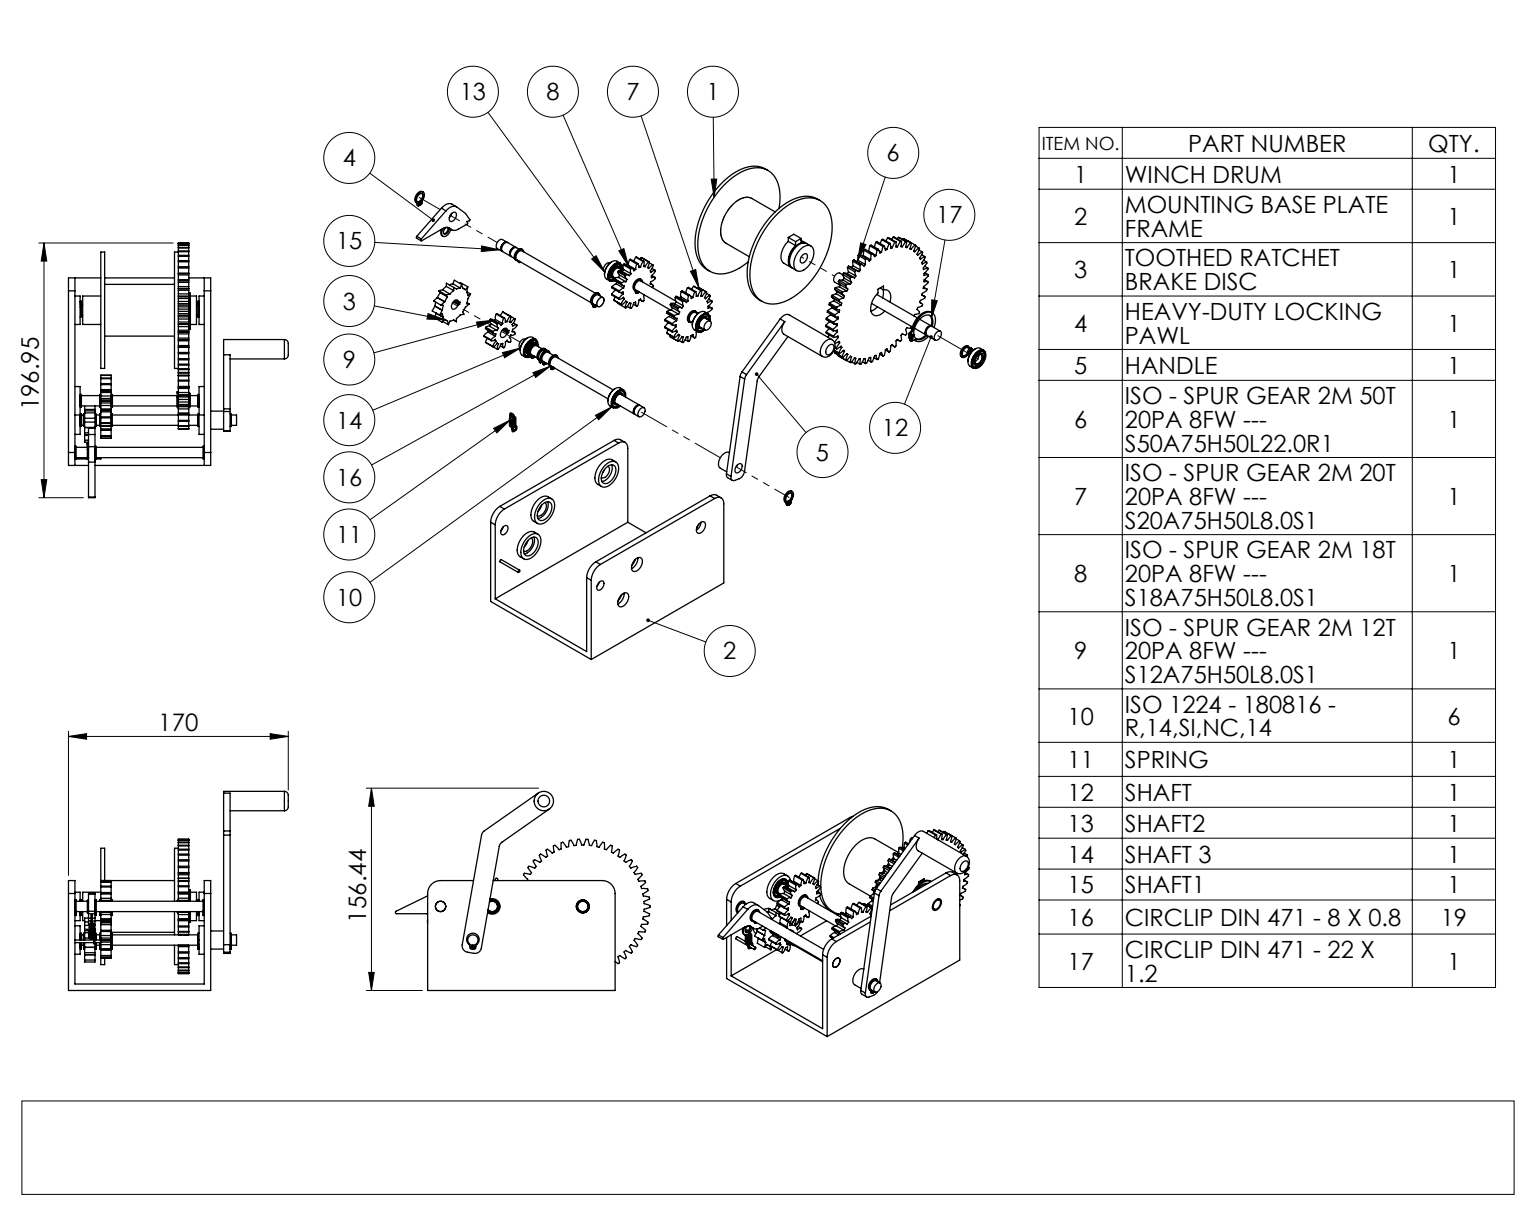
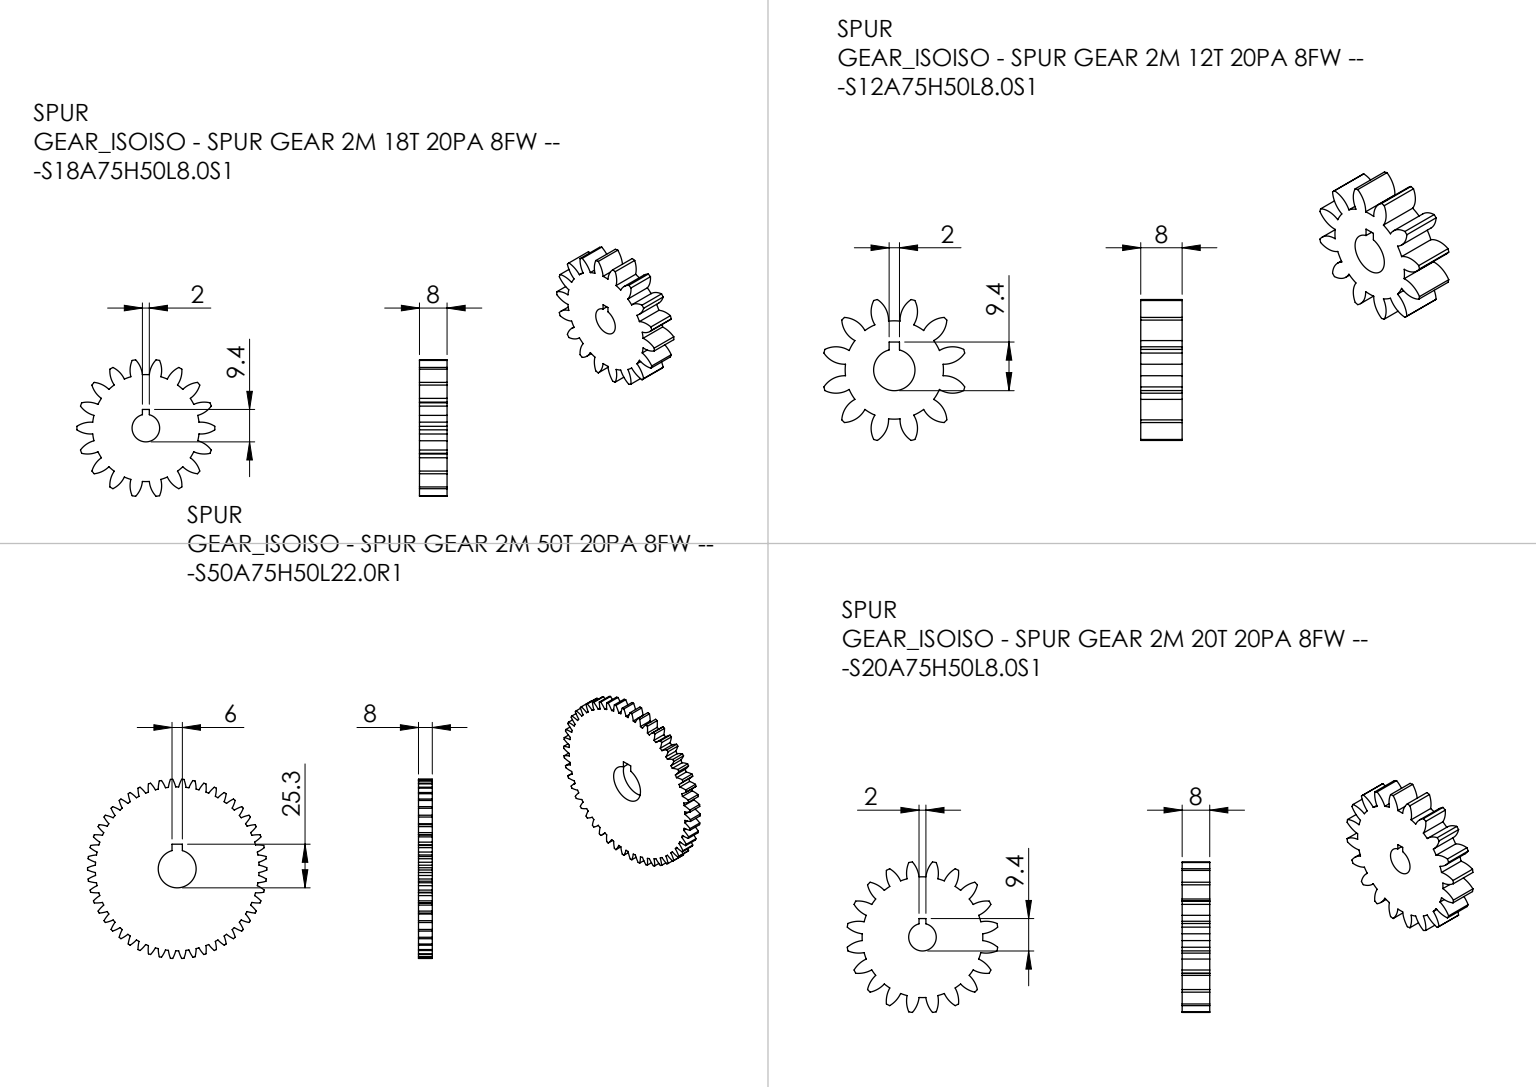
ISO-10303-21;
HEADER;
FILE_DESCRIPTION (('STEP AP214'),
    '1' );
FILE_NAME ('BR-594',
    '2026-09-28T15:49:00',
    ( '' ),
    ( '' ),
    'SwSTEP 2.0',
    'SolidWorks 2026',
    '' );
FILE_SCHEMA (( 'AUTOMOTIVE_DESIGN' ));
ENDSEC;

DATA;
#1 = CARTESIAN_POINT ( 'NONE',  ( 8.000000000000000000, -16.59870953437682672, 3.253005020243791456 ) ) ;
#2 = CARTESIAN_POINT ( 'NONE',  ( 8.000000000000000000, 0.000000000000000000, 0.000000000000000000 ) ) ;
#3 = EDGE_CURVE ( 'NONE', #21603, #30554, #20379, .T. ) ;
#4 = EDGE_LOOP ( 'NONE', ( #3245, #31755, #34673, #24973 ) ) ;
#5 = CARTESIAN_POINT ( 'NONE',  ( -34.00000000000000000, -114.0592624029313242, 6.003524454178450043 ) ) ;
#6 = EDGE_CURVE ( 'NONE', #33603, #20080, #10924, .T. ) ;
#7 = DIRECTION ( 'NONE',  ( -1.000000000000000000, 0.000000000000000000, 0.000000000000000000 ) ) ;
#8 = CYLINDRICAL_SURFACE ( 'NONE', #33227, 47.49900000000001654 ) ;
#9 = VERTEX_POINT ( 'NONE', #21941 ) ;
#10 = ORIENTED_EDGE ( 'NONE', *, *, #14256, .F. ) ;
#11 = DIRECTION ( 'NONE',  ( 1.000000000000000000, -0.000000000000000000, -0.000000000000000000 ) ) ;
#12 =( NAMED_UNIT ( * ) SI_UNIT ( $, .STERADIAN. ) SOLID_ANGLE_UNIT ( ) );
#13 = CARTESIAN_POINT ( 'NONE',  ( -12.55910585664919132, 0.7408941433508802188, -1.200000000000006617 ) ) ;
#14 = ORIENTED_EDGE ( 'NONE', *, *, #31358, .T. ) ;
#15 = ORIENTED_EDGE ( 'NONE', *, *, #2696, .T. ) ;
#16 = CARTESIAN_POINT ( 'NONE',  ( -35.50000000000000000, -112.5389594332240222, 2.818899826424027477 ) ) ;
#17 = DIRECTION ( 'NONE',  ( -1.000000000000000000, -0.000000000000000000, -0.000000000000000000 ) ) ;
#18 = VECTOR ( 'NONE', #20974, 1000.000000000000000 ) ;
#19 = ORIENTED_EDGE ( 'NONE', *, *, #4802, .F. ) ;
#20 = CARTESIAN_POINT ( 'NONE',  ( -35.50000000000000711, -114.9929510916434339, 11.38636890470581164 ) ) ;
#21 = EDGE_CURVE ( 'NONE', #11865, #28075, #4908, .T. ) ;
#22 = CARTESIAN_POINT ( 'NONE',  ( -34.50000000000000000, -113.9929510916434339, 12.17846912687782712 ) ) ;
#23 = CARTESIAN_POINT ( 'NONE',  ( 7.999999999999992895, 0.000000000000000000, 0.000000000000000000 ) ) ;
#24 = CARTESIAN_POINT ( 'NONE',  ( 7.999999999999992895, 13.56094713063570723, 50.20060470671747055 ) ) ;
#25 = CARTESIAN_POINT ( 'NONE',  ( -34.50000000000000000, -113.9929510916434339, 10.68227981832981044 ) ) ;
#26 = CARTESIAN_POINT ( 'NONE',  ( -38.99999693208653895, -114.9929510916434339, 12.62875129555797749 ) ) ;
#27 = CARTESIAN_POINT ( 'NONE',  ( -35.50000000000000711, -114.9860996047076895, 10.38555023491505835 ) ) ;
#28 = DIRECTION ( 'NONE',  ( 0.000000000000000000, 0.000000000000000000, 1.000000000000000000 ) ) ;
#29 = EDGE_CURVE ( 'NONE', #15669, #7819, #25865, .T. ) ;
#30 = VERTEX_POINT ( 'NONE', #8607 ) ;
#31 = ADVANCED_FACE ( 'NONE', ( #16880 ), #5577, .T. ) ;
#32 = ORIENTED_EDGE ( 'NONE', *, *, #23830, .T. ) ;
#33 = AXIS2_PLACEMENT_3D ( 'NONE', #19655, #6177, #11053 ) ;
#34 = EDGE_CURVE ( 'NONE', #41, #24879, #23867, .T. ) ;
#35 = DIRECTION ( 'NONE',  ( 0.000000000000000000, 0.000000000000000000, 1.000000000000000000 ) ) ;
#36 = DIRECTION ( 'NONE',  ( -1.174092375852890260E-15, 4.222049128630259891E-16, 1.000000000000000000 ) ) ;
#37 = ORIENTED_EDGE ( 'NONE', *, *, #7435, .F. ) ;
#38 = AXIS2_PLACEMENT_3D ( 'NONE', #16663, #5703, #35251 ) ;
#39 = ADVANCED_BREP_SHAPE_REPRESENTATION ( '', ( #22133, #21307 ), #32890 ) ;
#40 = FACE_OUTER_BOUND ( 'NONE', #7039, .T. ) ;
#41 = VERTEX_POINT ( 'NONE', #30237 ) ;
#42 = CARTESIAN_POINT ( 'NONE',  ( -35.50000000000000000, -113.2441867727860227, 0.9026824934337903672 ) ) ;
#43 = DIRECTION ( 'NONE',  ( -1.000000000000000000, 0.000000000000000000, 0.000000000000000000 ) ) ;
#44 = CARTESIAN_POINT ( 'NONE',  ( -37.97545270896701908, -113.5265240346955977, 3.847274454178448710 ) ) ;
#45 = CIRCLE ( 'NONE', #32841, 4.000000000000000000 ) ;
#46 = AXIS2_PLACEMENT_3D ( 'NONE', #19606, #14217, #25394 ) ;
#47 = DIRECTION ( 'NONE',  ( 0.000000000000000000, 0.000000000000000000, -1.000000000000000000 ) ) ;
#48 = ADVANCED_FACE ( 'NONE', ( #22956 ), #19423, .T. ) ;
#49 = ORIENTED_EDGE ( 'NONE', *, *, #14010, .T. ) ;
#50 = LINE ( 'NONE', #33346, #23380 ) ;
#51 = CARTESIAN_POINT ( 'NONE',  ( -35.50000000000000000, -116.2431927316855109, -2.224114562372550008 ) ) ;
#52 = VERTEX_POINT ( 'NONE', #30421 ) ;
#53 = ORIENTED_EDGE ( 'NONE', *, *, #22089, .T. ) ;
#54 = CARTESIAN_POINT ( 'NONE',  ( -39.02454729103295961, -114.7691647218148745, 8.159774454178448266 ) ) ;
#55 =( NAMED_UNIT ( * ) SI_UNIT ( $, .STERADIAN. ) SOLID_ANGLE_UNIT ( ) );
#56 = CARTESIAN_POINT ( 'NONE',  ( 55.00000000000000711, -25.98076211353320986, 88.99999999999994316 ) ) ;
#57 = ORIENTED_EDGE ( 'NONE', *, *, #32180, .F. ) ;
#58 = ORIENTED_EDGE ( 'NONE', *, *, #8163, .F. ) ;
#59 = CARTESIAN_POINT ( 'NONE',  ( -34.50000000000000000, -113.0140978167136581, -0.6247823525984268489 ) ) ;
#60 = DIRECTION ( 'NONE',  ( 0.000000000000000000, -0.3681245526846852467, 0.9297764858882484607 ) ) ;
#61 = PRODUCT_DEFINITION_CONTEXT ( 'detailed design', #10343, 'design' ) ;
#62 = CARTESIAN_POINT ( 'NONE',  ( 7.999999999999992895, 46.21320724403649649, 10.97699764141971102 ) ) ;
#63 = EDGE_CURVE ( 'NONE', #29341, #31925, #15789, .T. ) ;
#64 = FACE_BOUND ( 'NONE', #18708, .T. ) ;
#65 = CARTESIAN_POINT ( 'NONE',  ( -35.50000000000000000, -113.9929510916434339, 10.61627146648203990 ) ) ;
#66 = EDGE_CURVE ( 'NONE', #4339, #26513, #34817, .T. ) ;
#67 = DIRECTION ( 'NONE',  ( 1.226634733346697831E-16, 0.9659258262890664248, 0.2588190451025275673 ) ) ;
#68 = CARTESIAN_POINT ( 'NONE',  ( -55.00000000000000000, -25.98076211353320275, 84.99999999999994316 ) ) ;
#69 = CIRCLE ( 'NONE', #24242, 52.00000000000000711 ) ;
#70 = CARTESIAN_POINT ( 'NONE',  ( -34.50000000000000000, -113.0071371610607684, 2.888584676720006961 ) ) ;
#71 = CARTESIAN_POINT ( 'NONE',  ( -39.00000000000000000, -115.9929510916434481, 12.17846912687782179 ) ) ;
#72 = FACE_OUTER_BOUND ( 'NONE', #19048, .T. ) ;
#73 = CYLINDRICAL_SURFACE ( 'NONE', #12884, 22.00000000000000000 ) ;
#74 = EDGE_CURVE ( 'NONE', #4180, #540, #6597, .T. ) ;
#75 = DIRECTION ( 'NONE',  ( -1.000000000000000000, 0.000000000000000000, -0.000000000000000000 ) ) ;
#76 = ORIENTED_EDGE ( 'NONE', *, *, #2779, .T. ) ;
#77 = CARTESIAN_POINT ( 'NONE',  ( -35.50000000000000711, -114.1414532730574507, 9.517316564499758158 ) ) ;
#78 = CARTESIAN_POINT ( 'NONE',  ( 0.000000000000000000, 0.000000000000000000, -52.50000000000000000 ) ) ;
#79 = SURFACE_STYLE_USAGE ( .BOTH. , #8342 ) ;
#80 = ADVANCED_FACE ( 'NONE', ( #27547, #5915 ), #12161, .T. ) ;
#81 = CARTESIAN_POINT ( 'NONE',  ( 0.000000000000000000, 0.000000000000000000, -33.50000000000000711 ) ) ;
#82 = CARTESIAN_POINT ( 'NONE',  ( -3.799999999999999822, 4.382607293638566128E-16, -21.89999999999999858 ) ) ;
#83 = ORIENTED_EDGE ( 'NONE', *, *, #30527, .F. ) ;
#84 = LINE ( 'NONE', #13940, #22802 ) ;
#85 = CARTESIAN_POINT ( 'NONE',  ( -46.00000000000000000, 0.000000000000000000, 70.00000000000000000 ) ) ;
#86 = CARTESIAN_POINT ( 'NONE',  ( 0.000000000000000000, 43.83938735307269496, 18.28286404005814703 ) ) ;
#87 = DIRECTION ( 'NONE',  ( 0.000000000000000000, 0.000000000000000000, -1.000000000000000000 ) ) ;
#88 = CYLINDRICAL_SURFACE ( 'NONE', #8916, 47.49900000000001654 ) ;
#89 = CYLINDRICAL_SURFACE ( 'NONE', #22796, 4.000000000000000000 ) ;
#90 = ORIENTED_EDGE ( 'NONE', *, *, #30599, .T. ) ;
#91 = SURFACE_STYLE_FILL_AREA ( #262 ) ;
#92 = DIRECTION ( 'NONE',  ( 0.000000000000000000, 0.000000000000000000, 1.000000000000000000 ) ) ;
#93 = DIRECTION ( 'NONE',  ( -1.000000000000000000, 0.000000000000000000, -0.000000000000000000 ) ) ;
#94 = EDGE_LOOP ( 'NONE', ( #19216, #26930 ) ) ;
#95 = CARTESIAN_POINT ( 'NONE',  ( -36.64504884055821776, -112.9754527089670688, 6.715225545821551734 ) ) ;
#96 = ORIENTED_EDGE ( 'NONE', *, *, #21612, .T. ) ;
#97 = AXIS2_PLACEMENT_3D ( 'NONE', #12823, #1667, #2025 ) ;
#98 =( GEOMETRIC_REPRESENTATION_CONTEXT ( 3 ) GLOBAL_UNCERTAINTY_ASSIGNED_CONTEXT ( ( #24807 ) ) GLOBAL_UNIT_ASSIGNED_CONTEXT ( ( #15841, #16194, #16020 ) ) REPRESENTATION_CONTEXT ( 'NONE', 'WORKASPACE' ) );
#99 = AXIS2_PLACEMENT_3D ( 'NONE', #28579, #20265, #1214 ) ;
#100 = SURFACE_STYLE_FILL_AREA ( #24773 ) ;
#101 = ORIENTED_EDGE ( 'NONE', *, *, #74, .T. ) ;
#102 = EDGE_LOOP ( 'NONE', ( #28338, #13792, #13740, #22838 ) ) ;
#103 = DIRECTION ( 'NONE',  ( 0.000000000000000000, 0.000000000000000000, 1.000000000000000000 ) ) ;
#104 = ADVANCED_FACE ( 'NONE', ( #25008 ), #22116, .T. ) ;
#105 = CARTESIAN_POINT ( 'NONE',  ( 0.1085714285714300953, -3.798448662927791819, -0.7999999999999951594 ) ) ;
#106 = AXIS2_PLACEMENT_3D ( 'NONE', #28368, #3711, #14664 ) ;
#107 = EDGE_CURVE ( 'NONE', #5795, #7932, #19266, .T. ) ;
#108 = CARTESIAN_POINT ( 'NONE',  ( -35.50000000000000711, -114.0882517521923489, 9.510534276948430232 ) ) ;
#109 = FACE_OUTER_BOUND ( 'NONE', #11807, .T. ) ;
#110 = CARTESIAN_POINT ( 'NONE',  ( 0.000000000000000000, 0.000000000000000000, -0.7999999999999951594 ) ) ;
#111 = DIRECTION ( 'NONE',  ( -1.174092375852890260E-15, 4.222049128630259891E-16, 1.000000000000000000 ) ) ;
#112 = DIRECTION ( 'NONE',  ( -1.000000000000000000, 0.000000000000000000, 0.000000000000000000 ) ) ;
#113 = CARTESIAN_POINT ( 'NONE',  ( 3.983177536951269193, -13.66651769228263724, -1.200000000000006617 ) ) ;
#114 = CIRCLE ( 'NONE', #34046, 4.000000000000000000 ) ;
#115 = CARTESIAN_POINT ( 'NONE',  ( -35.87745010033553683, -115.9929510916434481, 14.11371147303761475 ) ) ;
#117 = DIRECTION ( 'NONE',  ( -1.000000000000000000, 0.000000000000000000, 0.000000000000000000 ) ) ;
#116 = AXIS2_PLACEMENT_3D ( 'NONE', #21705, #19183, #32879 ) ;
#118 = CARTESIAN_POINT ( 'NONE',  ( 7.999999999999992895, -46.90537658765327933, -2.727856614654800005 ) ) ;
#119 = DIRECTION ( 'NONE',  ( 1.000000000000000000, 0.000000000000000000, 0.000000000000000000 ) ) ;
#120 = CARTESIAN_POINT ( 'NONE',  ( 0.000000000000000000, 0.000000000000000000, -50.00000000000000000 ) ) ;
#121 = CARTESIAN_POINT ( 'NONE',  ( 8.000000000000000000, -6.085920226790910270, -15.78165944574524637 ) ) ;
#122 = FILL_AREA_STYLE_COLOUR ( '', #22409 ) ;
#123 = ORIENTED_EDGE ( 'NONE', *, *, #11203, .T. ) ;
#124 = CARTESIAN_POINT ( 'NONE',  ( -35.62769128460905677, -112.5438815906447729, 6.808975545821550845 ) ) ;
#125 = FACE_OUTER_BOUND ( 'NONE', #23551, .T. ) ;
#126 = LINE ( 'NONE', #14327, #30319 ) ;
#127 = DIRECTION ( 'NONE',  ( 0.000000000000000000, 0.000000000000000000, 1.000000000000000000 ) ) ;
#128 = VERTEX_POINT ( 'NONE', #22295 ) ;
#129 = COLOUR_RGB ( '', 0.40784314, 0.44705882, 0.49803922) ;
#130 = ORIENTED_EDGE ( 'NONE', *, *, #26286, .T. ) ;
#131 = DIRECTION ( 'NONE',  ( 3.154042683594195121E-16, -1.000000000000000000, 0.000000000000000000 ) ) ;
#132 = DIRECTION ( 'NONE',  ( -1.000000000000000000, 0.000000000000000000, 0.000000000000000000 ) ) ;
#133 = ORIENTED_EDGE ( 'NONE', *, *, #25065, .T. ) ;
#134 = ORIENTED_EDGE ( 'NONE', *, *, #4280, .T. ) ;
#135 = LINE ( 'NONE', #21918, #20318 ) ;
#136 = AXIS2_PLACEMENT_3D ( 'NONE', #5268, #29577, #7420 ) ;
#137 = FACE_BOUND ( 'NONE', #21992, .T. ) ;
#138 = VECTOR ( 'NONE', #11051, 999.9999999999998863 ) ;
#139 = DIRECTION ( 'NONE',  ( 0.000000000000000000, 0.000000000000000000, 1.000000000000000000 ) ) ;
#140 = DIRECTION ( 'NONE',  ( -1.000000000000000000, 0.000000000000000000, 0.000000000000000000 ) ) ;
#141 = ORIENTED_EDGE ( 'NONE', *, *, #2856, .F. ) ;
#142 = EDGE_LOOP ( 'NONE', ( #28421, #17559, #31221, #701 ) ) ;
#143 = EDGE_CURVE ( 'NONE', #14032, #9695, #27885, .T. ) ;
#144 = DIRECTION ( 'NONE',  ( -1.000000000000000000, 0.000000000000000000, -0.000000000000000000 ) ) ;
#145 = DIRECTION ( 'NONE',  ( -1.000000000000000000, 0.000000000000000000, 0.000000000000000000 ) ) ;
#146 = EDGE_LOOP ( 'NONE', ( #18691, #20967, #34067, #15002, #19215, #15839 ) ) ;
#147 = CARTESIAN_POINT ( 'NONE',  ( 0.000000000000000000, -3.968388925834656966, -21.63912866391144618 ) ) ;
#148 = AXIS2_PLACEMENT_3D ( 'NONE', #26646, #23213, #28979 ) ;
#149 = CARTESIAN_POINT ( 'NONE',  ( -34.50000000000000000, -113.4307644833805000, -1.624782352598427959 ) ) ;
#150 = CIRCLE ( 'NONE', #20253, 10.49999999999999645 ) ;
#151 = CARTESIAN_POINT ( 'NONE',  ( -39.00000000000000711, -114.9929510916434339, 12.60752341388803721 ) ) ;
#152 = CARTESIAN_POINT ( 'NONE',  ( -35.50000000000000000, -113.9929510916434339, 10.50625754673586876 ) ) ;
#153 = CARTESIAN_POINT ( 'NONE',  ( 8.000000000000000000, 8.605879768205236147, 12.89022243466711615 ) ) ;
#154 = EDGE_CURVE ( 'NONE', #9833, #15465, #27896, .T. ) ;
#155 = CARTESIAN_POINT ( 'NONE',  ( -36.03125000000004263, -114.9929510916434339, 14.11852480586264846 ) ) ;
#156 = CARTESIAN_POINT ( 'NONE',  ( 65.00000000000001421, 81.48267994499606459, 30.15054357219658954 ) ) ;
#157 = DIRECTION ( 'NONE',  ( 0.000000000000000000, 0.000000000000000000, 1.000000000000000000 ) ) ;
#158 = DIRECTION ( 'NONE',  ( 1.000000000000000000, 0.000000000000000000, 0.000000000000000000 ) ) ;
#159 = DIRECTION ( 'NONE',  ( 0.000000000000000000, -0.9510565162951564178, 0.3090169943749385140 ) ) ;
#160 = CARTESIAN_POINT ( 'NONE',  ( -39.49999999999999289, -4.676198662292047281, 104.0227405789415798 ) ) ;
#161 = AXIS2_PLACEMENT_3D ( 'NONE', #25822, #31910, #29039 ) ;
#162 = EDGE_LOOP ( 'NONE', ( #12105, #9700 ) ) ;
#163 = AXIS2_PLACEMENT_3D ( 'NONE', #32400, #32750, #18355 ) ;
#164 = CARTESIAN_POINT ( 'NONE',  ( 0.000000000000000000, 37.91532898920963390, -28.61088654061597225 ) ) ;
#165 = EDGE_LOOP ( 'NONE', ( #34019, #14736, #9837, #7104, #34372 ) ) ;
#166 = VECTOR ( 'NONE', #13952, 1000.000000000000000 ) ;
#167 = CARTESIAN_POINT ( 'NONE',  ( -39.16322519054179452, -116.0794154965774823, 6.566024454178448266 ) ) ;
#168 = DIRECTION ( 'NONE',  ( 0.000000000000000000, -2.423959199780483078E-15, 1.000000000000000000 ) ) ;
#169 = VERTEX_POINT ( 'NONE', #28551 ) ;
#170 = EDGE_LOOP ( 'NONE', ( #28975, #27946, #5714, #16850, #18978 ) ) ;
#171 = DIRECTION ( 'NONE',  ( 1.000000000000000000, 0.000000000000000000, 0.000000000000000000 ) ) ;
#172 = CARTESIAN_POINT ( 'NONE',  ( 7.999999999999992895, 0.000000000000000000, 0.000000000000000000 ) ) ;
#173 = ORIENTED_EDGE ( 'NONE', *, *, #35130, .T. ) ;
#174 = CARTESIAN_POINT ( 'NONE',  ( -39.07941549657748936, -111.8367748094582055, 6.941024454178450043 ) ) ;
#175 = CIRCLE ( 'NONE', #10540, 6.000000000000002665 ) ;
#176 = CARTESIAN_POINT ( 'NONE',  ( 8.000000000000000000, 5.482169781019050170, -16.00140663693117560 ) ) ;
#177 = DIRECTION ( 'NONE',  ( -1.000000000000000000, 0.000000000000000000, 0.000000000000000000 ) ) ;
#179 = ORIENTED_EDGE ( 'NONE', *, *, #27489, .F. ) ;
#178 = CIRCLE ( 'NONE', #22577, 4.000000000000000000 ) ;
#180 = VERTEX_POINT ( 'NONE', #14854 ) ;
#181 = CARTESIAN_POINT ( 'NONE',  ( 7.999999999999992895, -37.91532898920942074, 28.61088654061626357 ) ) ;
#182 = PRESENTATION_STYLE_ASSIGNMENT (( #24683 ) ) ;
#183 = CARTESIAN_POINT ( 'NONE',  ( -90.00000000000002842, 0.000000000000000000, 6.938893903907228378E-15 ) ) ;
#184 = ORIENTED_EDGE ( 'NONE', *, *, #5407, .T. ) ;
#185 = VERTEX_POINT ( 'NONE', #4789 ) ;
#186 = CARTESIAN_POINT ( 'NONE',  ( -35.50000000000000000, -111.8727710936879589, 2.535339294948415922 ) ) ;
#187 = VECTOR ( 'NONE', #26891, 1000.000000000000000 ) ;
#188 = EDGE_CURVE ( 'NONE', #23209, #29518, #12364, .T. ) ;
#189 = VECTOR ( 'NONE', #29534, 1000.000000000000000 ) ;
#190 = ADVANCED_FACE ( 'NONE', ( #12334 ), #23311, .F. ) ;
#191 = DIRECTION ( 'NONE',  ( 0.000000000000000000, 0.000000000000000000, 1.000000000000000000 ) ) ;
#192 = VERTEX_POINT ( 'NONE', #6754 ) ;
#193 = CARTESIAN_POINT ( 'NONE',  ( -35.50160444427493189, -114.9929510916434339, 12.65937477241749853 ) ) ;
#194 = CARTESIAN_POINT ( 'NONE',  ( -36.03125000000003553, -113.9929510916434339, 14.11852480586265024 ) ) ;
#195 = DIRECTION ( 'NONE',  ( 1.000000000000000000, -0.000000000000000000, -0.000000000000000000 ) ) ;
#196 = LINE ( 'NONE', #5955, #10522 ) ;
#197 = EDGE_CURVE ( 'NONE', #14850, #9043, #11214, .T. ) ;
#198 = CARTESIAN_POINT ( 'NONE',  ( -34.50000000000000000, -113.9929510916434339, 10.50625754673588474 ) ) ;
#199 = CARTESIAN_POINT ( 'NONE',  ( -39.00000000000000711, -114.9929510916434339, 11.21034663311206181 ) ) ;
#200 = CARTESIAN_POINT ( 'NONE',  ( -35.50000000000000711, -114.9492820284331742, 10.20776876943783940 ) ) ;
#201 = DIRECTION ( 'NONE',  ( 0.000000000000000000, 0.000000000000000000, -1.000000000000000000 ) ) ;
#202 = CIRCLE ( 'NONE', #8824, 0.5000000000000004441 ) ;
#203 = AXIS2_PLACEMENT_3D ( 'NONE', #2270, #7808, #27270 ) ;
#204 = DIRECTION ( 'NONE',  ( -1.000000000000000000, -0.000000000000000000, 0.000000000000000000 ) ) ;
#205 = ORIENTED_EDGE ( 'NONE', *, *, #23774, .F. ) ;
#206 = EDGE_LOOP ( 'NONE', ( #28394, #8003, #20134, #21793 ) ) ;
#207 = DIRECTION ( 'NONE',  ( 0.000000000000000000, 0.000000000000000000, 1.000000000000000000 ) ) ;
#208 = CARTESIAN_POINT ( 'NONE',  ( 8.000000000000000000, 0.000000000000000000, 20.00000000000000000 ) ) ;
#209 = VERTEX_POINT ( 'NONE', #26030 ) ;
#210 = CARTESIAN_POINT ( 'NONE',  ( 5.400000000000015454, -1.000000000000002220, -22.00000000000000000 ) ) ;
#211 = VERTEX_POINT ( 'NONE', #18081 ) ;
#212 = AXIS2_PLACEMENT_3D ( 'NONE', #10093, #32066, #18373 ) ;
#213 = CARTESIAN_POINT ( 'NONE',  ( -35.50000000000000000, -113.0140978167138712, 0.8127176474015720409 ) ) ;
#214 = CARTESIAN_POINT ( 'NONE',  ( -34.49999999999998579, -13.17619866229204284, 90.66066734786082293 ) ) ;
#215 = CARTESIAN_POINT ( 'NONE',  ( -36.11231047232249125, -112.0245472910329880, 5.722274454178448266 ) ) ;
#216 = DIRECTION ( 'NONE',  ( 0.000000000000000000, -0.4387576694191721027, 0.8986054237126862576 ) ) ;
#217 = ADVANCED_FACE ( 'NONE', ( #9811 ), #28733, .T. ) ;
#218 = ORIENTED_EDGE ( 'NONE', *, *, #1180, .F. ) ;
#219 = VECTOR ( 'NONE', #13826, 1000.000000000000000 ) ;
#220 = DIRECTION ( 'NONE',  ( -0.000000000000000000, 1.000000000000000000, 0.000000000000000000 ) ) ;
#221 = CARTESIAN_POINT ( 'NONE',  ( -35.50000000000000711, -112.8356783780338759, 1.859636627348750348 ) ) ;
#222 = ORIENTED_EDGE ( 'NONE', *, *, #22015, .T. ) ;
#223 = VERTEX_POINT ( 'NONE', #1907 ) ;
#224 = CARTESIAN_POINT ( 'NONE',  ( -38.97545270896704039, -113.1123104723225197, 8.347274454178448266 ) ) ;
#225 = LINE ( 'NONE', #30656, #27926 ) ;
#226 = EDGE_LOOP ( 'NONE', ( #27642, #13433, #11030, #13764 ) ) ;
#227 = ORIENTED_EDGE ( 'NONE', *, *, #23757, .T. ) ;
#228 = CARTESIAN_POINT ( 'NONE',  ( -34.50000000000000000, -113.6318576702834804, 1.956056246348823580 ) ) ;
#229 = CARTESIAN_POINT ( 'NONE',  ( 0.000000000000000000, 9.919332006307222116, 5.363026430117163734 ) ) ;
#230 = EDGE_CURVE ( 'NONE', #16800, #15848, #17909, .T. ) ;
#231 = EDGE_CURVE ( 'NONE', #22807, #14329, #9992, .T. ) ;
#232 = EDGE_CURVE ( 'NONE', #25838, #30814, #21546, .T. ) ;
#233 = DIRECTION ( 'NONE',  ( 0.000000000000000000, 0.000000000000000000, -1.000000000000000000 ) ) ;
#234 = AXIS2_PLACEMENT_3D ( 'NONE', #3071, #14027, #25022 ) ;
#235 = CARTESIAN_POINT ( 'NONE',  ( -35.50000000000000000, -113.9929510916434339, 11.38636890470581164 ) ) ;
#236 = AXIS2_PLACEMENT_3D ( 'NONE', #6665, #9551, #20518 ) ;
#237 = FACE_OUTER_BOUND ( 'NONE', #27820, .T. ) ;
#238 = DIRECTION ( 'NONE',  ( 1.000000000000000000, -0.000000000000000000, -0.000000000000000000 ) ) ;
#239 = ADVANCED_FACE ( 'NONE', ( #26385 ), #21143, .F. ) ;
#240 = CARTESIAN_POINT ( 'NONE',  ( -34.50000000000000000, -111.1014359431343905, 1.472195201997948510 ) ) ;
#241 = EDGE_CURVE ( 'NONE', #27557, #21748, #15191, .T. ) ;
#242 = CARTESIAN_POINT ( 'NONE',  ( -37.51022648969539119, -115.9929510916434481, 14.11852173794918563 ) ) ;
#243 = UNCERTAINTY_MEASURE_WITH_UNIT (LENGTH_MEASURE( 1.000000000000000082E-05 ), #22968, 'distance_accuracy_value', 'NONE');
#244 = FACE_BOUND ( 'NONE', #10635, .T. ) ;
#245 = DIRECTION ( 'NONE',  ( 0.000000000000000000, 0.000000000000000000, 1.000000000000000000 ) ) ;
#246 = EDGE_LOOP ( 'NONE', ( #18364, #3419, #5510, #32868 ) ) ;
#247 = CARTESIAN_POINT ( 'NONE',  ( -37.99999897736217491, -115.9929510916434481, 12.62466071271733092 ) ) ;
#248 = LINE ( 'NONE', #32677, #17648 ) ;
#249 = LINE ( 'NONE', #5836, #8196 ) ;
#250 = DIRECTION ( 'NONE',  ( 1.000000000000000000, -0.000000000000000000, -0.000000000000000000 ) ) ;
#251 = VERTEX_POINT ( 'NONE', #7468 ) ;
#252 = DIRECTION ( 'NONE',  ( 0.000000000000000000, 0.000000000000000000, 1.000000000000000000 ) ) ;
#253 = CARTESIAN_POINT ( 'NONE',  ( 46.00000000000000000, 0.000000000000000000, 0.000000000000000000 ) ) ;
#254 = CARTESIAN_POINT ( 'NONE',  ( 0.000000000000000000, -9.604183132802424083, 5.908880290975512928 ) ) ;
#255 = CARTESIAN_POINT ( 'NONE',  ( 0.000000000000000000, -2.710505431213761085E-17, -45.89999999999999858 ) ) ;
#256 = ITEM_DEFINED_TRANSFORMATION ( 'NONE', 'NONE', #2309,  #21307 ) ;
#257 = FACE_OUTER_BOUND ( 'NONE', #21375, .T. ) ;
#258 = DIRECTION ( 'NONE',  ( -1.000000000000000000, 0.000000000000000000, 0.000000000000000000 ) ) ;
#259 = ADVANCED_FACE ( 'NONE', ( #12521 ), #20953, .T. ) ;
#260 = ORIENTED_EDGE ( 'NONE', *, *, #3308, .F. ) ;
#261 = AXIS2_PLACEMENT_3D ( 'NONE', #4805, #2292, #35227 ) ;
#262 = FILL_AREA_STYLE ('',( #8710 ) ) ;
#263 = CARTESIAN_POINT ( 'NONE',  ( 0.000000000000000000, -2.710505431213761085E-17, 54.99999999999999289 ) ) ;
#264 = EDGE_CURVE ( 'NONE', #30567, #34766, #2139, .T. ) ;
#265 = CARTESIAN_POINT ( 'NONE',  ( -2.600000000000004530, -12.74999999999999822, -1.386669559958809814E-29 ) ) ;
#266 = ORIENTED_EDGE ( 'NONE', *, *, #9713, .F. ) ;
#267 = CARTESIAN_POINT ( 'NONE',  ( -37.74901162816868805, -113.3347980657955958, 4.933975545821551734 ) ) ;
#268 = ORIENTED_EDGE ( 'NONE', *, *, #6401, .F. ) ;
#269 = EDGE_CURVE ( 'NONE', #16003, #16053, #12703, .T. ) ;
#270 = AXIS2_PLACEMENT_3D ( 'NONE', #1715, #16715, #22475 ) ;
#271 = ORIENTED_EDGE ( 'NONE', *, *, #33716, .F. ) ;
#272 = VERTEX_POINT ( 'NONE', #18447 ) ;
#273 = CARTESIAN_POINT ( 'NONE',  ( -21.15833593587365513, -18.77980021920990694, 100.4724318643354053 ) ) ;
#274 = EDGE_CURVE ( 'NONE', #16735, #21654, #4432, .T. ) ;
#275 = EDGE_CURVE ( 'NONE', #2191, #19467, #3280, .T. ) ;
#276 = CARTESIAN_POINT ( 'NONE',  ( -35.50000000000000000, -117.0140978167138854, 0.6252176474015650465 ) ) ;
#277 = DIRECTION ( 'NONE',  ( -1.000000000000000000, 0.000000000000000000, 0.000000000000000000 ) ) ;
#278 = VECTOR ( 'NONE', #10313, 1000.000000000000000 ) ;
#279 = FACE_OUTER_BOUND ( 'NONE', #7139, .T. ) ;
#280 = CARTESIAN_POINT ( 'NONE',  ( 0.000000000000000000, 0.000000000000000000, 0.000000000000000000 ) ) ;
#281 = DIRECTION ( 'NONE',  ( 1.000000000000000000, -4.524158825347490025E-15, -1.177133787269970298E-15 ) ) ;
#282 = EDGE_CURVE ( 'NONE', #12434, #12602, #7107, .T. ) ;
#283 = CARTESIAN_POINT ( 'NONE',  ( -42.49999999999999289, -34.23950567274748380, 96.30456345124107997 ) ) ;
#284 = CARTESIAN_POINT ( 'NONE',  ( 29.99999999999999289, 1.244980450007031636E-14, -3.000000000000002665 ) ) ;
#285 = VECTOR ( 'NONE', #5532, 1000.000000000000000 ) ;
#286 = DIRECTION ( 'NONE',  ( -1.000000000000000000, 0.000000000000000000, 0.000000000000000000 ) ) ;
#287 = CARTESIAN_POINT ( 'NONE',  ( -38.81062062679291813, -115.9929510916434481, 13.37409560816442244 ) ) ;
#288 = DIRECTION ( 'NONE',  ( -1.000000000000000000, 0.000000000000000000, 0.000000000000000000 ) ) ;
#289 = VECTOR ( 'NONE', #25912, 1000.000000000000000 ) ;
#290 = CYLINDRICAL_SURFACE ( 'NONE', #33735, 20.00000000000000355 ) ;
#291 = DIRECTION ( 'NONE',  ( 1.000000000000000000, 0.000000000000000000, 0.000000000000000000 ) ) ;
#292 = DIRECTION ( 'NONE',  ( -1.000000000000000000, 0.000000000000000000, 0.000000000000000000 ) ) ;
#293 = CIRCLE ( 'NONE', #26762, 20.00000000000001066 ) ;
#294 = CARTESIAN_POINT ( 'NONE',  ( -42.49999999999999289, -25.98076211353322051, 84.99999999999992895 ) ) ;
#295 = ORIENTED_EDGE ( 'NONE', *, *, #4026, .T. ) ;
#296 = CARTESIAN_POINT ( 'NONE',  ( -37.88768952767750875, -112.0245472910329880, 9.527725545821557063 ) ) ;
#297 = FACE_OUTER_BOUND ( 'NONE', #4749, .T. ) ;
#298 = CARTESIAN_POINT ( 'NONE',  ( -34.49999999999998579, -28.81745899286249823, 74.41330312067046293 ) ) ;
#299 = DIRECTION ( 'NONE',  ( -1.000000000000000000, -0.000000000000000000, -0.000000000000000000 ) ) ;
#300 = ADVANCED_FACE ( 'NONE', ( #12882 ), #23862, .F. ) ;
#301 = ORIENTED_EDGE ( 'NONE', *, *, #5401, .F. ) ;
#302 = AXIS2_PLACEMENT_3D ( 'NONE', #13367, #4574, #23816 ) ;
#303 = EDGE_LOOP ( 'NONE', ( #1691, #1216, #1468, #3078 ) ) ;
#304 = EDGE_CURVE ( 'NONE', #15866, #20180, #29503, .T. ) ;
#305 = CARTESIAN_POINT ( 'NONE',  ( -21.15833593587365513, -33.18172400785640264, 69.52756813566438154 ) ) ;
#306 = DIRECTION ( 'NONE',  ( -1.000000000000000000, 0.000000000000000000, 0.000000000000000000 ) ) ;
#307 = ORIENTED_EDGE ( 'NONE', *, *, #12809, .F. ) ;
#308 = ORIENTED_EDGE ( 'NONE', *, *, #26431, .T. ) ;
#309 = PLANE ( 'NONE',  #1960 ) ;
#310 = VECTOR ( 'NONE', #1724, 1000.000000000000000 ) ;
#311 = PLANE ( 'NONE',  #8495 ) ;
#312 = EDGE_CURVE ( 'NONE', #5963, #29170, #3617, .T. ) ;
#313 = EDGE_CURVE ( 'NONE', #20125, #14882, #23736, .T. ) ;
#314 = DIRECTION ( 'NONE',  ( 1.000000000000000000, 0.000000000000000000, 0.000000000000000000 ) ) ;
#315 = AXIS2_PLACEMENT_3D ( 'NONE', #2102, #4970, #28914 ) ;
#316 = CARTESIAN_POINT ( 'NONE',  ( -4.000000000000000000, 0.000000000000000000, 55.00000000000000000 ) ) ;
#317 = ORIENTED_EDGE ( 'NONE', *, *, #1121, .T. ) ;
#318 = ORIENTED_EDGE ( 'NONE', *, *, #12144, .F. ) ;
#319 = CARTESIAN_POINT ( 'NONE',  ( 8.000000000000000000, 0.000000000000000000, 0.000000000000000000 ) ) ;
#320 = CARTESIAN_POINT ( 'NONE',  ( 7.999999999999992895, 0.000000000000000000, 0.000000000000000000 ) ) ;
#321 = ORIENTED_EDGE ( 'NONE', *, *, #9480, .F. ) ;
#322 = DIRECTION ( 'NONE',  ( 0.000000000000000000, 0.6427876096865349220, 0.7660444431189816772 ) ) ;
#323 = AXIS2_PLACEMENT_3D ( 'NONE', #35472, #10977, #16174 ) ;
#324 = CARTESIAN_POINT ( 'NONE',  ( -34.50000000000000000, -115.0795240838853886, -1.623175561345890472 ) ) ;
#325 = CARTESIAN_POINT ( 'NONE',  ( -38.99999693208653895, -114.9929510916434339, 12.62875129555797749 ) ) ;
#326 = CARTESIAN_POINT ( 'NONE',  ( -35.50000000000000000, -113.9929510916433060, 10.50625754673589540 ) ) ;
#327 = CARTESIAN_POINT ( 'NONE',  ( 50.00005079999998969, 5.400000000000098943, 1.000000000000000888 ) ) ;
#328 = CARTESIAN_POINT ( 'NONE',  ( -34.50481333282507279, -114.9929510916434339, 12.74107470552716492 ) ) ;
#329 = CARTESIAN_POINT ( 'NONE',  ( 0.000000000000000000, -45.78515115856053797, 12.64416602183649019 ) ) ;
#330 = CARTESIAN_POINT ( 'NONE',  ( 50.00000000000000000, 0.000000000000000000, 59.00000000000000000 ) ) ;
#331 = CARTESIAN_POINT ( 'NONE',  ( 50.00005079999998969, 5.400000000000029665, -1.000000000000000888 ) ) ;
#332 = DIRECTION ( 'NONE',  ( 1.000000000000000000, -5.339440136655842133E-16, -1.047965281155519420E-16 ) ) ;
#333 = DIRECTION ( 'NONE',  ( -1.000000000000000000, 0.000000000000000000, 0.000000000000000000 ) ) ;
#334 = VERTEX_POINT ( 'NONE', #10530 ) ;
#335 = DIRECTION ( 'NONE',  ( -1.000000000000000000, 0.000000000000000000, 0.000000000000000000 ) ) ;
#336 = ORIENTED_EDGE ( 'NONE', *, *, #17121, .F. ) ;
#337 = CARTESIAN_POINT ( 'NONE',  ( -33.97545270896702618, -112.8166217158120475, 5.909774454178450931 ) ) ;
#338 = AXIS2_PLACEMENT_3D ( 'NONE', #9593, #20561, #17688 ) ;
#339 = DIRECTION ( 'NONE',  ( -1.000000000000000000, -1.734723475976807094E-16, 0.000000000000000000 ) ) ;
#340 = VECTOR ( 'NONE', #10135, 1000.000000000000000 ) ;
#341 = CARTESIAN_POINT ( 'NONE',  ( -35.50000000000000711, -115.6286452741999113, -1.424448457485488095 ) ) ;
#342 = VERTEX_POINT ( 'NONE', #32678 ) ;
#343 = ORIENTED_EDGE ( 'NONE', *, *, #6840, .F. ) ;
#344 = CIRCLE ( 'NONE', #20442, 11.00000000000000000 ) ;
#345 = ADVANCED_FACE ( 'NONE', ( #24395 ), #13584, .T. ) ;
#346 = FILL_AREA_STYLE ('',( #33832 ) ) ;
#347 = CARTESIAN_POINT ( 'NONE',  ( 0.000000000000000000, 0.000000000000000000, 49.10000000000000142 ) ) ;
#348 = EDGE_LOOP ( 'NONE', ( #11431, #30900, #20303, #6750 ) ) ;
#349 = AXIS2_PLACEMENT_3D ( 'NONE', #33743, #25292, #25111 ) ;
#350 = CIRCLE ( 'NONE', #918, 6.984000000000015085 ) ;
#351 = DIRECTION ( 'NONE',  ( -1.000000000000000000, 0.000000000000000000, 0.000000000000000000 ) ) ;
#352 = VERTEX_POINT ( 'NONE', #8172 ) ;
#353 = ORIENTED_EDGE ( 'NONE', *, *, #11463, .F. ) ;
#354 = CARTESIAN_POINT ( 'NONE',  ( 2.000000000000001776, 0.000000000000000000, 0.000000000000000000 ) ) ;
#355 = CARTESIAN_POINT ( 'NONE',  ( 7.999999999999992895, 0.000000000000000000, 0.000000000000000000 ) ) ;
#356 = ORIENTED_EDGE ( 'NONE', *, *, #3793, .T. ) ;
#357 = ORIENTED_EDGE ( 'NONE', *, *, #10887, .T. ) ;
#358 = CARTESIAN_POINT ( 'NONE',  ( -35.50000000000000000, -112.3070160848889429, 2.749963775944984867 ) ) ;
#359 = AXIS2_PLACEMENT_3D ( 'NONE', #30031, #5369, #29856 ) ;
#360 = ORIENTED_EDGE ( 'NONE', *, *, #19402, .F. ) ;
#361 = CARTESIAN_POINT ( 'NONE',  ( -35.83891589277640577, -114.9929510916434339, 13.09299768411358222 ) ) ;
#362 = AXIS2_PLACEMENT_3D ( 'NONE', #20190, #31196, #14810 ) ;
#363 = VECTOR ( 'NONE', #32529, 1000.000000000000000 ) ;
#364 = VECTOR ( 'NONE', #24765, 1000.000000000000000 ) ;
#365 = CARTESIAN_POINT ( 'NONE',  ( -34.50000000000000000, -113.9929510916434339, 12.56351784598954424 ) ) ;
#366 = DIRECTION ( 'NONE',  ( -1.000000000000000000, 0.000000000000000000, 0.000000000000000000 ) ) ;
#367 = CARTESIAN_POINT ( 'NONE',  ( 8.000000000000000000, 21.80633394113452539, 2.912696353505896951 ) ) ;
#368 = CARTESIAN_POINT ( 'NONE',  ( -34.50000000000000000, -113.9929510916434339, 11.21034663311132107 ) ) ;
#369 = DIRECTION ( 'NONE',  ( 1.000000000000000000, 0.000000000000000000, 0.000000000000000000 ) ) ;
#370 = AXIS2_PLACEMENT_3D ( 'NONE', #13032, #24546, #7606 ) ;
#371 = CARTESIAN_POINT ( 'NONE',  ( -35.50000000000000711, -114.8211182053456838, 9.932864235516914775 ) ) ;
#372 = AXIS2_PLACEMENT_3D ( 'NONE', #3017, #13976, #33249 ) ;
#373 = DIRECTION ( 'NONE',  ( 0.000000000000000000, 0.000000000000000000, 1.000000000000000000 ) ) ;
#374 = DIRECTION ( 'NONE',  ( -1.226634733346697831E-16, -0.2588190451025116356, -0.9659258262890706437 ) ) ;
#375 = VERTEX_POINT ( 'NONE', #7637 ) ;
#376 = EDGE_LOOP ( 'NONE', ( #21433, #15135, #23914, #10868 ) ) ;
#377 = CARTESIAN_POINT ( 'NONE',  ( 0.000000000000000000, 44.75336757549799671, -14.30704879393557327 ) ) ;
#378 = CYLINDRICAL_SURFACE ( 'NONE', #30091, 15.49899999999998457 ) ;
#379 = CIRCLE ( 'NONE', #19345, 3.799999999999999822 ) ;
#380 = ORIENTED_EDGE ( 'NONE', *, *, #21612, .F. ) ;
#381 = DIRECTION ( 'NONE',  ( 1.000000000000000000, 0.000000000000000000, 0.000000000000000000 ) ) ;
#382 = ORIENTED_EDGE ( 'NONE', *, *, #11261, .F. ) ;
#383 = EDGE_CURVE ( 'NONE', #18596, #21774, #10521, .T. ) ;
#384 = VECTOR ( 'NONE', #23234, 1000.000000000000000 ) ;
#385 = CARTESIAN_POINT ( 'NONE',  ( -35.50000000000000000, -114.5974311500472567, -0.6247823525984269599 ) ) ;
#386 = CARTESIAN_POINT ( 'NONE',  ( 7.999999999999992895, 46.90537658765329354, 2.727856614654466938 ) ) ;
#387 = CARTESIAN_POINT ( 'NONE',  ( -39.02454729103295961, -114.7691647218148745, 5.159774454178448266 ) ) ;
#388 = CARTESIAN_POINT ( 'NONE',  ( 0.000000000000000000, 51.19683565102445755, 9.104066087303644750 ) ) ;
#389 = AXIS2_PLACEMENT_3D ( 'NONE', #7723, #24133, #18535 ) ;
#390 = VECTOR ( 'NONE', #25326, 1000.000000000000000 ) ;
#391 = ORIENTED_EDGE ( 'NONE', *, *, #34173, .T. ) ;
#392 = CIRCLE ( 'NONE', #1591, 47.49900000000000944 ) ;
#393 = CYLINDRICAL_SURFACE ( 'NONE', #30281, 7.199999999999993072 ) ;
#394 = CARTESIAN_POINT ( 'NONE',  ( -35.50000000000000711, -112.0140900043112282, 0.8439677466545482121 ) ) ;
#395 = ORIENTED_EDGE ( 'NONE', *, *, #3137, .T. ) ;
#396 = ORIENTED_EDGE ( 'NONE', *, *, #22449, .F. ) ;
#397 = VECTOR ( 'NONE', #13640, 1000.000000000000000 ) ;
#398 = AXIS2_PLACEMENT_3D ( 'NONE', #35095, #21378, #5020 ) ;
#399 = CARTESIAN_POINT ( 'NONE',  ( -35.00000000000000000, -114.0592624029313242, 9.003524454178448266 ) ) ;
#400 = EDGE_CURVE ( 'NONE', #22707, #21695, #5318, .T. ) ;
#401 =( NAMED_UNIT ( * ) PLANE_ANGLE_UNIT ( ) SI_UNIT ( $, .RADIAN. ) );
#402 = DIRECTION ( 'NONE',  ( 0.000000000000000000, -0.3090169943749350723, -0.9510565162951575280 ) ) ;
#403 = VERTEX_POINT ( 'NONE', #30151 ) ;
#404 = EDGE_LOOP ( 'NONE', ( #13036, #19341, #25152, #34846 ) ) ;
#405 = CARTESIAN_POINT ( 'NONE',  ( -34.50000000000000000, -112.7472371723319355, 1.839427296857320648 ) ) ;
#406 = CYLINDRICAL_SURFACE ( 'NONE', #13724, 5.000000000000011546 ) ;
#407 = ORIENTED_EDGE ( 'NONE', *, *, #33311, .T. ) ;
#408 = PRODUCT_DEFINITION_CONTEXT ( 'detailed design', #15835, 'design' ) ;
#409 = CARTESIAN_POINT ( 'NONE',  ( 0.000000000000000000, -10.15474465512046542, 9.637487275701101197 ) ) ;
#410 = CIRCLE ( 'NONE', #8457, 0.5000000000000004441 ) ;
#411 = VECTOR ( 'NONE', #24803, 1000.000000000000000 ) ;
#412 = CARTESIAN_POINT ( 'NONE',  ( -35.50000000000000000, -113.9929510916434339, 11.91443571948720148 ) ) ;
#413 = DIRECTION ( 'NONE',  ( 1.000000000000000000, 0.000000000000000000, 0.000000000000000000 ) ) ;
#414 = DIRECTION ( 'NONE',  ( -1.000000000000000000, -1.734723475976807094E-16, 0.000000000000000000 ) ) ;
#415 = CARTESIAN_POINT ( 'NONE',  ( -34.50000000000000000, -115.9821387493194891, -0.8839717462762166633 ) ) ;
#416 = AXIS2_PLACEMENT_3D ( 'NONE', #846, #31809, #12558 ) ;
#417 = ADVANCED_FACE ( 'NONE', ( #22037 ), #5488, .T. ) ;
#418 = AXIS2_PLACEMENT_3D ( 'NONE', #11952, #782, #607 ) ;
#419 = CARTESIAN_POINT ( 'NONE',  ( -39.00000206272865455, -115.9929510916434481, 12.61164896875035879 ) ) ;
#420 = LINE ( 'NONE', #771, #15850 ) ;
#421 = CARTESIAN_POINT ( 'NONE',  ( 8.000000000000000000, 1.693188892523948885, -15.40623615209870323 ) ) ;
#422 = AXIS2_PLACEMENT_3D ( 'NONE', #13815, #3025, #22085 ) ;
#423 = VERTEX_POINT ( 'NONE', #35569 ) ;
#424 = DIRECTION ( 'NONE',  ( 0.000000000000000000, 0.000000000000000000, 1.000000000000000000 ) ) ;
#425 = CYLINDRICAL_SURFACE ( 'NONE', #5340, 47.49900000000001654 ) ;
#426 = AXIS2_PLACEMENT_3D ( 'NONE', #32589, #7921, #10816 ) ;
#427 = DIRECTION ( 'NONE',  ( 0.000000000000000000, 0.000000000000000000, -1.000000000000000000 ) ) ;
#428 = VERTEX_POINT ( 'NONE', #27465 ) ;
#429 = DIRECTION ( 'NONE',  ( 0.000000000000000000, -1.000000000000000000, 0.000000000000000000 ) ) ;
#430 = CYLINDRICAL_SURFACE ( 'NONE', #31948, 8.000000000000001776 ) ;
#431 = EDGE_CURVE ( 'NONE', #31128, #23989, #2442, .T. ) ;
#432 = DIRECTION ( 'NONE',  ( 0.000000000000000000, 0.000000000000000000, 1.000000000000000000 ) ) ;
#433 = CARTESIAN_POINT ( 'NONE',  ( 7.999999999999992895, 45.78515115856061612, -12.64416602183615623 ) ) ;
#434 = ADVANCED_FACE ( 'NONE', ( #13768 ), #33029, .T. ) ;
#435 = EDGE_CURVE ( 'NONE', #31128, #24732, #16826, .T. ) ;
#436 = ITEM_DEFINED_TRANSFORMATION ( 'NONE', 'NONE', #28729,  #21307 ) ;
#437 = DIRECTION ( 'NONE',  ( 0.000000000000000000, 0.1253332335643046747, -0.9921147013144777649 ) ) ;
#438 = CARTESIAN_POINT ( 'NONE',  ( 50.00000000000000000, -25.98076211353320275, 95.99999999999991473 ) ) ;
#439 = AXIS2_PLACEMENT_3D ( 'NONE', #27809, #6356, #14099 ) ;
#440 = VERTEX_POINT ( 'NONE', #35039 ) ;
#441 = PLANE ( 'NONE',  #8977 ) ;
#442 = AXIS2_PLACEMENT_3D ( 'NONE', #1395, #17763, #28764 ) ;
#443 = CARTESIAN_POINT ( 'NONE',  ( 55.00000000000000000, 0.000000000000000000, 70.00000000000000000 ) ) ;
#444 = DIRECTION ( 'NONE',  ( -1.000000000000000000, 0.000000000000000000, 0.000000000000000000 ) ) ;
#445 = ORIENTED_EDGE ( 'NONE', *, *, #2012, .T. ) ;
#446 = CARTESIAN_POINT ( 'NONE',  ( -37.05926240293131713, -113.0000000000000000, 3.621475545821551734 ) ) ;
#447 = VECTOR ( 'NONE', #3446, 1000.000000000000000 ) ;
#448 = EDGE_CURVE ( 'NONE', #932, #28254, #34663, .T. ) ;
#449 = ORIENTED_EDGE ( 'NONE', *, *, #1744, .T. ) ;
#450 = EDGE_CURVE ( 'NONE', #2681, #869, #20260, .T. ) ;
#451 = SURFACE_SIDE_STYLE ('',( #22398 ) ) ;
#452 = ORIENTED_EDGE ( 'NONE', *, *, #14571, .F. ) ;
#453 = VERTEX_POINT ( 'NONE', #32313 ) ;
#454 = CIRCLE ( 'NONE', #19981, 20.00000000000000355 ) ;
#455 = LINE ( 'NONE', #30526, #1091 ) ;
#456 =( REPRESENTATION_RELATIONSHIP ('NONE','NONE', #26607, #13971 ) REPRESENTATION_RELATIONSHIP_WITH_TRANSFORMATION ( #30918 )SHAPE_REPRESENTATION_RELATIONSHIP( ) );
#457 = AXIS2_PLACEMENT_3D ( 'NONE', #23375, #28612, #18143 ) ;
#458 = CARTESIAN_POINT ( 'NONE',  ( -35.50000000000000711, -115.6286452741999113, -1.424448457485488095 ) ) ;
#459 = CARTESIAN_POINT ( 'NONE',  ( 8.000000000000000000, 10.62435788049443808, 13.16139124467922272 ) ) ;
#460 = CARTESIAN_POINT ( 'NONE',  ( -35.50000000000000711, -114.1264797827112574, 9.515205387299289441 ) ) ;
#461 = FACE_BOUND ( 'NONE', #6076, .T. ) ;
#462 = CARTESIAN_POINT ( 'NONE',  ( 0.000000000000000000, -2.710505431213761085E-17, -21.89999999999999858 ) ) ;
#463 = EDGE_CURVE ( 'NONE', #27419, #6784, #13245, .T. ) ;
#464 = CARTESIAN_POINT ( 'NONE',  ( -34.50000000000000000, -114.9819937217110635, 10.35556074009299188 ) ) ;
#465 = DIRECTION ( 'NONE',  ( 1.000000000000000000, -0.000000000000000000, 0.000000000000000000 ) ) ;
#466 = PRODUCT_RELATED_PRODUCT_CATEGORY ( 'part', '', ( #12395 ) ) ;
#467 = DIRECTION ( 'NONE',  ( 0.000000000000000000, -8.673617379884035472E-16, -1.000000000000000000 ) ) ;
#468 = CARTESIAN_POINT ( 'NONE',  ( -36.24999999999983658, -115.9929510916434481, 14.11852480586265024 ) ) ;
#469 = CARTESIAN_POINT ( 'NONE',  ( -35.50000000000000711, -112.0140900043366088, -0.5935324770972457697 ) ) ;
#470 = CARTESIAN_POINT ( 'NONE',  ( -55.00000000000000000, -25.98076211353320275, 78.99999999999992895 ) ) ;
#471 = CIRCLE ( 'NONE', #25782, 20.00000000000000711 ) ;
#472 = DIRECTION ( 'NONE',  ( 0.000000000000000000, 0.000000000000000000, -1.000000000000000000 ) ) ;
#473 = FACE_BOUND ( 'NONE', #33922, .T. ) ;
#474 = ADVANCED_FACE ( 'NONE', ( #13068 ), #24053, .T. ) ;
#475 = CARTESIAN_POINT ( 'NONE',  ( 8.000000000000007105, -5.363026430117185051, 9.919332006307207905 ) ) ;
#476 = DIRECTION ( 'NONE',  ( 0.000000000000000000, -1.000000000000000000, -2.543449303551180694E-16 ) ) ;
#477 = ORIENTED_EDGE ( 'NONE', *, *, #31892, .F. ) ;
#478 = EDGE_CURVE ( 'NONE', #24108, #10834, #18807, .T. ) ;
#479 = ADVANCED_FACE ( 'NONE', ( #18984 ), #14625, .T. ) ;
#480 = CARTESIAN_POINT ( 'NONE',  ( -36.11231047232249125, -115.9754527089670262, 7.277725545821551734 ) ) ;
#481 = CIRCLE ( 'NONE', #21749, 8.000000000000007105 ) ;
#482 = CARTESIAN_POINT ( 'NONE',  ( 0.000000000000000000, 51.85248208264525260, -3.914090171285633524 ) ) ;
#483 = DIRECTION ( 'NONE',  ( -1.000000000000000000, 0.000000000000000000, 0.000000000000000000 ) ) ;
#484 = CARTESIAN_POINT ( 'NONE',  ( -34.49999999999998579, -34.23950567274747669, 96.30456345124106576 ) ) ;
#485 = VERTEX_POINT ( 'NONE', #11755 ) ;
#486 = EDGE_LOOP ( 'NONE', ( #7178, #9341, #8028, #31274 ) ) ;
#487 = ADVANCED_BREP_SHAPE_REPRESENTATION ( '', ( #34958, #21307 ), #24211 ) ;
#488 = DIRECTION ( 'NONE',  ( 0.000000000000000000, 0.5877852522924742473, -0.8090169943749466741 ) ) ;
#489 = CARTESIAN_POINT ( 'NONE',  ( 4.000000000000000000, 4.627536653468036720E-16, 45.99999999999998579 ) ) ;
#490 = ORIENTED_EDGE ( 'NONE', *, *, #31210, .T. ) ;
#491 = ORIENTED_EDGE ( 'NONE', *, *, #20535, .F. ) ;
#492 = ADVANCED_FACE ( 'NONE', ( #19665 ), #33908, .F. ) ;
#493 = DIRECTION ( 'NONE',  ( 1.000000000000000000, 0.000000000000000000, 0.000000000000000000 ) ) ;
#494 = CARTESIAN_POINT ( 'NONE',  ( 0.000000000000000000, -34.03046037009232094, -33.13733193845841640 ) ) ;
#495 = CIRCLE ( 'NONE', #14285, 8.000000000000007105 ) ;
#496 = EDGE_CURVE ( 'NONE', #185, #4943, #8530, .T. ) ;
#497 = AXIS2_PLACEMENT_3D ( 'NONE', #3704, #28360, #7419 ) ;
#498 = SHAPE_DEFINITION_REPRESENTATION ( #31065, #33742 ) ;
#499 = CYLINDRICAL_SURFACE ( 'NONE', #3569, 3.799999999999999822 ) ;
#500 = ORIENTED_EDGE ( 'NONE', *, *, #33503, .T. ) ;
#501 = ORIENTED_EDGE ( 'NONE', *, *, #19569, .T. ) ;
#502 = CARTESIAN_POINT ( 'NONE',  ( 0.6000000000000035305, -12.74999999999999822, -1.386669559958809814E-29 ) ) ;
#503 = CARTESIAN_POINT ( 'NONE',  ( 0.000000000000000000, 17.08890430202750110, 43.76671000081951490 ) ) ;
#504 = ORIENTED_EDGE ( 'NONE', *, *, #8965, .F. ) ;
#505 = DIRECTION ( 'NONE',  ( -1.000000000000000000, -0.000000000000000000, -0.000000000000000000 ) ) ;
#506 = ADVANCED_FACE ( 'NONE', ( #28329 ), #31024, .T. ) ;
#507 = CARTESIAN_POINT ( 'NONE',  ( -34.50000000000000000, -113.3474311500483935, -0.6247823525984269599 ) ) ;
#508 = DIRECTION ( 'NONE',  ( -1.000000000000000000, 0.000000000000000000, -0.000000000000000000 ) ) ;
#509 = CARTESIAN_POINT ( 'NONE',  ( 0.000000000000000000, 0.000000000000000000, 4.000000000000000000 ) ) ;
#510 = CARTESIAN_POINT ( 'NONE',  ( -39.00000000000000711, -114.9929510916434339, 11.91443571948719615 ) ) ;
#511 = ADVANCED_FACE ( 'NONE', ( #8700 ), #3145, .T. ) ;
#512 = CARTESIAN_POINT ( 'NONE',  ( 7.999999999999992895, 0.000000000000000000, 0.000000000000000000 ) ) ;
#513 = DIRECTION ( 'NONE',  ( -1.000000000000000000, -0.000000000000000000, -0.000000000000000000 ) ) ;
#514 = CARTESIAN_POINT ( 'NONE',  ( -34.50000000000000000, -114.9929510916434339, 12.59652202191340642 ) ) ;
#515 = DIRECTION ( 'NONE',  ( 0.000000000000000000, 0.000000000000000000, 1.000000000000000000 ) ) ;
#516 = FACE_BOUND ( 'NONE', #19608, .T. ) ;
#517 = DIRECTION ( 'NONE',  ( -1.000000000000000000, 0.000000000000000000, 0.000000000000000000 ) ) ;
#518 = CARTESIAN_POINT ( 'NONE',  ( -37.49999999999999289, -11.52052244843579309, 112.1848168619253840 ) ) ;
#519 = VERTEX_POINT ( 'NONE', #9064 ) ;
#520 = DIRECTION ( 'NONE',  ( -5.339440136655842133E-16, -1.000000000000000000, 6.938893903907197563E-17 ) ) ;
#521 = ORIENTED_EDGE ( 'NONE', *, *, #7435, .T. ) ;
#522 = EDGE_CURVE ( 'NONE', #24075, #10339, #11416, .T. ) ;
#523 = CARTESIAN_POINT ( 'NONE',  ( -39.16322519054179452, -116.0794154965774823, 3.566024454178448710 ) ) ;
#524 = EDGE_CURVE ( 'NONE', #10046, #1935, #25095, .T. ) ;
#525 = FACE_BOUND ( 'NONE', #22321, .T. ) ;
#526 = CARTESIAN_POINT ( 'NONE',  ( -35.50000000000000711, -112.1403507321855528, -1.128496220798856253 ) ) ;
#527 = ORIENTED_EDGE ( 'NONE', *, *, #11411, .F. ) ;
#528 = VECTOR ( 'NONE', #14611, 1000.000000000000000 ) ;
#529 = VERTEX_POINT ( 'NONE', #3676 ) ;
#530 = CARTESIAN_POINT ( 'NONE',  ( 8.000000000000007105, 11.27190672109280811, -0.3151488735047974776 ) ) ;
#531 = DIRECTION ( 'NONE',  ( -1.000000000000000000, 0.000000000000000000, 0.000000000000000000 ) ) ;
#532 = VERTEX_POINT ( 'NONE', #20194 ) ;
#533 = DIRECTION ( 'NONE',  ( -1.000000000000000000, 0.000000000000000000, 0.000000000000000000 ) ) ;
#534 = CYLINDRICAL_SURFACE ( 'NONE', #32662, 44.99999999999999289 ) ;
#535 = ORIENTED_EDGE ( 'NONE', *, *, #3545, .F. ) ;
#536 = ORIENTED_EDGE ( 'NONE', *, *, #30688, .F. ) ;
#537 = CARTESIAN_POINT ( 'NONE',  ( 0.000000000000000000, 0.000000000000000000, 0.000000000000000000 ) ) ;
#538 = CARTESIAN_POINT ( 'NONE',  ( 3.999999999999996447, -2.912696353505970226, 21.80633394113446499 ) ) ;
#539 = ORIENTED_EDGE ( 'NONE', *, *, #35544, .F. ) ;
#540 = VERTEX_POINT ( 'NONE', #11585 ) ;
#541 = CARTESIAN_POINT ( 'NONE',  ( -35.50000000000000000, -112.9611193698460738, 2.883091707513499635 ) ) ;
#542 = VERTEX_POINT ( 'NONE', #3500 ) ;
#543 = CARTESIAN_POINT ( 'NONE',  ( -35.50025087934803736, -114.9929510916434339, 12.63488142334835196 ) ) ;
#544 = EDGE_CURVE ( 'NONE', #34202, #2406, #30682, .T. ) ;
#545 = CIRCLE ( 'NONE', #10351, 4.000000000000000000 ) ;
#546 = EDGE_CURVE ( 'NONE', #32690, #18111, #21436, .T. ) ;
#547 = CARTESIAN_POINT ( 'NONE',  ( -38.98797722933581866, -113.9929510916434339, 12.81430620224974959 ) ) ;
#548 = DIRECTION ( 'NONE',  ( 0.000000000000000000, 0.000000000000000000, -1.000000000000000000 ) ) ;
#549 = DIRECTION ( 'NONE',  ( -1.000000000000000000, 0.000000000000000000, 0.000000000000000000 ) ) ;
#550 = COLOUR_RGB ( '', 0.72549020, 0.75294118, 0.79215686) ;
#551 = CARTESIAN_POINT ( 'NONE',  ( -34.50300906734826611, -113.9929510916434339, 12.71660600561482468 ) ) ;
#552 = CARTESIAN_POINT ( 'NONE',  ( -38.98797722933582577, -114.9929510916434339, 12.81430620224974959 ) ) ;
#553 = CARTESIAN_POINT ( 'NONE',  ( -35.50000000000000711, -114.9929510916434339, 10.51175824272318415 ) ) ;
#554 = DIRECTION ( 'NONE',  ( 0.000000000000000000, -0.8090169943749405679, -0.5877852522924827960 ) ) ;
#555 = CARTESIAN_POINT ( 'NONE',  ( -39.49999999999999289, -3.784235812937200460, 96.08311962715481513 ) ) ;
#556 = ORIENTED_EDGE ( 'NONE', *, *, #35529, .F. ) ;
#557 = ORIENTED_EDGE ( 'NONE', *, *, #20368, .F. ) ;
#558 = LINE ( 'NONE', #915, #5728 ) ;
#559 = CARTESIAN_POINT ( 'NONE',  ( 0.000000000000000000, 0.000000000000000000, 36.00000000000000000 ) ) ;
#560 = ORIENTED_EDGE ( 'NONE', *, *, #26222, .T. ) ;
#561 = DIRECTION ( 'NONE',  ( -5.339440136655842133E-16, -1.000000000000000000, 6.938893903907197563E-17 ) ) ;
#562 = EDGE_LOOP ( 'NONE', ( #8046, #15728, #33138, #17649 ) ) ;
#563 = CARTESIAN_POINT ( 'NONE',  ( -35.50000000000000000, -113.0140978167138712, -0.6247823525979733228 ) ) ;
#564 = FACE_OUTER_BOUND ( 'NONE', #12819, .T. ) ;
#565 = CARTESIAN_POINT ( 'NONE',  ( -35.62769128460905677, -115.4561184093552413, 4.691024454178448266 ) ) ;
#566 = AXIS2_PLACEMENT_3D ( 'NONE', #22239, #8555, #22407 ) ;
#567 = ORIENTED_EDGE ( 'NONE', *, *, #16616, .F. ) ;
#568 = DIRECTION ( 'NONE',  ( 0.000000000000000000, -1.000000000000000000, 0.000000000000000000 ) ) ;
#569 = ORIENTED_EDGE ( 'NONE', *, *, #1551, .F. ) ;
#570 = VECTOR ( 'NONE', #19867, 1000.000000000000000 ) ;
#571 = FILL_AREA_STYLE_COLOUR ( '', #26846 ) ;
#572 = CARTESIAN_POINT ( 'NONE',  ( -35.50000000000000711, -112.6605569508015350, 1.812590711673265575 ) ) ;
#573 = ORIENTED_EDGE ( 'NONE', *, *, #27913, .F. ) ;
#574 = VERTEX_POINT ( 'NONE', #20021 ) ;
#575 = CARTESIAN_POINT ( 'NONE',  ( -38.37230871539094323, -112.5438815906447729, 5.441024454178449155 ) ) ;
#576 = VECTOR ( 'NONE', #819, 1000.000000000000000 ) ;
#577 = VERTEX_POINT ( 'NONE', #17928 ) ;
#578 = AXIS2_PLACEMENT_3D ( 'NONE', #13486, #24469, #16158 ) ;
#579 = CARTESIAN_POINT ( 'NONE',  ( 7.999999999999992895, -24.47917365149979219, 45.87777302070927732 ) ) ;
#580 = VERTEX_POINT ( 'NONE', #778 ) ;
#581 = ORIENTED_EDGE ( 'NONE', *, *, #5080, .F. ) ;
#582 = CARTESIAN_POINT ( 'NONE',  ( -34.50000000000000000, -113.0106174888879877, 1.881901162060937827 ) ) ;
#583 = DIRECTION ( 'NONE',  ( -1.000000000000000000, 0.000000000000000000, 0.000000000000000000 ) ) ;
#584 = VERTEX_POINT ( 'NONE', #3327 ) ;
#585 = ORIENTED_EDGE ( 'NONE', *, *, #4307, .T. ) ;
#586 = CARTESIAN_POINT ( 'NONE',  ( 8.000000000000000000, 3.678165988948789877, -15.05623113391063406 ) ) ;
#587 = EDGE_CURVE ( 'NONE', #5670, #2768, #8782, .T. ) ;
#588 = CARTESIAN_POINT ( 'NONE',  ( -35.50000000000000000, -113.9929510916434339, 10.50625754673577994 ) ) ;
#589 = CARTESIAN_POINT ( 'NONE',  ( -3.799999999999999822, 0.000000000000000000, -34.40000000000000568 ) ) ;
#590 = VECTOR ( 'NONE', #2265, 1000.000000000000000 ) ;
#591 = LINE ( 'NONE', #31017, #5597 ) ;
#592 = CARTESIAN_POINT ( 'NONE',  ( -34.50000000000000000, -112.7319952733504635, 2.855726801009121463 ) ) ;
#593 = CARTESIAN_POINT ( 'NONE',  ( -37.74437085908086686, -115.9929510916434481, 14.09929883582536903 ) ) ;
#594 = CYLINDRICAL_SURFACE ( 'NONE', #29679, 8.000000000000001776 ) ;
#595 = VECTOR ( 'NONE', #30757, 1000.000000000000000 ) ;
#596 = DIRECTION ( 'NONE',  ( -1.000000000000000000, 0.000000000000000000, 0.000000000000000000 ) ) ;
#597 = EDGE_CURVE ( 'NONE', #5418, #24725, #6477, .T. ) ;
#598 = AXIS2_PLACEMENT_3D ( 'NONE', #31782, #23685, #21325 ) ;
#599 = AXIS2_PLACEMENT_3D ( 'NONE', #5420, #533, #19441 ) ;
#600 = DIRECTION ( 'NONE',  ( -1.000000000000000000, 0.000000000000000000, 0.000000000000000000 ) ) ;
#601 = DIRECTION ( 'NONE',  ( 1.000000000000000000, -0.000000000000000000, -0.000000000000000000 ) ) ;
#602 = AXIS2_PLACEMENT_3D ( 'NONE', #22892, #9216, #15491 ) ;
#603 = DIRECTION ( 'NONE',  ( -1.000000000000000000, 0.000000000000000000, 0.000000000000000000 ) ) ;
#604 = ORIENTED_EDGE ( 'NONE', *, *, #33983, .T. ) ;
#605 = LINE ( 'NONE', #3678, #32361 ) ;
#606 = CARTESIAN_POINT ( 'NONE',  ( 6.071532165918824830E-15, 1.000000000000000000, 38.00000000000000000 ) ) ;
#607 = DIRECTION ( 'NONE',  ( 1.000000000000000000, -4.528031003192420052E-15, -1.179290629824070178E-15 ) ) ;
#608 = DIRECTION ( 'NONE',  ( 0.000000000000000000, 0.9980267284282712259, 0.06279051952931682945 ) ) ;
#609 = CARTESIAN_POINT ( 'NONE',  ( 8.000000000000000000, -11.06713717293248855, 13.55483219355725844 ) ) ;
#610 = CARTESIAN_POINT ( 'NONE',  ( -9.999999999999994671, 0.000000000000000000, 0.000000000000000000 ) ) ;
#611 = EDGE_LOOP ( 'NONE', ( #12181, #2390, #23196, #30546, #28877, #14877 ) ) ;
#612 = SURFACE_SIDE_STYLE ('',( #91 ) ) ;
#613 = FACE_OUTER_BOUND ( 'NONE', #17801, .T. ) ;
#614 = CARTESIAN_POINT ( 'NONE',  ( 8.000000000000000000, -18.48663108841356717, -3.384281271888017084 ) ) ;
#615 = ORIENTED_EDGE ( 'NONE', *, *, #4691, .F. ) ;
#616 = CIRCLE ( 'NONE', #28227, 11.00000000000001066 ) ;
#617 = CARTESIAN_POINT ( 'NONE',  ( -36.52652403469559061, -114.9754527089670262, 5.777725545821551734 ) ) ;
#618 = ORIENTED_EDGE ( 'NONE', *, *, #23308, .T. ) ;
#619 = EDGE_LOOP ( 'NONE', ( #5194, #17904, #27219, #22825 ) ) ;
#620 = VERTEX_POINT ( 'NONE', #19503 ) ;
#621 = CARTESIAN_POINT ( 'NONE',  ( 7.999999999999992895, 0.000000000000000000, 0.000000000000000000 ) ) ;
#622 = VECTOR ( 'NONE', #10858, 1000.000000000000000 ) ;
#623 =( GEOMETRIC_REPRESENTATION_CONTEXT ( 3 ) GLOBAL_UNCERTAINTY_ASSIGNED_CONTEXT ( ( #6706 ) ) GLOBAL_UNIT_ASSIGNED_CONTEXT ( ( #29466, #21700, #8019 ) ) REPRESENTATION_CONTEXT ( 'NONE', 'WORKASPACE' ) );
#624 = AXIS2_PLACEMENT_3D ( 'NONE', #12818, #34782, #9575 ) ;
#625 = DIRECTION ( 'NONE',  ( 0.000000000000000000, 1.000000000000000000, 0.000000000000000000 ) ) ;
#626 = FACE_OUTER_BOUND ( 'NONE', #28757, .T. ) ;
#627 = AXIS2_PLACEMENT_3D ( 'NONE', #21553, #32552, #26639 ) ;
#628 = EDGE_CURVE ( 'NONE', #13726, #1603, #27780, .T. ) ;
#629 = CARTESIAN_POINT ( 'NONE',  ( -35.50000000000000711, -114.9928438774171582, 10.49113435197128652 ) ) ;
#630 = DIRECTION ( 'NONE',  ( -1.000000000000000000, -0.000000000000000000, 0.000000000000000000 ) ) ;
#631 = EDGE_CURVE ( 'NONE', #27296, #14694, #28154, .T. ) ;
#632 = CARTESIAN_POINT ( 'NONE',  ( 10.50000000000000178, -7.127471650355167704E-32, -1.232595164407830946E-29 ) ) ;
#633 = CARTESIAN_POINT ( 'NONE',  ( -34.50000000000000000, -114.9929510916434339, 10.85830208992344303 ) ) ;
#634 = DIRECTION ( 'NONE',  ( -1.000000000000000000, 0.000000000000000000, 0.000000000000000000 ) ) ;
#635 = AXIS2_PLACEMENT_3D ( 'NONE', #18306, #29485, #1579 ) ;
#636 = CARTESIAN_POINT ( 'NONE',  ( 70.00000000000001421, -37.13120097615721704, 79.35042362907756797 ) ) ;
#637 = EDGE_CURVE ( 'NONE', #14516, #4854, #18566, .T. ) ;
#638 = CARTESIAN_POINT ( 'NONE',  ( -39.00000000000000000, -115.9929510916434481, 11.73841344789285657 ) ) ;
#639 = CARTESIAN_POINT ( 'NONE',  ( -35.50000000000000711, -112.2144317118258527, -1.239329810084414341 ) ) ;
#640 = CARTESIAN_POINT ( 'NONE',  ( 4.000000000000003553, -3.268936481846063113, -13.61301047812921183 ) ) ;
#641 = CARTESIAN_POINT ( 'NONE',  ( 50.00005079999999680, 5.400000000000000355, -0.9999999999999985567 ) ) ;
#642 = CARTESIAN_POINT ( 'NONE',  ( -21.15833593587365513, -14.60640646055094649, 76.70096189432339884 ) ) ;
#643 = CARTESIAN_POINT ( 'NONE',  ( 8.000000000000000000, 14.71414642875970635, -9.471478019454975694 ) ) ;
#644 = DIRECTION ( 'NONE',  ( -1.000000000000000000, 0.000000000000000000, 0.000000000000000000 ) ) ;
#645 = ORIENTED_EDGE ( 'NONE', *, *, #12370, .F. ) ;
#646 = AXIS2_PLACEMENT_3D ( 'NONE', #20529, #14704, #3938 ) ;
#647 = CARTESIAN_POINT ( 'NONE',  ( -36.64504884055821776, -112.9754527089670688, 3.715225545821552178 ) ) ;
#648 = CARTESIAN_POINT ( 'NONE',  ( 7.999999999999992895, 47.00885577955413908, 6.806061952192451692 ) ) ;
#649 = CARTESIAN_POINT ( 'NONE',  ( 7.999999999999992895, 19.44205635905603202, -43.33776004284589334 ) ) ;
#650 = DIRECTION ( 'NONE',  ( -1.000000000000000000, 0.000000000000000000, 0.000000000000000000 ) ) ;
#651 = EDGE_LOOP ( 'NONE', ( #4323, #22804, #11964, #18462 ) ) ;
#652 = ORIENTED_EDGE ( 'NONE', *, *, #8841, .T. ) ;
#653 = CARTESIAN_POINT ( 'NONE',  ( 38.00000000000000000, -10.99999999999999112, 0.000000000000000000 ) ) ;
#654 = CARTESIAN_POINT ( 'NONE',  ( 0.000000000000000000, 35.20873326984128227, -31.88259874183993503 ) ) ;
#655 = ORIENTED_EDGE ( 'NONE', *, *, #31762, .F. ) ;
#656 = VERTEX_POINT ( 'NONE', #964 ) ;
#657 = EDGE_CURVE ( 'NONE', #5410, #7912, #11948, .T. ) ;
#658 = CARTESIAN_POINT ( 'NONE',  ( 4.000000000000003553, 44.25018368420744252, 27.31155879685197263 ) ) ;
#659 = CARTESIAN_POINT ( 'NONE',  ( -34.49999999999998579, -25.98076211353320986, 84.99999999999994316 ) ) ;
#660 = APPLICATION_PROTOCOL_DEFINITION ( 'draft international standard', 'automotive_design', 1998, #17203 ) ;
#661 = LINE ( 'NONE', #3396, #25418 ) ;
#662 = EDGE_LOOP ( 'NONE', ( #8266, #3117 ) ) ;
#663 = ORIENTED_EDGE ( 'NONE', *, *, #14067, .F. ) ;
#664 = EDGE_CURVE ( 'NONE', #29327, #20524, #13938, .T. ) ;
#665 = PLANE ( 'NONE',  #1337 ) ;
#666 = EDGE_CURVE ( 'NONE', #20493, #13129, #4578, .T. ) ;
#667 = EDGE_CURVE ( 'NONE', #19003, #35092, #26350, .T. ) ;
#668 = CARTESIAN_POINT ( 'NONE',  ( 7.999999999999992895, -47.22458491092824318, 5.098390039074071289 ) ) ;
#669 = ORIENTED_EDGE ( 'NONE', *, *, #23660, .F. ) ;
#670 = CIRCLE ( 'NONE', #8717, 15.49899999999998457 ) ;
#671 = DIRECTION ( 'NONE',  ( -1.000000000000000000, 0.000000000000000000, 0.000000000000000000 ) ) ;
#672 = CARTESIAN_POINT ( 'NONE',  ( -34.50000000000000000, -115.0140978167138712, -0.6247823525985405357 ) ) ;
#673 = FACE_OUTER_BOUND ( 'NONE', #23003, .T. ) ;
#674 = CARTESIAN_POINT ( 'NONE',  ( 8.000000000000000000, 0.3212489022567689423, -16.91141623315866482 ) ) ;
#675 = CARTESIAN_POINT ( 'NONE',  ( -39.00000000000000711, -114.9929510916434339, 12.39849696637031151 ) ) ;
#676 = CARTESIAN_POINT ( 'NONE',  ( -50.00000000000000000, 0.000000000000000000, 70.00000000000000000 ) ) ;
#677 = PLANE ( 'NONE',  #20286 ) ;
#678 = EDGE_CURVE ( 'NONE', #10711, #10849, #15672, .T. ) ;
#679 = CARTESIAN_POINT ( 'NONE',  ( -34.50000000000000000, -114.2600084737790809, 8.524153227862690585 ) ) ;
#680 = DIRECTION ( 'NONE',  ( 1.000000000000000000, 1.836970198721029934E-16, 0.000000000000000000 ) ) ;
#681 = ADVANCED_FACE ( 'NONE', ( #6712 ), #12122, .T. ) ;
#682 = DIRECTION ( 'NONE',  ( 0.000000000000000000, 0.9048270524660205760, -0.4257792915650702170 ) ) ;
#683 = AXIS2_PLACEMENT_3D ( 'NONE', #6567, #26384, #18080 ) ;
#684 = FACE_OUTER_BOUND ( 'NONE', #26041, .T. ) ;
#685 = DIRECTION ( 'NONE',  ( -1.000000000000000000, 0.000000000000000000, -0.000000000000000000 ) ) ;
#686 = ORIENTED_EDGE ( 'NONE', *, *, #188, .F. ) ;
#687 = CARTESIAN_POINT ( 'NONE',  ( 7.999999999999992895, 44.75336757549799671, -14.30704879393557327 ) ) ;
#688 = VERTEX_POINT ( 'NONE', #7244 ) ;
#689 = CARTESIAN_POINT ( 'NONE',  ( -38.30190309005061522, -116.9754527089670546, 7.972274454178450043 ) ) ;
#690 = DIRECTION ( 'NONE',  ( -1.000000000000000000, 0.000000000000000000, 0.000000000000000000 ) ) ;
#691 = CARTESIAN_POINT ( 'NONE',  ( -35.50000000000000711, -112.9486715495423681, -1.623175561345890472 ) ) ;
#692 = ORIENTED_EDGE ( 'NONE', *, *, #31285, .T. ) ;
#693 = ORIENTED_EDGE ( 'NONE', *, *, #12556, .F. ) ;
#694 = CARTESIAN_POINT ( 'NONE',  ( 7.999999999999992895, 0.000000000000000000, 0.000000000000000000 ) ) ;
#695 = DIRECTION ( 'NONE',  ( -1.000000000000000000, 0.000000000000000000, 0.000000000000000000 ) ) ;
#696 = ORIENTED_EDGE ( 'NONE', *, *, #4802, .T. ) ;
#697 = VECTOR ( 'NONE', #11975, 1000.000000000000114 ) ;
#698 = EDGE_CURVE ( 'NONE', #15493, #29381, #34092, .T. ) ;
#699 =( REPRESENTATION_RELATIONSHIP ('NONE','NONE', #26607, #18063 ) REPRESENTATION_RELATIONSHIP_WITH_TRANSFORMATION ( #31387 )SHAPE_REPRESENTATION_RELATIONSHIP( ) );
#700 = DIRECTION ( 'NONE',  ( 1.541976423090495387E-16, -1.000000000000000000, 0.000000000000000000 ) ) ;
#701 = ORIENTED_EDGE ( 'NONE', *, *, #8316, .T. ) ;
#703 = ORIENTED_EDGE ( 'NONE', *, *, #21313, .T. ) ;
#702 = EDGE_CURVE ( 'NONE', #28348, #19239, #12841, .T. ) ;
#704 = CARTESIAN_POINT ( 'NONE',  ( -36.23083527818513261, -111.9754527089670404, 5.215225545821551734 ) ) ;
#705 = ADVANCED_FACE ( 'NONE', ( #23823 ), #18225, .T. ) ;
#706 = DIRECTION ( 'NONE',  ( 1.000000000000000000, 0.000000000000000000, 0.000000000000000000 ) ) ;
#707 = EDGE_LOOP ( 'NONE', ( #35537, #16646, #35410, #34981 ) ) ;
#708 = VERTEX_POINT ( 'NONE', #10129 ) ;
#709 = VECTOR ( 'NONE', #30336, 1000.000000000000000 ) ;
#710 = CARTESIAN_POINT ( 'NONE',  ( -35.50000000000000000, -112.4803765279500993, 2.803636946313094569 ) ) ;
#711 = ADVANCED_FACE ( 'NONE', ( #28693 ), #34457, .F. ) ;
#712 = FACE_OUTER_BOUND ( 'NONE', #1339, .T. ) ;
#713 = ORIENTED_EDGE ( 'NONE', *, *, #23446, .F. ) ;
#714 = EDGE_CURVE ( 'NONE', #28345, #33371, #20371, .T. ) ;
#715 = CARTESIAN_POINT ( 'NONE',  ( -37.37500000000009237, -114.9929510916434339, 13.11852480586264669 ) ) ;
#716 = VECTOR ( 'NONE', #27976, 1000.000000000000000 ) ;
#717 = CARTESIAN_POINT ( 'NONE',  ( -37.54906985245723661, -113.9929510916434339, 14.11777216781844757 ) ) ;
#718 = CIRCLE ( 'NONE', #22558, 52.00000000000000711 ) ;
#719 = FACE_BOUND ( 'NONE', #18642, .T. ) ;
#720 = CARTESIAN_POINT ( 'NONE',  ( -42.49999999999999289, -12.06135120645816983, 86.49999999999994316 ) ) ;
#721 = CIRCLE ( 'NONE', #4769, 4.800000000000005151 ) ;
#722 = CARTESIAN_POINT ( 'NONE',  ( -36.12500000000014211, -113.9929510916434339, 14.11852480586265024 ) ) ;
#723 = CARTESIAN_POINT ( 'NONE',  ( 8.000000000000000000, 0.000000000000000000, 0.000000000000000000 ) ) ;
#724 = EDGE_CURVE ( 'NONE', #25690, #31502, #33542, .T. ) ;
#725 = CARTESIAN_POINT ( 'NONE',  ( -35.50040135968785648, -114.9929510916434339, 12.63896776382214071 ) ) ;
#726 = CARTESIAN_POINT ( 'NONE',  ( 8.000000000000007105, 9.919332006307222116, 5.363026430117163734 ) ) ;
#727 = DIRECTION ( 'NONE',  ( -1.000000000000000000, 0.000000000000000000, 0.000000000000000000 ) ) ;
#728 = DIRECTION ( 'NONE',  ( -1.000000000000000000, 0.000000000000000000, -0.000000000000000000 ) ) ;
#729 = ORIENTED_EDGE ( 'NONE', *, *, #32592, .F. ) ;
#730 = ORIENTED_EDGE ( 'NONE', *, *, #15666, .T. ) ;
#731 = CARTESIAN_POINT ( 'NONE',  ( 7.999999999999992895, -7.162210897275381072, -51.50439529848838305 ) ) ;
#732 = DIRECTION ( 'NONE',  ( 0.000000000000000000, 0.000000000000000000, 1.000000000000000000 ) ) ;
#733 = ORIENTED_EDGE ( 'NONE', *, *, #666, .T. ) ;
#734 = AXIS2_PLACEMENT_3D ( 'NONE', #10668, #13371, #21624 ) ;
#735 = PLANE ( 'NONE',  #27972 ) ;
#736 = ORIENTED_EDGE ( 'NONE', *, *, #10860, .F. ) ;
#737 = CIRCLE ( 'NONE', #20844, 44.99999999999999289 ) ;
#738 = CARTESIAN_POINT ( 'NONE',  ( -35.50000000000000000, -115.0140978167134165, -0.6247823525984399495 ) ) ;
#739 = LINE ( 'NONE', #3114, #13317 ) ;
#740 = CARTESIAN_POINT ( 'NONE',  ( -38.02454729103296671, -114.3549511594417396, 8.159774454178448266 ) ) ;
#741 = VERTEX_POINT ( 'NONE', #14986 ) ;
#742 = CARTESIAN_POINT ( 'NONE',  ( -36.11231047232249125, -112.0245472910329880, 7.222274454178451819 ) ) ;
#743 = EDGE_CURVE ( 'NONE', #35591, #7199, #12479, .T. ) ;
#744 = ORIENTED_EDGE ( 'NONE', *, *, #6570, .T. ) ;
#745 = EDGE_CURVE ( 'NONE', #21122, #17030, #7068, .T. ) ;
#746 = DIRECTION ( 'NONE',  ( 0.000000000000000000, -0.4999999999999958367, -0.8660254037844410391 ) ) ;
#747 = VECTOR ( 'NONE', #16758, 1000.000000000000000 ) ;
#748 = CARTESIAN_POINT ( 'NONE',  ( -35.50000000000000000, -116.0215255531121983, -2.372276521655488857 ) ) ;
#749 = CIRCLE ( 'NONE', #31207, 52.00000000000000711 ) ;
#750 = EDGE_LOOP ( 'NONE', ( #4388, #25058, #30347, #34872, #28090, #6286 ) ) ;
#751 = VERTEX_POINT ( 'NONE', #15513 ) ;
#752 = CARTESIAN_POINT ( 'NONE',  ( -36.11231047232249125, -112.0245472910329880, 5.722274454178448266 ) ) ;
#753 =( NAMED_UNIT ( * ) SI_UNIT ( $, .STERADIAN. ) SOLID_ANGLE_UNIT ( ) );
#754 = CARTESIAN_POINT ( 'NONE',  ( 0.000000000000000000, 0.000000000000000000, 0.000000000000000000 ) ) ;
#755 = ORIENTED_EDGE ( 'NONE', *, *, #18321, .T. ) ;
#756 = ORIENTED_EDGE ( 'NONE', *, *, #11411, .T. ) ;
#757 = CARTESIAN_POINT ( 'NONE',  ( -34.50000000000000000, -112.0414288467712112, 1.115164475686276191 ) ) ;
#758 = CARTESIAN_POINT ( 'NONE',  ( 0.000000000000000000, 16.59870953437680896, 3.253005020243904255 ) ) ;
#759 = EDGE_CURVE ( 'NONE', #1825, #2615, #29234, .T. ) ;
#760 = ORIENTED_EDGE ( 'NONE', *, *, #7391, .T. ) ;
#761 = PRODUCT_DEFINITION_CONTEXT ( 'detailed design', #16046, 'design' ) ;
#762 = EDGE_LOOP ( 'NONE', ( #23017, #33225, #3692, #5978 ) ) ;
#763 = DIRECTION ( 'NONE',  ( -0.000000000000000000, 0.000000000000000000, -1.000000000000000000 ) ) ;
#764 = CIRCLE ( 'NONE', #26644, 4.725000000000016520 ) ;
#765 = AXIS2_PLACEMENT_3D ( 'NONE', #10520, #29975, #33023 ) ;
#766 = CARTESIAN_POINT ( 'NONE',  ( -37.18750000000004974, -113.9929510916434339, 13.11852480586264846 ) ) ;
#767 = CARTESIAN_POINT ( 'NONE',  ( -21.15833593587365513, -26.68172400785662290, 89.21410161513769310 ) ) ;
#768 = CARTESIAN_POINT ( 'NONE',  ( 0.000000000000000000, 15.17386234660407140, -15.92965478239605304 ) ) ;
#769 = CARTESIAN_POINT ( 'NONE',  ( -34.50000000000000000, -111.0140978167138570, 0.5627176474015715968 ) ) ;
#770 = CARTESIAN_POINT ( 'NONE',  ( -39.00000000000000000, -115.9929510916434481, 12.57451923796417681 ) ) ;
#771 = CARTESIAN_POINT ( 'NONE',  ( -1.000000000000014655, -4.808326913196006913, -0.7999999999999951594 ) ) ;
#773 = AXIS2_PLACEMENT_3D ( 'NONE', #25054, #11547, #30805 ) ;
#772 = CARTESIAN_POINT ( 'NONE',  ( 0.000000000000000000, -14.71414642875963708, 9.471478019455089381 ) ) ;
#774 = CIRCLE ( 'NONE', #13989, 47.49900000000001654 ) ;
#775 = CIRCLE ( 'NONE', #20886, 9.499000000000012989 ) ;
#776 = CARTESIAN_POINT ( 'NONE',  ( 70.00000000000001421, 87.62632027716348659, 34.45236684482946288 ) ) ;
#777 = DIRECTION ( 'NONE',  ( 1.000000000000000000, -4.524158825347490025E-15, -1.177133787269970298E-15 ) ) ;
#778 = CARTESIAN_POINT ( 'NONE',  ( -5.639656061357301020, -10.48075544252181857, 0.000000000000000000 ) ) ;
#779 = VERTEX_POINT ( 'NONE', #6892 ) ;
#780 = CARTESIAN_POINT ( 'NONE',  ( 3.413765605486549060, -14.29811891091956078, -1.200000000000006617 ) ) ;
#781 = CARTESIAN_POINT ( 'NONE',  ( 70.00000000000001421, 45.53424681125909501, 59.69714175238111409 ) ) ;
#782 = DIRECTION ( 'NONE',  ( -1.174092375852890260E-15, 4.222049128630259891E-16, 1.000000000000000000 ) ) ;
#783 = CARTESIAN_POINT ( 'NONE',  ( 7.999999999999992895, 15.49408907645234734, -44.90087086784577508 ) ) ;
#784 = ITEM_DEFINED_TRANSFORMATION ( 'NONE', 'NONE', #22388,  #21307 ) ;
#785 = DIRECTION ( 'NONE',  ( 1.000000000000000000, -0.000000000000000000, 0.000000000000000000 ) ) ;
#786 = DIRECTION ( 'NONE',  ( -1.000000000000000000, -0.000000000000000000, 0.000000000000000000 ) ) ;
#787 = EDGE_LOOP ( 'NONE', ( #1518, #3931, #9120, #16817 ) ) ;
#788 = EDGE_CURVE ( 'NONE', #2874, #30169, #31736, .T. ) ;
#789 = PRESENTATION_STYLE_ASSIGNMENT (( #11768 ) ) ;
#790 = DIRECTION ( 'NONE',  ( 1.734723475976807341E-16, -1.000000000000000000, 0.000000000000000000 ) ) ;
#791 = CARTESIAN_POINT ( 'NONE',  ( 7.999999999999992895, 39.78933988720149273, -24.98727647984960853 ) ) ;
#792 = ORIENTED_EDGE ( 'NONE', *, *, #12344, .F. ) ;
#793 = VERTEX_POINT ( 'NONE', #28863 ) ;
#794 = CARTESIAN_POINT ( 'NONE',  ( -36.52652403469559061, -114.9754527089670262, 7.277725545821552622 ) ) ;
#795 = ORIENTED_EDGE ( 'NONE', *, *, #19790, .F. ) ;
#796 = ORIENTED_EDGE ( 'NONE', *, *, #22416, .F. ) ;
#797 = ORIENTED_EDGE ( 'NONE', *, *, #33317, .T. ) ;
#798 = DIRECTION ( 'NONE',  ( -1.000000000000000000, 0.000000000000000000, 0.000000000000000000 ) ) ;
#799 = AXIS2_PLACEMENT_3D ( 'NONE', #2899, #3428, #30949 ) ;
#800 = AXIS2_PLACEMENT_3D ( 'NONE', #30330, #75, #27458 ) ;
#801 = CARTESIAN_POINT ( 'NONE',  ( -35.50000000000000711, -115.2732872103912030, -1.592823285204062911 ) ) ;
#802 = CARTESIAN_POINT ( 'NONE',  ( 8.000000000000007105, -11.27190672109260028, -0.3151488735048807444 ) ) ;
#803 = CARTESIAN_POINT ( 'NONE',  ( -35.50000000000000711, -114.9929510916434339, 12.59652202191340642 ) ) ;
#804 = FACE_OUTER_BOUND ( 'NONE', #7598, .T. ) ;
#805 = DIRECTION ( 'NONE',  ( 0.000000000000000000, 0.000000000000000000, 1.000000000000000000 ) ) ;
#806 = AXIS2_PLACEMENT_3D ( 'NONE', #19835, #22373, #33370 ) ;
#807 = CARTESIAN_POINT ( 'NONE',  ( -34.50000000000000000, -114.9929510916434339, 10.55026311463432087 ) ) ;
#808 = DIRECTION ( 'NONE',  ( 1.000000000000000000, 1.836970198721029934E-16, 0.000000000000000000 ) ) ;
#809 = FACE_OUTER_BOUND ( 'NONE', #28343, .T. ) ;
#810 = ORIENTED_EDGE ( 'NONE', *, *, #8583, .F. ) ;
#811 = CARTESIAN_POINT ( 'NONE',  ( -39.00000000000000000, -115.9929510916434481, 12.26648026267477221 ) ) ;
#812 = CARTESIAN_POINT ( 'NONE',  ( -35.50000000000000711, -112.0414288467712112, 1.115164475686276191 ) ) ;
#813 = PRESENTATION_STYLE_ASSIGNMENT (( #32934 ) ) ;
#814 = DIRECTION ( 'NONE',  ( 0.000000000000000000, 0.1253332335642974305, 0.9921147013144787641 ) ) ;
#815 = DIRECTION ( 'NONE',  ( 0.000000000000000000, 0.000000000000000000, 1.000000000000000000 ) ) ;
#816 = FACE_OUTER_BOUND ( 'NONE', #2322, .T. ) ;
#817 = CIRCLE ( 'NONE', #23843, 8.000000000000008882 ) ;
#818 = DIRECTION ( 'NONE',  ( -0.8432271980573220471, 4.875366479720417855E-16, 0.5375573387615479870 ) ) ;
#819 = DIRECTION ( 'NONE',  ( -1.000000000000000000, 0.000000000000000000, -0.000000000000000000 ) ) ;
#820 = ORIENTED_EDGE ( 'NONE', *, *, #33243, .T. ) ;
#821 = CARTESIAN_POINT ( 'NONE',  ( -36.64504884055823908, -115.0245472910329880, 1.784774454178449155 ) ) ;
#822 = DIRECTION ( 'NONE',  ( -1.000000000000000000, 0.000000000000000000, 0.000000000000000000 ) ) ;
#823 = CARTESIAN_POINT ( 'NONE',  ( 0.000000000000000000, 0.000000000000000000, 0.000000000000000000 ) ) ;
#824 = AXIS2_PLACEMENT_3D ( 'NONE', #33297, #24491, #5926 ) ;
#825 = ORIENTED_EDGE ( 'NONE', *, *, #30231, .F. ) ;
#826 = EDGE_LOOP ( 'NONE', ( #7938, #26446, #19938, #30947 ) ) ;
#827 = EDGE_CURVE ( 'NONE', #17814, #16992, #7429, .T. ) ;
#828 = LINE ( 'NONE', #11810, #9606 ) ;
#829 = DIRECTION ( 'NONE',  ( 0.000000000000000000, 0.000000000000000000, -1.000000000000000000 ) ) ;
#830 = ORIENTED_EDGE ( 'NONE', *, *, #13493, .F. ) ;
#831 = EDGE_CURVE ( 'NONE', #31433, #8092, #15696, .T. ) ;
#832 = CARTESIAN_POINT ( 'NONE',  ( -37.05926240293131713, -111.0000000000000284, 5.121475545821551734 ) ) ;
#833 = ORIENTED_EDGE ( 'NONE', *, *, #10772, .F. ) ;
#834 = DIRECTION ( 'NONE',  ( 1.734723475976807834E-16, -1.000000000000000000, 0.000000000000000000 ) ) ;
#835 = CARTESIAN_POINT ( 'NONE',  ( 55.00000000000000000, -2.775557561562891351E-14, 106.0000000000000000 ) ) ;
#836 = EDGE_CURVE ( 'NONE', #11310, #17425, #3855, .T. ) ;
#837 = APPLICATION_PROTOCOL_DEFINITION ( 'draft international standard', 'automotive_design', 1998, #8023 ) ;
#838 = CARTESIAN_POINT ( 'NONE',  ( 0.000000000000000000, -39.64889472655756464, 33.64468972902493960 ) ) ;
#839 = ORIENTED_EDGE ( 'NONE', *, *, #27989, .F. ) ;
#840 = EDGE_LOOP ( 'NONE', ( #34397, #4739, #23398, #35409 ) ) ;
#841 = AXIS2_PLACEMENT_3D ( 'NONE', #19896, #5545, #8749 ) ;
#842 = VECTOR ( 'NONE', #18131, 1000.000000000000000 ) ;
#843 = CARTESIAN_POINT ( 'NONE',  ( 0.000000000000000000, 21.80633394113450052, -2.912696353505896063 ) ) ;
#844 = PLANE ( 'NONE',  #8243 ) ;
#845 = ORIENTED_EDGE ( 'NONE', *, *, #12218, .T. ) ;
#846 = CARTESIAN_POINT ( 'NONE',  ( -9.999999999999994671, 0.000000000000000000, 0.000000000000000000 ) ) ;
#847 = VECTOR ( 'NONE', #27852, 1000.000000000000000 ) ;
#848 = CARTESIAN_POINT ( 'NONE',  ( -34.50000000000000000, -115.0140978167139707, -0.6247823525984387283 ) ) ;
#849 = CYLINDRICAL_SURFACE ( 'NONE', #28263, 47.49900000000001654 ) ;
#850 = CARTESIAN_POINT ( 'NONE',  ( -36.49999999999999289, -11.52052244843579309, 115.1848168619253698 ) ) ;
#851 = AXIS2_PLACEMENT_3D ( 'NONE', #33266, #6070, #8060 ) ;
#852 = CARTESIAN_POINT ( 'NONE',  ( -39.00000000000000711, -114.9929510916434339, 11.73841344789285657 ) ) ;
#853 = DIRECTION ( 'NONE',  ( -0.000000000000000000, 0.000000000000000000, -1.000000000000000000 ) ) ;
#854 = CARTESIAN_POINT ( 'NONE',  ( -36.23083527818513261, -116.0245472910329880, 1.784774454178448710 ) ) ;
#855 = CARTESIAN_POINT ( 'NONE',  ( -39.00000000000000711, -114.9929510916434339, 11.91443571948719615 ) ) ;
#856 = LINE ( 'NONE', #14891, #34928 ) ;
#857 = EDGE_CURVE ( 'NONE', #18809, #28617, #1930, .T. ) ;
#858 = DIRECTION ( 'NONE',  ( 0.000000000000000000, 0.000000000000000000, -1.000000000000000000 ) ) ;
#859 = AXIS2_PLACEMENT_3D ( 'NONE', #7769, #4918, #5101 ) ;
#860 = DIRECTION ( 'NONE',  ( 1.000000000000000000, 0.000000000000000000, 0.000000000000000000 ) ) ;
#861 = CARTESIAN_POINT ( 'NONE',  ( -34.49999999999998579, -25.98076211353322051, 84.99999999999992895 ) ) ;
#862 = ORIENTED_EDGE ( 'NONE', *, *, #27591, .F. ) ;
#863 = CYLINDRICAL_SURFACE ( 'NONE', #14722, 47.49900000000001654 ) ;
#864 = VERTEX_POINT ( 'NONE', #10853 ) ;
#865 = CARTESIAN_POINT ( 'NONE',  ( -35.81662171581203324, -110.9754527089670546, 3.715225545821552178 ) ) ;
#866 = CARTESIAN_POINT ( 'NONE',  ( 0.000000000000000000, -8.725776631572701447, 3.753907720749016796 ) ) ;
#867 = CARTESIAN_POINT ( 'NONE',  ( -35.50000000000000711, -112.8511839106603247, -1.611965039240275122 ) ) ;
#868 = ORIENTED_EDGE ( 'NONE', *, *, #16358, .T. ) ;
#869 = VERTEX_POINT ( 'NONE', #13202 ) ;
#870 = AXIS2_PLACEMENT_3D ( 'NONE', #6568, #19233, #11989 ) ;
#871 = ADVANCED_FACE ( 'NONE', ( #21988 ), #35173, .F. ) ;
#873 = LINE ( 'NONE', #25383, #15397 ) ;
#872 = PRODUCT_DEFINITION_SHAPE ( 'NONE', 'NONE',  #912 ) ;
#874 = AXIS2_PLACEMENT_3D ( 'NONE', #19196, #30544, #22421 ) ;
#875 = DIRECTION ( 'NONE',  ( -1.000000000000000000, 0.000000000000000000, 0.000000000000000000 ) ) ;
#876 = VERTEX_POINT ( 'NONE', #27238 ) ;
#877 = EDGE_CURVE ( 'NONE', #33166, #32215, #26711, .T. ) ;
#878 = EDGE_CURVE ( 'NONE', #32697, #33707, #24177, .T. ) ;
#879 = ORIENTED_EDGE ( 'NONE', *, *, #34561, .T. ) ;
#880 = VECTOR ( 'NONE', #6059, 1000.000000000000000 ) ;
#881 = AXIS2_PLACEMENT_3D ( 'NONE', #18246, #26551, #34156 ) ;
#882 = CARTESIAN_POINT ( 'NONE',  ( -34.49999999999998579, -31.64142946139415713, 97.80456345124107997 ) ) ;
#883 = EDGE_LOOP ( 'NONE', ( #34471, #34935, #28562, #25963 ) ) ;
#884 = ORIENTED_EDGE ( 'NONE', *, *, #5572, .F. ) ;
#885 = CARTESIAN_POINT ( 'NONE',  ( -39.02454729103295961, -113.2308352781851397, 6.340225545821550845 ) ) ;
#886 = EDGE_CURVE ( 'NONE', #6583, #5115, #8131, .T. ) ;
#887 = DIRECTION ( 'NONE',  ( 1.000000000000000000, 0.000000000000000000, 0.000000000000000000 ) ) ;
#888 = ADVANCED_FACE ( 'NONE', ( #7597 ), #29763, .T. ) ;
#889 = DIRECTION ( 'NONE',  ( -1.000000000000000000, 0.000000000000000000, 0.000000000000000000 ) ) ;
#891 = VERTEX_POINT ( 'NONE', #10669 ) ;
#890 = AXIS2_PLACEMENT_3D ( 'NONE', #13160, #26663, #24135 ) ;
#892 = VERTEX_POINT ( 'NONE', #10490 ) ;
#893 = CARTESIAN_POINT ( 'NONE',  ( -35.50000000000000000, -113.2224311500466030, -2.624782352598442614 ) ) ;
#894 = FACE_OUTER_BOUND ( 'NONE', #8453, .T. ) ;
#895 = ORIENTED_EDGE ( 'NONE', *, *, #19002, .T. ) ;
#896 = CARTESIAN_POINT ( 'NONE',  ( -35.74814306589956914, -114.9929510916434339, 13.05539834812772781 ) ) ;
#897 = CARTESIAN_POINT ( 'NONE',  ( -39.00000206272865455, -113.9929510916434339, 12.61164896875035879 ) ) ;
#898 = VECTOR ( 'NONE', #11588, 1000.000000000000000 ) ;
#899 = LINE ( 'NONE', #25581, #1043 ) ;
#900 = DIRECTION ( 'NONE',  ( 0.000000000000000000, 0.000000000000000000, 1.000000000000000000 ) ) ;
#901 = CARTESIAN_POINT ( 'NONE',  ( -35.80421860361284558, -113.9929510916434339, 14.10650203519841916 ) ) ;
#902 = LINE ( 'NONE', #34037, #32658 ) ;
#903 = CIRCLE ( 'NONE', #21584, 3.799999999999999822 ) ;
#904 = EDGE_CURVE ( 'NONE', #3203, #33824, #4242, .T. ) ;
#905 = AXIS2_PLACEMENT_3D ( 'NONE', #14826, #14455, #1154 ) ;
#906 = CARTESIAN_POINT ( 'NONE',  ( -35.96730626674924025, -114.9929510916434339, 13.11752178341330044 ) ) ;
#907 = DIRECTION ( 'NONE',  ( -1.000000000000000000, -0.000000000000000000, 0.000000000000000000 ) ) ;
#908 = VERTEX_POINT ( 'NONE', #15691 ) ;
#909 = DIRECTION ( 'NONE',  ( 1.000000000000000000, -5.339440136655842133E-16, -1.047965281155519420E-16 ) ) ;
#910 = DIRECTION ( 'NONE',  ( -1.836970198721029934E-16, 1.000000000000000000, 0.000000000000000000 ) ) ;
#911 = ORIENTED_EDGE ( 'NONE', *, *, #959, .F. ) ;
#912 = PRODUCT_DEFINITION ( 'UNKNOWN', '', #34489, #31011 ) ;
#913 = CARTESIAN_POINT ( 'NONE',  ( -35.74814306589956914, -114.9929510916434339, 13.05539834812772781 ) ) ;
#914 = EDGE_LOOP ( 'NONE', ( #16361, #32759, #8268, #34150 ) ) ;
#915 = CARTESIAN_POINT ( 'NONE',  ( 4.000000000000003553, -12.30077720129132679, 50.52416135122078344 ) ) ;
#916 = LINE ( 'NONE', #17108, #747 ) ;
#917 = AXIS2_PLACEMENT_3D ( 'NONE', #22747, #16640, #22392 ) ;
#918 = AXIS2_PLACEMENT_3D ( 'NONE', #32577, #332, #10621 ) ;
#919 = ORIENTED_EDGE ( 'NONE', *, *, #32387, .F. ) ;
#920 = CYLINDRICAL_SURFACE ( 'NONE', #19895, 22.00000000000000000 ) ;
#921 = ORIENTED_EDGE ( 'NONE', *, *, #33278, .T. ) ;
#922 = CARTESIAN_POINT ( 'NONE',  ( -35.50000000000000000, -113.0140978167156902, -0.6247823525984268489 ) ) ;
#923 = CYLINDRICAL_SURFACE ( 'NONE', #16159, 13.99999999999999822 ) ;
#924 = CARTESIAN_POINT ( 'NONE',  ( -35.97545270896702618, -113.6450488405582604, 8.909774454178450043 ) ) ;
#925 = EDGE_CURVE ( 'NONE', #1732, #8675, #21625, .T. ) ;
#926 = ADVANCED_FACE ( 'NONE', ( #19110 ), #21813, .F. ) ;
#927 = ORIENTED_EDGE ( 'NONE', *, *, #14396, .F. ) ;
#928 = CARTESIAN_POINT ( 'NONE',  ( -38.97545270896704039, -113.1123104723225197, 6.847274454178450931 ) ) ;
#929 = CARTESIAN_POINT ( 'NONE',  ( 0.000000000000000000, 22.43957647427161461, 41.27978878573636479 ) ) ;
#930 = VECTOR ( 'NONE', #2407, 1000.000000000000114 ) ;
#931 = CARTESIAN_POINT ( 'NONE',  ( -35.50000000000000711, -112.0221129971568104, -0.7553032835231431319 ) ) ;
#932 = VERTEX_POINT ( 'NONE', #34998 ) ;
#933 = VERTEX_POINT ( 'NONE', #16399 ) ;
#934 = LINE ( 'NONE', #18017, #26319 ) ;
#935 = CIRCLE ( 'NONE', #21042, 4.000000000000003553 ) ;
#936 = AXIS2_PLACEMENT_3D ( 'NONE', #35608, #27322, #5706 ) ;
#937 = SHAPE_REPRESENTATION_RELATIONSHIP ( 'NONE' , 'NONE' ,  #15534, #14621 ) ;
#938 = EDGE_CURVE ( 'NONE', #16466, #28118, #27417, .T. ) ;
#939 = DIRECTION ( 'NONE',  ( 0.000000000000000000, 0.000000000000000000, -1.000000000000000000 ) ) ;
#940 = ORIENTED_EDGE ( 'NONE', *, *, #3703, .F. ) ;
#941 = ORIENTED_EDGE ( 'NONE', *, *, #10320, .T. ) ;
#942 = CARTESIAN_POINT ( 'NONE',  ( -34.50000000000000000, -112.9185811467682754, 1.870920967077121411 ) ) ;
#943 = CARTESIAN_POINT ( 'NONE',  ( 8.000000000000000000, -16.71027810728550733, -2.620268201066114688 ) ) ;
#944 = ORIENTED_EDGE ( 'NONE', *, *, #22014, .F. ) ;
#945 = ORIENTED_EDGE ( 'NONE', *, *, #7975, .T. ) ;
#947 = ADVANCED_FACE ( 'NONE', ( #11026 ), #32450, .T. ) ;
#946 = VECTOR ( 'NONE', #32460, 1000.000000000000000 ) ;
#948 = DIRECTION ( 'NONE',  ( -1.000000000000000000, 0.000000000000000000, 0.000000000000000000 ) ) ;
#949 = VECTOR ( 'NONE', #32359, 1000.000000000000000 ) ;
#950 = CARTESIAN_POINT ( 'NONE',  ( -35.93473953453761993, -113.9929510916434339, 13.11451721564123396 ) ) ;
#951 = DIRECTION ( 'NONE',  ( 0.000000000000000000, 0.3681245526846718685, 0.9297764858882537897 ) ) ;
#952 = DIRECTION ( 'NONE',  ( 0.000000000000000000, 0.8660254037844444808, -0.4999999999999898415 ) ) ;
#953 = CARTESIAN_POINT ( 'NONE',  ( -35.69272627125608466, -113.9929510916434339, 13.01835785830562209 ) ) ;
#954 = EDGE_CURVE ( 'NONE', #1113, #17966, #12270, .T. ) ;
#955 = CARTESIAN_POINT ( 'NONE',  ( -35.50000000000000000, -115.9929510916434481, 10.94631322572069365 ) ) ;
#956 = CIRCLE ( 'NONE', #18789, 11.00000000000000000 ) ;
#957 = UNCERTAINTY_MEASURE_WITH_UNIT (LENGTH_MEASURE( 1.000000000000000082E-05 ), #30348, 'distance_accuracy_value', 'NONE');
#958 = DIRECTION ( 'NONE',  ( 0.000000000000000000, 0.000000000000000000, 1.000000000000000000 ) ) ;
#959 = EDGE_CURVE ( 'NONE', #8132, #34240, #13437, .T. ) ;
#960 = LINE ( 'NONE', #1142, #3147 ) ;
#961 = EDGE_CURVE ( 'NONE', #25611, #15981, #4752, .T. ) ;
#962 = CARTESIAN_POINT ( 'NONE',  ( 0.000000000000000000, -42.60732521687585006, 19.80331771201643321 ) ) ;
#963 = DIRECTION ( 'NONE',  ( 0.000000000000000000, 0.000000000000000000, 1.000000000000000000 ) ) ;
#964 = CARTESIAN_POINT ( 'NONE',  ( 8.000000000000000000, 19.60123832284017453, 3.973846525876499225 ) ) ;
#965 = AXIS2_PLACEMENT_3D ( 'NONE', #19885, #17736, #3717 ) ;
#966 = VERTEX_POINT ( 'NONE', #18759 ) ;
#967 = AXIS2_PLACEMENT_3D ( 'NONE', #19477, #2946, #5809 ) ;
#968 = CARTESIAN_POINT ( 'NONE',  ( -39.49999999999999289, -12.06102132296306451, 91.30451528491657598 ) ) ;
#969 = DIRECTION ( 'NONE',  ( -1.734723475976807094E-16, 0.8660254037844444808, -0.4999999999999898415 ) ) ;
#970 = CARTESIAN_POINT ( 'NONE',  ( -55.00000000000000000, 19.99999999999998934, -25.00000000000000000 ) ) ;
#971 = CARTESIAN_POINT ( 'NONE',  ( -4.000000000000000000, 0.000000000000000000, 65.00000000000000000 ) ) ;
#972 = AXIS2_PLACEMENT_3D ( 'NONE', #19881, #17368, #9454 ) ;
#973 = EDGE_CURVE ( 'NONE', #27298, #22879, #2405, .T. ) ;
#974 = CONTEXT_DEPENDENT_SHAPE_REPRESENTATION ( #5766, #33640 ) ;
#975 = ADVANCED_FACE ( 'NONE', ( #5278 ), #19470, .T. ) ;
#976 = AXIS2_PLACEMENT_3D ( 'NONE', #5116, #7440, #29949 ) ;
#977 = DIRECTION ( 'NONE',  ( 1.387778780781445922E-16, -1.000000000000000000, 0.000000000000000000 ) ) ;
#978 = CYLINDRICAL_SURFACE ( 'NONE', #23374, 20.00000000000000355 ) ;
#979 = AXIS2_PLACEMENT_3D ( 'NONE', #5322, #32316, #24399 ) ;
#980 = ORIENTED_EDGE ( 'NONE', *, *, #19432, .T. ) ;
#981 = DIRECTION ( 'NONE',  ( -1.174092375852890260E-15, 4.222049128630259891E-16, 1.000000000000000000 ) ) ;
#982 = CARTESIAN_POINT ( 'NONE',  ( 65.00000000000001421, -25.98076211353320986, 84.99999999999994316 ) ) ;
#983 = DIRECTION ( 'NONE',  ( 0.000000000000000000, 0.000000000000000000, -1.000000000000000000 ) ) ;
#984 = VERTEX_POINT ( 'NONE', #11377 ) ;
#985 = ORIENTED_EDGE ( 'NONE', *, *, #1744, .F. ) ;
#986 = CARTESIAN_POINT ( 'NONE',  ( -37.74901162816868805, -113.3347980657955958, 9.433975545821549957 ) ) ;
#987 = EDGE_LOOP ( 'NONE', ( #17416, #22843, #3443, #6878 ) ) ;
#988 = VECTOR ( 'NONE', #31472, 1000.000000000000000 ) ;
#989 = ORIENTED_EDGE ( 'NONE', *, *, #3063, .T. ) ;
#990 = EDGE_LOOP ( 'NONE', ( #27082, #22848, #13873, #14916 ) ) ;
#991 = CARTESIAN_POINT ( 'NONE',  ( 0.000000000000000000, -2.710505431213761085E-17, 55.00000000000000000 ) ) ;
#992 = CIRCLE ( 'NONE', #28003, 47.49900000000001654 ) ;
#993 = CARTESIAN_POINT ( 'NONE',  ( 0.1374368770859640820, -4.808326913196061980, -0.7999999999999951594 ) ) ;
#994 = CIRCLE ( 'NONE', #2177, 52.00000000000000711 ) ;
#995 = CIRCLE ( 'NONE', #24010, 2.999999999999988898 ) ;
#996 = CYLINDRICAL_SURFACE ( 'NONE', #1858, 8.000000000000001776 ) ;
#997 = AXIS2_PLACEMENT_3D ( 'NONE', #354, #27740, #13703 ) ;
#998 = CARTESIAN_POINT ( 'NONE',  ( -35.95915003344517658, -114.9929510916434339, 13.11692036158763308 ) ) ;
#999 = DIRECTION ( 'NONE',  ( 1.000000000000000000, -0.000000000000000000, -0.000000000000000000 ) ) ;
#1000 = DIRECTION ( 'NONE',  ( 1.000000000000000000, -5.339440136655842133E-16, -1.047965281155519420E-16 ) ) ;
#1001 = VECTOR ( 'NONE', #23243, 1000.000000000000000 ) ;
#1002 = EDGE_CURVE ( 'NONE', #620, #27346, #26078, .T. ) ;
#1003 = CARTESIAN_POINT ( 'NONE',  ( -34.50000000000000000, -114.0998638248492085, 9.511920366020609308 ) ) ;
#1004 = DIRECTION ( 'NONE',  ( 0.000000000000000000, 0.000000000000000000, 1.000000000000000000 ) ) ;
#1005 = EDGE_CURVE ( 'NONE', #9557, #21816, #22163, .T. ) ;
#1006 = UNCERTAINTY_MEASURE_WITH_UNIT (LENGTH_MEASURE( 1.000000000000000082E-05 ), #14051, 'distance_accuracy_value', 'NONE');
#1007 = DIRECTION ( 'NONE',  ( -1.000000000000000000, 5.339440136655842133E-16, 1.047965281155519420E-16 ) ) ;
#1008 = ORIENTED_EDGE ( 'NONE', *, *, #33723, .T. ) ;
#1009 = CARTESIAN_POINT ( 'NONE',  ( -35.50000000000000000, -115.9929081983957104, 10.49113315946066294 ) ) ;
#1010 = CARTESIAN_POINT ( 'NONE',  ( -35.50000000000000711, -113.6318576702834804, 1.956056246348823580 ) ) ;
#1011 = CARTESIAN_POINT ( 'NONE',  ( -42.49999999999999289, -28.69486372867094559, 81.70096189432321410 ) ) ;
#1012 = CARTESIAN_POINT ( 'NONE',  ( -22.99999999999999645, 3.857637417314163478E-15, 0.000000000000000000 ) ) ;
#1013 = LINE ( 'NONE', #31248, #24550 ) ;
#1014 = AXIS2_PLACEMENT_3D ( 'NONE', #5144, #32851, #10892 ) ;
#1015 = DIRECTION ( 'NONE',  ( 1.000000000000000000, 0.000000000000000000, -0.000000000000000000 ) ) ;
#1016 = CYLINDRICAL_SURFACE ( 'NONE', #2626, 52.00000000000000711 ) ;
#1017 = AXIS2_PLACEMENT_3D ( 'NONE', #35598, #30184, #13621 ) ;
#1018 = CARTESIAN_POINT ( 'NONE',  ( 8.000000000000000000, 0.000000000000000000, 0.000000000000000000 ) ) ;
#1019 = CARTESIAN_POINT ( 'NONE',  ( -46.00000000000000000, -25.98076211353320275, 84.99999999999992895 ) ) ;
#1020 = ORIENTED_EDGE ( 'NONE', *, *, #16886, .T. ) ;
#1021 = CARTESIAN_POINT ( 'NONE',  ( -37.66520193420439711, -114.7490116281687023, 6.058975545821550845 ) ) ;
#1022 = CIRCLE ( 'NONE', #2766, 47.49900000000001654 ) ;
#1023 = CARTESIAN_POINT ( 'NONE',  ( 8.000000000000007105, -5.679790370315976666, -7.613867765417642097 ) ) ;
#1024 = PLANE ( 'NONE',  #11271 ) ;
#1025 = ORIENTED_EDGE ( 'NONE', *, *, #23489, .F. ) ;
#1026 = VERTEX_POINT ( 'NONE', #28115 ) ;
#1027 = AXIS2_PLACEMENT_3D ( 'NONE', #29683, #9873, #7366 ) ;
#1028 = CARTESIAN_POINT ( 'NONE',  ( 1.600000000000004086, -12.74999999999999822, -1.200000000000006617 ) ) ;
#1029 = DIRECTION ( 'NONE',  ( 1.000000000000000000, 0.000000000000000000, 0.000000000000000000 ) ) ;
#1030 = EDGE_LOOP ( 'NONE', ( #7294, #134, #29404, #21726, #18517, #9971 ) ) ;
#1031 = CARTESIAN_POINT ( 'NONE',  ( -36.94073759706866156, -111.0000000000000284, 7.128524454178450043 ) ) ;
#1032 = ORIENTED_EDGE ( 'NONE', *, *, #29947, .T. ) ;
#1033 = AXIS2_PLACEMENT_3D ( 'NONE', #11770, #24941, #790 ) ;
#1034 = CARTESIAN_POINT ( 'NONE',  ( 26.99999999999999645, 1.304248841091931221E-14, 0.000000000000000000 ) ) ;
#1035 = CARTESIAN_POINT ( 'NONE',  ( 50.00000000000000711, -2.775557561562891351E-14, 106.0000000000000000 ) ) ;
#1036 = APPLICATION_PROTOCOL_DEFINITION ( 'draft international standard', 'automotive_design', 1998, #31941 ) ;
#1037 = DIRECTION ( 'NONE',  ( -1.000000000000000000, -0.000000000000000000, -0.000000000000000000 ) ) ;
#1038 = VECTOR ( 'NONE', #35170, 1000.000000000000000 ) ;
#1039 = ORIENTED_EDGE ( 'NONE', *, *, #33488, .T. ) ;
#1040 = ORIENTED_EDGE ( 'NONE', *, *, #17483, .T. ) ;
#1041 = CARTESIAN_POINT ( 'NONE',  ( -34.49999999999998579, -25.98076211353322051, 84.99999999999992895 ) ) ;
#1042 = FACE_OUTER_BOUND ( 'NONE', #18730, .T. ) ;
#1043 = VECTOR ( 'NONE', #27752, 1000.000000000000000 ) ;
#1044 = ORIENTED_EDGE ( 'NONE', *, *, #17234, .T. ) ;
#1045 = CARTESIAN_POINT ( 'NONE',  ( 8.000000000000007105, 7.613867765417711375, -5.679790370315948245 ) ) ;
#1046 = VECTOR ( 'NONE', #5866, 1000.000000000000000 ) ;
#1047 = VECTOR ( 'NONE', #10594, 1000.000000000000000 ) ;
#1048 = CARTESIAN_POINT ( 'NONE',  ( -34.50000000000000000, -115.0140978167138712, -0.4685323525984310122 ) ) ;
#1049 = DIRECTION ( 'NONE',  ( 0.000000000000000000, 0.000000000000000000, 1.000000000000000000 ) ) ;
#1050 = CARTESIAN_POINT ( 'NONE',  ( -2.000000000000001776, 6.765000000000020997, -2.775557561562891351E-14 ) ) ;
#1051 = ADVANCED_FACE ( 'NONE', ( #25419 ), #33335, .T. ) ;
#1052 = CARTESIAN_POINT ( 'NONE',  ( -34.50000000000000000, -114.3793648455349654, 8.543708532059524074 ) ) ;
#1053 = PLANE ( 'NONE',  #11134 ) ;
#1054 = CARTESIAN_POINT ( 'NONE',  ( 70.00000000000001421, -30.47068043442695284, 88.33026027086506815 ) ) ;
#1055 = CARTESIAN_POINT ( 'NONE',  ( -38.99879592093640923, -114.9929510916434339, 12.67985367974111455 ) ) ;
#1056 = CARTESIAN_POINT ( 'NONE',  ( -4.000000000000000000, -2.710505431213761085E-17, -20.99999999999999645 ) ) ;
#1057 = AXIS2_PLACEMENT_3D ( 'NONE', #25207, #11856, #34016 ) ;
#1058 = DIRECTION ( 'NONE',  ( 0.000000000000000000, -1.000000000000000000, 1.067522139062650474E-15 ) ) ;
#1059 = DIRECTION ( 'NONE',  ( 0.000000000000000000, 0.000000000000000000, -1.000000000000000000 ) ) ;
#1060 = DIRECTION ( 'NONE',  ( -1.174092375852890260E-15, 4.222049128630259891E-16, 1.000000000000000000 ) ) ;
#1061 = EDGE_LOOP ( 'NONE', ( #19343, #9916, #7797, #11714 ) ) ;
#1062 = CARTESIAN_POINT ( 'NONE',  ( -4.000000000000000000, 0.000000000000000000, -40.00000000000000711 ) ) ;
#1063 = ORIENTED_EDGE ( 'NONE', *, *, #18291, .T. ) ;
#1064 = EDGE_CURVE ( 'NONE', #1802, #27521, #4812, .T. ) ;
#1065 = CARTESIAN_POINT ( 'NONE',  ( -39.16322519054178741, -111.9205845034225177, 3.433975545821550845 ) ) ;
#1066 = DIRECTION ( 'NONE',  ( 0.000000000000000000, 0.000000000000000000, -1.000000000000000000 ) ) ;
#1067 = CARTESIAN_POINT ( 'NONE',  ( -35.50000000000000711, -116.0140978167138712, -0.4685323525984310677 ) ) ;
#1068 = ORIENTED_EDGE ( 'NONE', *, *, #2171, .T. ) ;
#1069 = ORIENTED_EDGE ( 'NONE', *, *, #33286, .T. ) ;
#1070 = CARTESIAN_POINT ( 'NONE',  ( -0.1085714285714300953, -3.798448662927791819, -0.7999999999999951594 ) ) ;
#1071 = CARTESIAN_POINT ( 'NONE',  ( -9.999999999999994671, 0.000000000000000000, 52.00000000000000711 ) ) ;
#1072 = ORIENTED_EDGE ( 'NONE', *, *, #10606, .F. ) ;
#1073 = VECTOR ( 'NONE', #29292, 1000.000000000000000 ) ;
#1074 = VERTEX_POINT ( 'NONE', #8659 ) ;
#1075 = AXIS2_PLACEMENT_3D ( 'NONE', #10480, #13193, #34986 ) ;
#1076 = VECTOR ( 'NONE', #16065, 1000.000000000000000 ) ;
#1077 = CARTESIAN_POINT ( 'NONE',  ( -34.49999999999998579, -25.98076211353322051, 84.99999999999992895 ) ) ;
#1078 = ORIENTED_EDGE ( 'NONE', *, *, #3827, .T. ) ;
#1079 = CARTESIAN_POINT ( 'NONE',  ( -37.76916472181486739, -116.0245472910329880, 5.965225545821551734 ) ) ;
#1080 = CARTESIAN_POINT ( 'NONE',  ( 46.00000000000000000, -25.98076211353320275, 84.99999999999992895 ) ) ;
#1081 = EDGE_LOOP ( 'NONE', ( #34389, #6733, #17492, #18601 ) ) ;
#1082 = ORIENTED_EDGE ( 'NONE', *, *, #21395, .T. ) ;
#1083 = CARTESIAN_POINT ( 'NONE',  ( -35.50000000000000000, -114.8057644833805853, -2.624782352598442614 ) ) ;
#1084 = FACE_OUTER_BOUND ( 'NONE', #26395, .T. ) ;
#1085 = ORIENTED_EDGE ( 'NONE', *, *, #11721, .T. ) ;
#1086 = DIRECTION ( 'NONE',  ( 0.000000000000000000, -0.4817536741017037771, -0.8763066800438699122 ) ) ;
#1087 = EDGE_CURVE ( 'NONE', #7004, #1909, #24358, .T. ) ;
#1088 = CARTESIAN_POINT ( 'NONE',  ( -37.59808119975203766, -113.9929510916434339, 14.11551573851449071 ) ) ;
#1089 = EDGE_CURVE ( 'NONE', #18547, #14157, #25484, .T. ) ;
#1090 = LINE ( 'NONE', #12782, #18845 ) ;
#1091 = VECTOR ( 'NONE', #33567, 1000.000000000000000 ) ;
#1092 = CARTESIAN_POINT ( 'NONE',  ( -39.49999999999999289, -13.92619866229204106, 93.69175626110634880 ) ) ;
#1093 = CARTESIAN_POINT ( 'NONE',  ( -37.46874999999995737, -113.9929510916434339, 14.11852480586265024 ) ) ;
#1094 = CARTESIAN_POINT ( 'NONE',  ( 44.00000000000000000, 1.616533774874506480E-14, 0.000000000000000000 ) ) ;
#1095 = CARTESIAN_POINT ( 'NONE',  ( -36.03906250000000000, -114.9929510916434339, 13.11852480586264669 ) ) ;
#1096 =( LENGTH_UNIT ( ) NAMED_UNIT ( * ) SI_UNIT ( .MILLI., .METRE. ) );
#1097 = ORIENTED_EDGE ( 'NONE', *, *, #34186, .F. ) ;
#1098 = CIRCLE ( 'NONE', #1672, 20.00000000000000711 ) ;
#1099 = CARTESIAN_POINT ( 'NONE',  ( 1.599999999999990985, -4.694161725993254197E-16, -6.765000000000044977 ) ) ;
#1100 = DIRECTION ( 'NONE',  ( 1.000000000000000000, 0.000000000000000000, 0.000000000000000000 ) ) ;
#1101 = VERTEX_POINT ( 'NONE', #208 ) ;
#1102 = CARTESIAN_POINT ( 'NONE',  ( -35.50000000000000711, -114.9929510916434339, 11.38636890470581164 ) ) ;
#1103 = ORIENTED_EDGE ( 'NONE', *, *, #15865, .T. ) ;
#1104 = EDGE_CURVE ( 'NONE', #9474, #16728, #8811, .T. ) ;
#1105 = CARTESIAN_POINT ( 'NONE',  ( -37.88768952767750164, -115.9754527089670262, 1.972274454178448710 ) ) ;
#1106 = EDGE_CURVE ( 'NONE', #7183, #1299, #2524, .T. ) ;
#1107 = ORIENTED_EDGE ( 'NONE', *, *, #7172, .T. ) ;
#1108 = LINE ( 'NONE', #12077, #15873 ) ;
#1109 = ORIENTED_EDGE ( 'NONE', *, *, #2269, .F. ) ;
#1110 = CARTESIAN_POINT ( 'NONE',  ( -35.50000000000000000, -113.0140978167138996, -0.6247823525984306237 ) ) ;
#1111 = DIRECTION ( 'NONE',  ( -1.000000000000000000, 0.000000000000000000, 0.000000000000000000 ) ) ;
#1112 = CARTESIAN_POINT ( 'NONE',  ( 7.999999999999992895, 50.95304419620840264, -10.38206564895607897 ) ) ;
#1113 = VERTEX_POINT ( 'NONE', #30633 ) ;
#1114 = CARTESIAN_POINT ( 'NONE',  ( -37.88768952767750164, -115.9754527089670262, 1.972274454178448710 ) ) ;
#1115 = CARTESIAN_POINT ( 'NONE',  ( 4.000000000000000000, 4.898587196589412829E-16, 55.00000000000000711 ) ) ;
#1116 = CARTESIAN_POINT ( 'NONE',  ( -35.50000000000000711, -115.0795240838853886, -1.623175561345890472 ) ) ;
#1117 = ORIENTED_EDGE ( 'NONE', *, *, #9775, .T. ) ;
#1118 = ORIENTED_EDGE ( 'NONE', *, *, #2748, .F. ) ;
#1119 = DIRECTION ( 'NONE',  ( -1.000000000000000000, 0.000000000000000000, 0.000000000000000000 ) ) ;
#1120 = AXIS2_PLACEMENT_3D ( 'NONE', #13278, #13615, #19015 ) ;
#1121 = EDGE_CURVE ( 'NONE', #31360, #19035, #11897, .T. ) ;
#1122 = SURFACE_STYLE_USAGE ( .BOTH. , #3832 ) ;
#1123 = DIRECTION ( 'NONE',  ( -1.000000000000000000, 0.000000000000000000, 0.000000000000000000 ) ) ;
#1124 = EDGE_LOOP ( 'NONE', ( #30644, #31350 ) ) ;
#1125 = ORIENTED_EDGE ( 'NONE', *, *, #11845, .F. ) ;
#1126 = AXIS2_PLACEMENT_3D ( 'NONE', #27961, #30662, #22899 ) ;
#1127 = CARTESIAN_POINT ( 'NONE',  ( -34.50000000000000000, -116.0140978167138712, -0.4685323525984310677 ) ) ;
#1128 = CARTESIAN_POINT ( 'NONE',  ( 1.799999999999995604, 8.057851996059937582E-16, 4.200000000000014388 ) ) ;
#1129 = AXIS2_PLACEMENT_3D ( 'NONE', #2764, #24709, #30289 ) ;
#1130 = ORIENTED_EDGE ( 'NONE', *, *, #6598, .T. ) ;
#1131 = ORIENTED_EDGE ( 'NONE', *, *, #8517, .T. ) ;
#1132 = DIRECTION ( 'NONE',  ( -1.000000000000000000, 0.000000000000000000, 0.000000000000000000 ) ) ;
#1133 = EDGE_CURVE ( 'NONE', #14117, #4018, #916, .T. ) ;
#1134 = CARTESIAN_POINT ( 'NONE',  ( -37.50613590685470911, -113.9929510916434339, 13.11852378322482515 ) ) ;
#1135 = DIRECTION ( 'NONE',  ( -1.000000000000000000, -1.734723475976807094E-16, -0.000000000000000000 ) ) ;
#1136 = ADVANCED_FACE ( 'NONE', ( #19978 ), #5968, .T. ) ;
#1137 = CARTESIAN_POINT ( 'NONE',  ( 8.000000000000000000, -19.35373470438990395, 10.46102064772334295 ) ) ;
#1138 = EDGE_CURVE ( 'NONE', #15981, #31617, #31232, .T. ) ;
#1139 = CARTESIAN_POINT ( 'NONE',  ( -35.50000000000000000, -113.9929510916434339, 11.91443571948720148 ) ) ;
#1140 = CARTESIAN_POINT ( 'NONE',  ( -35.50000000000000000, -115.9929510916434481, 10.72628538622835670 ) ) ;
#1141 = FACE_OUTER_BOUND ( 'NONE', #15819, .T. ) ;
#1142 = CARTESIAN_POINT ( 'NONE',  ( 5.400000000000015454, -1.000000000000002220, 38.00000000000000000 ) ) ;
#1143 = EDGE_CURVE ( 'NONE', #23788, #31360, #16286, .T. ) ;
#1144 = CARTESIAN_POINT ( 'NONE',  ( 7.999999999999992895, 5.400000000000029665, -1.000000000000000888 ) ) ;
#1145 = FACE_OUTER_BOUND ( 'NONE', #2016, .T. ) ;
#1146 = DIRECTION ( 'NONE',  ( -1.000000000000000000, -0.000000000000000000, -0.000000000000000000 ) ) ;
#1147 = ADVANCED_FACE ( 'NONE', ( #33679 ), #378, .T. ) ;
#1148 = ORIENTED_EDGE ( 'NONE', *, *, #29574, .T. ) ;
#1149 = DIRECTION ( 'NONE',  ( 1.836970198721029934E-16, -1.000000000000000000, 0.000000000000000000 ) ) ;
#1150 = CARTESIAN_POINT ( 'NONE',  ( 0.000000000000000000, -20.99948489194452250, 42.60488980472776177 ) ) ;
#1151 = AXIS2_PLACEMENT_3D ( 'NONE', #25870, #19708, #17195 ) ;
#1152 = PRODUCT_DEFINITION_FORMATION_WITH_SPECIFIED_SOURCE ( 'ANY', '', #28786, .NOT_KNOWN. ) ;
#1153 = AXIS2_PLACEMENT_3D ( 'NONE', #33101, #33441, #33277 ) ;
#1154 = DIRECTION ( 'NONE',  ( 0.000000000000000000, 0.000000000000000000, 1.000000000000000000 ) ) ;
#1155 = FACE_OUTER_BOUND ( 'NONE', #2027, .T. ) ;
#1156 = ORIENTED_EDGE ( 'NONE', *, *, #678, .T. ) ;
#1157 = DIRECTION ( 'NONE',  ( -1.000000000000000000, 0.000000000000000000, 0.000000000000000000 ) ) ;
#1158 = CARTESIAN_POINT ( 'NONE',  ( -34.50000000000000000, -115.2751396785629510, -2.608751991713152307 ) ) ;
#1159 = DIRECTION ( 'NONE',  ( -1.000000000000000000, 0.000000000000000000, 0.000000000000000000 ) ) ;
#1160 = ORIENTED_EDGE ( 'NONE', *, *, #5332, .F. ) ;
#1161 = ORIENTED_EDGE ( 'NONE', *, *, #13775, .T. ) ;
#1162 = CARTESIAN_POINT ( 'NONE',  ( -37.99999999999998579, -113.9407375970686758, 3.753524454178448710 ) ) ;
#1163 = ORIENTED_EDGE ( 'NONE', *, *, #4540, .F. ) ;
#1164 = ADVANCED_FACE ( 'NONE', ( #8300 ), #19281, .T. ) ;
#1165 = SURFACE_STYLE_FILL_AREA ( #31929 ) ;
#1166 = ORIENTED_EDGE ( 'NONE', *, *, #2056, .T. ) ;
#1167 = VERTEX_POINT ( 'NONE', #33502 ) ;
#1168 = CARTESIAN_POINT ( 'NONE',  ( -34.50000000000000000, -113.0140978167142833, 0.8752176474019800478 ) ) ;
#1169 = EDGE_CURVE ( 'NONE', #3555, #2086, #8831, .T. ) ;
#1170 = ADVANCED_FACE ( 'NONE', ( #1274 ), #14768, .T. ) ;
#1171 = DIRECTION ( 'NONE',  ( 0.000000000000000000, 0.000000000000000000, -1.000000000000000000 ) ) ;
#1172 = CYLINDRICAL_SURFACE ( 'NONE', #34649, 19.99999999999998579 ) ;
#1173 = AXIS2_PLACEMENT_3D ( 'NONE', #22821, #28072, #3949 ) ;
#1174 = CARTESIAN_POINT ( 'NONE',  ( -35.50400759022159036, -114.9929510916434339, 12.68378527132497524 ) ) ;
#1175 = DIRECTION ( 'NONE',  ( 0.000000000000000000, 0.000000000000000000, 1.000000000000000000 ) ) ;
#1176 = EDGE_CURVE ( 'NONE', #9468, #31771, #34225, .T. ) ;
#1177 = AXIS2_PLACEMENT_3D ( 'NONE', #16266, #8007, #18991 ) ;
#1178 = CIRCLE ( 'NONE', #25910, 3.999999999999996447 ) ;
#1179 = CYLINDRICAL_SURFACE ( 'NONE', #28107, 8.000000000000051514 ) ;
#1180 = EDGE_CURVE ( 'NONE', #19478, #15493, #33568, .T. ) ;
#1181 = CARTESIAN_POINT ( 'NONE',  ( -34.50000000000000000, -114.9929510916434339, 10.94631322572069365 ) ) ;
#1182 = FACE_OUTER_BOUND ( 'NONE', #21588, .T. ) ;
#1183 = PRODUCT_DEFINITION_SHAPE ( 'NONE', 'NONE',  #8382 ) ;
#1184 = DIRECTION ( 'NONE',  ( -1.000000000000000000, 0.000000000000000000, 0.000000000000000000 ) ) ;
#1185 = EDGE_LOOP ( 'NONE', ( #21946, #29122, #4099, #24705 ) ) ;
#1186 = CARTESIAN_POINT ( 'NONE',  ( -35.50000000000000000, -115.9874658933321001, 10.35517832894335832 ) ) ;
#1187 = CARTESIAN_POINT ( 'NONE',  ( -35.50000000000000711, -112.1222502514821144, 1.343475657184566296 ) ) ;
#1188 = CARTESIAN_POINT ( 'NONE',  ( 7.999999999999992895, -44.25018368420762016, 27.31155879685168131 ) ) ;
#1189 = DIRECTION ( 'NONE',  ( 0.000000000000000000, -0.1253332335642905193, -0.9921147013144796523 ) ) ;
#1190 = DIRECTION ( 'NONE',  ( -1.000000000000000000, -1.734723475976807094E-16, -0.000000000000000000 ) ) ;
#1191 = CARTESIAN_POINT ( 'NONE',  ( 4.000000000000003553, -31.08872492059928305, -41.68322423723133596 ) ) ;
#1192 = DIRECTION ( 'NONE',  ( -1.000000000000000000, 0.000000000000000000, 0.000000000000000000 ) ) ;
#1193 = DIRECTION ( 'NONE',  ( -1.000000000000000000, -1.734723475976807094E-16, 0.000000000000000000 ) ) ;
#1194 = LINE ( 'NONE', #23141, #2335 ) ;
#1195 = ORIENTED_EDGE ( 'NONE', *, *, #24033, .T. ) ;
#1196 = CARTESIAN_POINT ( 'NONE',  ( -36.94073759706868287, -115.0000000000000000, 7.371475545821551734 ) ) ;
#1197 = DIRECTION ( 'NONE',  ( -1.174092375852890260E-15, 4.222049128630259891E-16, 1.000000000000000000 ) ) ;
#1198 = DIRECTION ( 'NONE',  ( 0.000000000000000000, 0.000000000000000000, 1.000000000000000000 ) ) ;
#1199 = ORIENTED_EDGE ( 'NONE', *, *, #32627, .T. ) ;
#1200 = ORIENTED_EDGE ( 'NONE', *, *, #17363, .T. ) ;
#1201 = DIRECTION ( 'NONE',  ( -1.000000000000000000, 0.000000000000000000, -0.000000000000000000 ) ) ;
#1202 = ORIENTED_EDGE ( 'NONE', *, *, #14635, .F. ) ;
#1203 = CARTESIAN_POINT ( 'NONE',  ( -33.97545270896703329, -115.1833782841879810, 5.590225545821552622 ) ) ;
#1204 = ORIENTED_EDGE ( 'NONE', *, *, #28400, .T. ) ;
#1205 = AXIS2_PLACEMENT_3D ( 'NONE', #29045, #1500, #20744 ) ;
#1206 = CIRCLE ( 'NONE', #18435, 3.999999999999996447 ) ;
#1207 = EDGE_CURVE ( 'NONE', #32151, #22471, #34416, .T. ) ;
#1208 = AXIS2_PLACEMENT_3D ( 'NONE', #4851, #21024, #34736 ) ;
#1209 = DIRECTION ( 'NONE',  ( -1.000000000000000000, 0.000000000000000000, 0.000000000000000000 ) ) ;
#1210 = EDGE_CURVE ( 'NONE', #15079, #24598, #29193, .T. ) ;
#1211 = CARTESIAN_POINT ( 'NONE',  ( 4.000000000000000000, 6.359167119270718871, -18.96209359615085788 ) ) ;
#1212 = FACE_BOUND ( 'NONE', #25738, .T. ) ;
#1213 = APPLICATION_PROTOCOL_DEFINITION ( 'draft international standard', 'automotive_design', 1998, #6862 ) ;
#1214 = DIRECTION ( 'NONE',  ( 0.000000000000000000, 0.000000000000000000, 1.000000000000000000 ) ) ;
#1215 = ORIENTED_EDGE ( 'NONE', *, *, #24076, .F. ) ;
#1216 = ORIENTED_EDGE ( 'NONE', *, *, #6898, .F. ) ;
#1217 = LINE ( 'NONE', #29120, #16781 ) ;
#1218 = DIRECTION ( 'NONE',  ( 0.000000000000000000, -6.938893903907226800E-15, 1.000000000000000000 ) ) ;
#1219 = AXIS2_PLACEMENT_3D ( 'NONE', #31997, #21184, #34528 ) ;
#1220 = ORIENTED_EDGE ( 'NONE', *, *, #17331, .T. ) ;
#1221 = DIRECTION ( 'NONE',  ( 1.000000000000000000, -0.000000000000000000, 0.000000000000000000 ) ) ;
#1222 = CARTESIAN_POINT ( 'NONE',  ( -34.50000000000000000, -113.2224311500466030, -0.6247823525984269599 ) ) ;
#1223 = DIRECTION ( 'NONE',  ( -1.000000000000000000, 0.000000000000000000, 0.000000000000000000 ) ) ;
#1224 = DIRECTION ( 'NONE',  ( -1.000000000000000000, 0.000000000000000000, 0.000000000000000000 ) ) ;
#1225 = CARTESIAN_POINT ( 'NONE',  ( -34.50000000000000000, -114.1556834383649459, 8.511484393387789282 ) ) ;
#1226 = CARTESIAN_POINT ( 'NONE',  ( -0.2142857142857362840, -10.49781318335649161, -1.200000000000006617 ) ) ;
#1227 = CARTESIAN_POINT ( 'NONE',  ( -38.97545270896704039, -113.1123104723225055, 2.347274454178448710 ) ) ;
#1228 = CIRCLE ( 'NONE', #27681, 0.1999999999999992339 ) ;
#1229 =( GEOMETRIC_REPRESENTATION_CONTEXT ( 3 ) GLOBAL_UNCERTAINTY_ASSIGNED_CONTEXT ( ( #20365 ) ) GLOBAL_UNIT_ASSIGNED_CONTEXT ( ( #10687, #18958, #29954 ) ) REPRESENTATION_CONTEXT ( 'NONE', 'WORKASPACE' ) );
#1230 = CARTESIAN_POINT ( 'NONE',  ( -34.50000000000000000, -114.1371041221139109, 8.509266650872710613 ) ) ;
#1232 = CARTESIAN_POINT ( 'NONE',  ( -1.999999999999998224, -1.846447412309851863E-16, -4.200000000000014388 ) ) ;
#1231 = VECTOR ( 'NONE', #22493, 1000.000000000000000 ) ;
#1233 = DIRECTION ( 'NONE',  ( -1.000000000000000000, 0.000000000000000000, -0.000000000000000000 ) ) ;
#1234 = DIRECTION ( 'NONE',  ( 0.000000000000000000, 0.000000000000000000, 1.000000000000000000 ) ) ;
#1235 = CARTESIAN_POINT ( 'NONE',  ( 65.00000000000001421, -25.98076211353320986, 84.99999999999994316 ) ) ;
#1236 = DIRECTION ( 'NONE',  ( 1.000000000000000000, -0.000000000000000000, -0.000000000000000000 ) ) ;
#1237 = ORIENTED_EDGE ( 'NONE', *, *, #26784, .F. ) ;
#1238 = CARTESIAN_POINT ( 'NONE',  ( -34.00000000000000000, -113.9407375970686758, 5.496475545821551734 ) ) ;
#1239 = DIRECTION ( 'NONE',  ( 0.000000000000000000, 0.000000000000000000, -1.000000000000000000 ) ) ;
#1240 = CARTESIAN_POINT ( 'NONE',  ( -35.50000000000000000, -113.3822401464312719, 0.9191614010536472978 ) ) ;
#1241 = VERTEX_POINT ( 'NONE', #31342 ) ;
#1242 = ORIENTED_EDGE ( 'NONE', *, *, #4478, .F. ) ;
#1243 = PLANE ( 'NONE',  #13482 ) ;
#1244 = ORIENTED_EDGE ( 'NONE', *, *, #30141, .T. ) ;
#1245 = ORIENTED_EDGE ( 'NONE', *, *, #9446, .F. ) ;
#1246 = EDGE_CURVE ( 'NONE', #16735, #21743, #18612, .T. ) ;
#1247 = FACE_OUTER_BOUND ( 'NONE', #24776, .T. ) ;
#1248 = CARTESIAN_POINT ( 'NONE',  ( -34.97545270896703329, -114.7691647218148745, 2.590225545821551290 ) ) ;
#1249 = DIRECTION ( 'NONE',  ( 0.000000000000000000, -0.9672551082808338307, 0.2538061376417689030 ) ) ;
#1250 = DIRECTION ( 'NONE',  ( 1.000000000000000000, 0.000000000000000000, 0.000000000000000000 ) ) ;
#1251 = ORIENTED_EDGE ( 'NONE', *, *, #31643, .F. ) ;
#1252 = ORIENTED_EDGE ( 'NONE', *, *, #745, .F. ) ;
#1253 = CARTESIAN_POINT ( 'NONE',  ( -35.50000000000000000, -115.2751396785629510, -2.608751991713152307 ) ) ;
#1254 = EDGE_CURVE ( 'NONE', #9156, #35591, #5972, .T. ) ;
#1255 = DIRECTION ( 'NONE',  ( 1.000000000000000000, -0.000000000000000000, -0.000000000000000000 ) ) ;
#1256 = VERTEX_POINT ( 'NONE', #17999 ) ;
#1257 = CARTESIAN_POINT ( 'NONE',  ( -37.99999897736218202, -114.9929510916434339, 12.62466071271732915 ) ) ;
#1258 = PRESENTATION_LAYER_ASSIGNMENT (  '', '', ( #4155 ) ) ;
#1259 = CARTESIAN_POINT ( 'NONE',  ( -34.50000000000000000, -114.1021862393805577, 9.512197583835053649 ) ) ;
#1260 = CARTESIAN_POINT ( 'NONE',  ( -50.00000000000000000, 0.000000000000000000, 70.00000000000000000 ) ) ;
#1261 = CARTESIAN_POINT ( 'NONE',  ( 7.999999999999992895, -36.05989434073634925, 30.12041790338604130 ) ) ;
#1262 = CARTESIAN_POINT ( 'NONE',  ( -38.99924736195577424, -113.9929510916434339, 12.66759465831984599 ) ) ;
#1263 = DIRECTION ( 'NONE',  ( -1.000000000000000000, 0.000000000000000000, 0.000000000000000000 ) ) ;
#1264 = CARTESIAN_POINT ( 'NONE',  ( -36.24999999999983658, -114.9929510916434339, 13.11852480586264669 ) ) ;
#1265 = DIRECTION ( 'NONE',  ( -1.000000000000000000, 0.000000000000000000, 0.000000000000000000 ) ) ;
#1266 = EDGE_LOOP ( 'NONE', ( #9909, #9614 ) ) ;
#1267 = DIRECTION ( 'NONE',  ( 0.000000000000000000, -1.000000000000000000, -1.048062100069320848E-14 ) ) ;
#1268 = CARTESIAN_POINT ( 'NONE',  ( 5.400000000000015454, -1.000000000000002220, 38.00000000000000000 ) ) ;
#1269 = EDGE_LOOP ( 'NONE', ( #4591, #17269, #21862, #33608, #20840, #6158, #6470, #4785 ) ) ;
#1270 = CARTESIAN_POINT ( 'NONE',  ( -35.50000000000000711, -114.9925223117477202, 10.47601618151863079 ) ) ;
#1271 = ORIENTED_EDGE ( 'NONE', *, *, #26959, .F. ) ;
#1272 = VECTOR ( 'NONE', #31102, 1000.000000000000000 ) ;
#1273 = CIRCLE ( 'NONE', #116, 15.49899999999999700 ) ;
#1274 = FACE_OUTER_BOUND ( 'NONE', #3438, .T. ) ;
#1275 = VERTEX_POINT ( 'NONE', #9555 ) ;
#1276 = CYLINDRICAL_SURFACE ( 'NONE', #10733, 4.800000000000000711 ) ;
#1277 = ORIENTED_EDGE ( 'NONE', *, *, #33014, .F. ) ;
#1278 = CARTESIAN_POINT ( 'NONE',  ( -34.50000000000000000, -113.0140978167138712, 0.8752176474016720720 ) ) ;
#1279 = CARTESIAN_POINT ( 'NONE',  ( 3.799999999999999822, 0.000000000000000000, 49.10000000000000142 ) ) ;
#1280 = CARTESIAN_POINT ( 'NONE',  ( -38.45611840935523418, -115.3723087153909432, 8.066024454178448266 ) ) ;
#1281 = ORIENTED_EDGE ( 'NONE', *, *, #9466, .T. ) ;
#1282 = CARTESIAN_POINT ( 'NONE',  ( -37.76916472181487450, -111.9754527089670404, 2.534774454178448710 ) ) ;
#1283 = MECHANICAL_DESIGN_GEOMETRIC_PRESENTATION_REPRESENTATION (  '', ( #34058 ), #23722 ) ;
#1284 = FACE_OUTER_BOUND ( 'NONE', #24156, .T. ) ;
#1285 = EDGE_CURVE ( 'NONE', #9210, #9731, #26681, .T. ) ;
#1286 = CARTESIAN_POINT ( 'NONE',  ( -35.50000000000000711, -113.0557643173828524, -1.624792769101735868 ) ) ;
#1287 = ORIENTED_EDGE ( 'NONE', *, *, #1502, .T. ) ;
#1288 = ORIENTED_EDGE ( 'NONE', *, *, #21239, .T. ) ;
#1289 = EDGE_CURVE ( 'NONE', #9085, #7270, #12869, .T. ) ;
#1290 = FACE_OUTER_BOUND ( 'NONE', #13785, .T. ) ;
#1291 =( LENGTH_UNIT ( ) NAMED_UNIT ( * ) SI_UNIT ( .MILLI., .METRE. ) );
#1292 = CARTESIAN_POINT ( 'NONE',  ( -42.49999999999999289, -27.48076211353326670, 88.99999999999994316 ) ) ;
#1293 = EDGE_LOOP ( 'NONE', ( #32920, #21265, #23659, #24898 ) ) ;
#1294 = ORIENTED_EDGE ( 'NONE', *, *, #20447, .T. ) ;
#1295 = CARTESIAN_POINT ( 'NONE',  ( -34.50000000000000000, -112.3995503592287690, -1.424448457485529618 ) ) ;
#1296 = DIRECTION ( 'NONE',  ( -1.000000000000000000, 0.000000000000000000, 0.000000000000000000 ) ) ;
#1297 = AXIS2_PLACEMENT_3D ( 'NONE', #14046, #9000, #14227 ) ;
#1298 = ADVANCED_FACE ( 'NONE', ( #6669 ), #9134, .T. ) ;
#1299 = VERTEX_POINT ( 'NONE', #9914 ) ;
#1300 = VECTOR ( 'NONE', #31939, 1000.000000000000000 ) ;
#1301 = VERTEX_POINT ( 'NONE', #12081 ) ;
#1302 = DIRECTION ( 'NONE',  ( -1.000000000000000000, 8.673617379884106963E-17, -1.502314598737155580E-16 ) ) ;
#1303 = CARTESIAN_POINT ( 'NONE',  ( -37.99359134332094357, -113.9929510916434339, 12.69998175888958514 ) ) ;
#1304 = DIRECTION ( 'NONE',  ( 0.000000000000000000, 0.000000000000000000, -1.000000000000000000 ) ) ;
#1305 = CARTESIAN_POINT ( 'NONE',  ( -36.03906250000000000, -113.9929510916434339, 13.11852480586264846 ) ) ;
#1306 = CARTESIAN_POINT ( 'NONE',  ( -35.50005019975638021, -115.9929510916434481, 12.62670525340498351 ) ) ;
#1307 = PRODUCT_DEFINITION_CONTEXT ( 'detailed design', #14895, 'design' ) ;
#1308 = CARTESIAN_POINT ( 'NONE',  ( 5.400000000000085620, -1.000000000000049516, -44.50000000000000000 ) ) ;
#1309 = VECTOR ( 'NONE', #7772, 1000.000000000000000 ) ;
#1310 = CIRCLE ( 'NONE', #10514, 8.000000000000007105 ) ;
#1311 = FACE_OUTER_BOUND ( 'NONE', #20645, .T. ) ;
#1312 = VECTOR ( 'NONE', #33377, 1000.000000000000000 ) ;
#1313 = DIRECTION ( 'NONE',  ( 0.000000000000000000, 0.000000000000000000, 1.000000000000000000 ) ) ;
#1314 = DIRECTION ( 'NONE',  ( 0.000000000000000000, -8.326672684688666165E-15, 1.000000000000000000 ) ) ;
#1315 = CARTESIAN_POINT ( 'NONE',  ( 4.000000000000003553, -19.35373470438975119, -10.46102064772362183 ) ) ;
#1316 = EDGE_CURVE ( 'NONE', #24884, #17787, #25538, .T. ) ;
#1317 = VERTEX_POINT ( 'NONE', #31534 ) ;
#1318 = DIRECTION ( 'NONE',  ( 0.000000000000000000, 0.000000000000000000, -1.000000000000000000 ) ) ;
#1319 = VECTOR ( 'NONE', #603, 1000.000000000000000 ) ;
#1320 = CIRCLE ( 'NONE', #19123, 52.00000000000000711 ) ;
#1321 = CARTESIAN_POINT ( 'NONE',  ( -35.50000000000000711, -113.8159288351371714, 1.978028123174813802 ) ) ;
#1322 = CYLINDRICAL_SURFACE ( 'NONE', #32817, 3.799999999999999822 ) ;
#1323 = AXIS2_PLACEMENT_3D ( 'NONE', #31219, #31395, #28341 ) ;
#1324 = CARTESIAN_POINT ( 'NONE',  ( -35.50000000000000711, -114.1152303497977414, 9.513755561829650986 ) ) ;
#1325 = CARTESIAN_POINT ( 'NONE',  ( -34.49999999999998579, -25.98076211353322051, 84.99999999999992895 ) ) ;
#1326 = ORIENTED_EDGE ( 'NONE', *, *, #32143, .T. ) ;
#1327 = CARTESIAN_POINT ( 'NONE',  ( 8.000000000000000000, 0.000000000000000000, 0.000000000000000000 ) ) ;
#1328 = ADVANCED_FACE ( 'NONE', ( #12443 ), #23786, .F. ) ;
#1329 = CARTESIAN_POINT ( 'NONE',  ( -34.50000000000000000, -113.6807644833805995, -2.624782352598442614 ) ) ;
#1330 = DIRECTION ( 'NONE',  ( 0.000000000000000000, 0.000000000000000000, 1.000000000000000000 ) ) ;
#1331 = VERTEX_POINT ( 'NONE', #34423 ) ;
#1332 = ORIENTED_EDGE ( 'NONE', *, *, #34804, .T. ) ;
#1333 = EDGE_CURVE ( 'NONE', #31962, #25998, #21476, .T. ) ;
#1334 = CARTESIAN_POINT ( 'NONE',  ( -36.64504884055823908, -115.0245472910329880, 1.784774454178449155 ) ) ;
#1335 = ADVANCED_FACE ( 'NONE', ( #18007 ), #20877, .T. ) ;
#1336 = ORIENTED_EDGE ( 'NONE', *, *, #33171, .F. ) ;
#1338 = ORIENTED_EDGE ( 'NONE', *, *, #30581, .T. ) ;
#1337 = AXIS2_PLACEMENT_3D ( 'NONE', #22806, #33808, #28399 ) ;
#1339 = EDGE_LOOP ( 'NONE', ( #24643, #28837, #2913, #12705 ) ) ;
#1340 = CARTESIAN_POINT ( 'NONE',  ( -35.50000000000000000, -113.8474311500459777, -0.6247823525984269599 ) ) ;
#1341 = AXIS2_PLACEMENT_3D ( 'NONE', #13158, #21408, #35126 ) ;
#1342 = EDGE_CURVE ( 'NONE', #27693, #32697, #31262, .T. ) ;
#1343 = DIRECTION ( 'NONE',  ( -0.000000000000000000, 1.611597878369477150E-16, -1.000000000000000000 ) ) ;
#1344 = EDGE_CURVE ( 'NONE', #4384, #12104, #12293, .T. ) ;
#1345 = DIRECTION ( 'NONE',  ( 1.000000000000000000, -5.339440136655842133E-16, -1.047965281155519420E-16 ) ) ;
#1346 = APPLICATION_CONTEXT ( 'automotive_design' ) ;
#1347 = VECTOR ( 'NONE', #5447, 1000.000000000000000 ) ;
#1348 = CARTESIAN_POINT ( 'NONE',  ( -35.49999931242378892, -114.9929510916434339, 12.61439929482945566 ) ) ;
#1349 = DIRECTION ( 'NONE',  ( 0.000000000000000000, 0.000000000000000000, 1.000000000000000000 ) ) ;
#1350 = LINE ( 'NONE', #28720, #24089 ) ;
#1351 = CARTESIAN_POINT ( 'NONE',  ( -34.50120407906360498, -114.9929510916434339, 12.67985367974112343 ) ) ;
#1352 = CARTESIAN_POINT ( 'NONE',  ( -10.00000000000000178, 0.000000000000000000, 0.000000000000000000 ) ) ;
#1353 = UNCERTAINTY_MEASURE_WITH_UNIT (LENGTH_MEASURE( 1.000000000000000082E-05 ), #3538, 'distance_accuracy_value', 'NONE');
#1354 = DIRECTION ( 'NONE',  ( 0.000000000000000000, -0.1736481776669211718, -0.9848077530122096857 ) ) ;
#1355 = EDGE_LOOP ( 'NONE', ( #23025, #6634 ) ) ;
#1356 = CARTESIAN_POINT ( 'NONE',  ( -35.50000000000000000, -115.9929510916434481, 11.73841344789270202 ) ) ;
#1357 = CARTESIAN_POINT ( 'NONE',  ( -35.50000000000000711, -115.1446187476384040, -1.616767172155725740 ) ) ;
#1358 =( NAMED_UNIT ( * ) SI_UNIT ( $, .STERADIAN. ) SOLID_ANGLE_UNIT ( ) );
#1359 = DIRECTION ( 'NONE',  ( -1.174092375852890260E-15, 4.222049128630259891E-16, 1.000000000000000000 ) ) ;
#1360 = EDGE_CURVE ( 'NONE', #6851, #27996, #26102, .T. ) ;
#1361 = CYLINDRICAL_SURFACE ( 'NONE', #19930, 22.00000000000000000 ) ;
#1362 = AXIS2_PLACEMENT_3D ( 'NONE', #33621, #17230, #14707 ) ;
#1363 = CARTESIAN_POINT ( 'NONE',  ( -42.49999999999999289, -28.31857036507959791, 80.03062855292519373 ) ) ;
#1364 = CARTESIAN_POINT ( 'NONE',  ( 7.999999999999992895, 0.000000000000000000, 0.000000000000000000 ) ) ;
#1365 = PRODUCT_RELATED_PRODUCT_CATEGORY ( 'part', '', ( #18142 ) ) ;
#1366 = FACE_OUTER_BOUND ( 'NONE', #1458, .T. ) ;
#1367 = DIRECTION ( 'NONE',  ( 0.000000000000000000, 0.000000000000000000, 1.000000000000000000 ) ) ;
#1368 = ORIENTED_EDGE ( 'NONE', *, *, #5758, .F. ) ;
#1369 = EDGE_CURVE ( 'NONE', #32690, #28784, #14777, .T. ) ;
#1370 = CARTESIAN_POINT ( 'NONE',  ( -36.52652403469559061, -114.9754527089670262, 5.777725545821551734 ) ) ;
#1371 = DIRECTION ( 'NONE',  ( -1.000000000000000000, 0.000000000000000000, 0.000000000000000000 ) ) ;
#1372 = LINE ( 'NONE', #17554, #8380 ) ;
#1373 = EDGE_LOOP ( 'NONE', ( #13603, #23594 ) ) ;
#1374 = VERTEX_POINT ( 'NONE', #1112 ) ;
#1375 = AXIS2_PLACEMENT_3D ( 'NONE', #34845, #33025, #24748 ) ;
#1376 = DIRECTION ( 'NONE',  ( 0.000000000000000000, -0.9929510916431035783, 0.1185248058626076212 ) ) ;
#1377 = ORIENTED_EDGE ( 'NONE', *, *, #12991, .T. ) ;
#1378 = EDGE_CURVE ( 'NONE', #15078, #7666, #28381, .T. ) ;
#1379 = CARTESIAN_POINT ( 'NONE',  ( -38.30190309005061522, -111.0245472910330022, 9.527725545821551734 ) ) ;
#1380 = EDGE_CURVE ( 'NONE', #24945, #10090, #3111, .T. ) ;
#1381 = ORIENTED_EDGE ( 'NONE', *, *, #35324, .T. ) ;
#1382 = SURFACE_SIDE_STYLE ('',( #4458 ) ) ;
#1383 = CARTESIAN_POINT ( 'NONE',  ( -4.000000000000000000, -2.710505431213761085E-17, -30.00000000000000711 ) ) ;
#1384 = DIRECTION ( 'NONE',  ( -1.000000000000000000, -0.000000000000000000, -0.000000000000000000 ) ) ;
#1385 = SHAPE_DEFINITION_REPRESENTATION ( #19819, #11863 ) ;
#1386 = ADVANCED_FACE ( 'NONE', ( #10817 ), #35486, .F. ) ;
#1387 = CARTESIAN_POINT ( 'NONE',  ( 7.999999999999992895, 0.000000000000000000, 0.000000000000000000 ) ) ;
#1388 = ORIENTED_EDGE ( 'NONE', *, *, #27301, .T. ) ;
#1389 = EDGE_LOOP ( 'NONE', ( #12090, #20252 ) ) ;
#1390 = CARTESIAN_POINT ( 'NONE',  ( -35.50000000000000711, -114.0000000000000853, 2.000000000000001776 ) ) ;
#1391 = DIRECTION ( 'NONE',  ( 0.000000000000000000, 0.000000000000000000, 1.000000000000000000 ) ) ;
#1392 = ORIENTED_EDGE ( 'NONE', *, *, #8153, .T. ) ;
#1393 = FACE_BOUND ( 'NONE', #12136, .T. ) ;
#1394 = CARTESIAN_POINT ( 'NONE',  ( -34.50000000000000000, -112.4434344552011282, 1.705278471174987986 ) ) ;
#1395 = CARTESIAN_POINT ( 'NONE',  ( 0.000000000000000000, 0.000000000000000000, 0.000000000000000000 ) ) ;
#1396 = FACE_OUTER_BOUND ( 'NONE', #1571, .T. ) ;
#1397 =( REPRESENTATION_RELATIONSHIP ('NONE','NONE', #26607, #15534 ) REPRESENTATION_RELATIONSHIP_WITH_TRANSFORMATION ( #5846 )SHAPE_REPRESENTATION_RELATIONSHIP( ) );
#1398 = AXIS2_PLACEMENT_3D ( 'NONE', #24633, #21379, #29506 ) ;
#1399 = CARTESIAN_POINT ( 'NONE',  ( -37.48437500000004263, -115.9929510916434481, 14.11852480586265024 ) ) ;
#1400 = CIRCLE ( 'NONE', #5998, 13.99999999999999645 ) ;
#1401 = CARTESIAN_POINT ( 'NONE',  ( 0.1085714285714300953, -3.798448662927791819, 0.000000000000000000 ) ) ;
#1402 = DIRECTION ( 'NONE',  ( 0.000000000000000000, 0.000000000000000000, -1.000000000000000000 ) ) ;
#1403 = CARTESIAN_POINT ( 'NONE',  ( -39.00000000000000711, -114.9929510916434339, 12.57451923796417503 ) ) ;
#1404 = LINE ( 'NONE', #12027, #34902 ) ;
#1405 = EDGE_CURVE ( 'NONE', #11997, #7078, #5393, .T. ) ;
#1406 = DIRECTION ( 'NONE',  ( -1.000000000000000000, -1.836970198721029934E-16, 0.000000000000000000 ) ) ;
#1407 = CARTESIAN_POINT ( 'NONE',  ( 0.000000000000000000, -2.710505431213761085E-17, -45.00000000000000000 ) ) ;
#1408 = LINE ( 'NONE', #20464, #3158 ) ;
#1409 = EDGE_CURVE ( 'NONE', #869, #29036, #15654, .T. ) ;
#1410 = ADVANCED_FACE ( 'NONE', ( #2372, #2728 ), #32242, .F. ) ;
#1411 = DIRECTION ( 'NONE',  ( 1.000000000000000000, 0.000000000000000000, 0.000000000000000000 ) ) ;
#1412 = ORIENTED_EDGE ( 'NONE', *, *, #13569, .T. ) ;
#1413 = CARTESIAN_POINT ( 'NONE',  ( -40.02454729103296671, -112.8166217158120332, 6.340225545821551734 ) ) ;
#1414 = CARTESIAN_POINT ( 'NONE',  ( 0.000000000000000000, -6.109652351742118626, 46.58570277113506819 ) ) ;
#1415 = CARTESIAN_POINT ( 'NONE',  ( -35.50000000000000000, -113.0140978167136581, -0.6247823525984268489 ) ) ;
#1416 = EDGE_LOOP ( 'NONE', ( #5626, #28974, #6098, #6104 ) ) ;
#1417 = ORIENTED_EDGE ( 'NONE', *, *, #6170, .T. ) ;
#1418 = CARTESIAN_POINT ( 'NONE',  ( 0.000000000000000000, -19.44205635905572649, 43.33776004284603545 ) ) ;
#1419 = DIRECTION ( 'NONE',  ( -1.000000000000000000, -0.000000000000000000, -0.000000000000000000 ) ) ;
#1420 = ORIENTED_EDGE ( 'NONE', *, *, #10163, .F. ) ;
#1421 = EDGE_CURVE ( 'NONE', #33849, #12864, #8271, .T. ) ;
#1422 = ORIENTED_EDGE ( 'NONE', *, *, #667, .F. ) ;
#1423 = EDGE_CURVE ( 'NONE', #19035, #2094, #30704, .T. ) ;
#1424 = ORIENTED_EDGE ( 'NONE', *, *, #13704, .F. ) ;
#1425 = CARTESIAN_POINT ( 'NONE',  ( 0.000000000000000000, 0.000000000000000000, -53.39999999999999858 ) ) ;
#1426 = CIRCLE ( 'NONE', #24430, 4.000000000000000000 ) ;
#1427 = CARTESIAN_POINT ( 'NONE',  ( -35.54388159064475872, -115.3723087153909432, 7.183975545821551734 ) ) ;
#1428 = AXIS2_PLACEMENT_3D ( 'NONE', #32944, #339, #24842 ) ;
#1429 = CYLINDRICAL_SURFACE ( 'NONE', #5829, 8.000000000000001776 ) ;
#1430 = VERTEX_POINT ( 'NONE', #2549 ) ;
#1431 = ORIENTED_EDGE ( 'NONE', *, *, #8430, .T. ) ;
#1432 = CARTESIAN_POINT ( 'NONE',  ( -35.50000000000000000, -117.0140978167138854, -0.4685323525984309012 ) ) ;
#1433 = DIRECTION ( 'NONE',  ( -1.000000000000000000, 0.000000000000000000, 1.691777834109591283E-31 ) ) ;
#1434 = DIRECTION ( 'NONE',  ( 0.000000000000000000, 0.000000000000000000, -1.000000000000000000 ) ) ;
#1435 = EDGE_LOOP ( 'NONE', ( #7725, #862, #34876, #6549 ) ) ;
#1436 = CARTESIAN_POINT ( 'NONE',  ( -38.00000000000000711, -114.9929510916434339, 12.57451923796417503 ) ) ;
#1437 = CIRCLE ( 'NONE', #35374, 8.000000000000000000 ) ;
#1438 = CARTESIAN_POINT ( 'NONE',  ( -34.50000000000000000, -114.9929510916434339, 10.94631322572069365 ) ) ;
#1439 = DIRECTION ( 'NONE',  ( 0.000000000000000000, 0.8660254037844398178, -0.4999999999999980571 ) ) ;
#1440 = CARTESIAN_POINT ( 'NONE',  ( -37.18750000000006395, -114.9929510916434339, 13.11852480586264669 ) ) ;
#1441 = DIRECTION ( 'NONE',  ( 0.000000000000000000, 0.2486898871648482723, 0.9685831611286327414 ) ) ;
#1442 = CARTESIAN_POINT ( 'NONE',  ( -35.98977351030467986, -113.9929510916434339, 14.11852173794918563 ) ) ;
#1443 = LINE ( 'NONE', #17456, #9565 ) ;
#1444 = CARTESIAN_POINT ( 'NONE',  ( -36.00585935943767169, -114.9929510916434339, 13.11852578240983291 ) ) ;
#1445 = LINE ( 'NONE', #31682, #19350 ) ;
#1446 = ORIENTED_EDGE ( 'NONE', *, *, #15244, .T. ) ;
#1448 = VECTOR ( 'NONE', #31600, 1000.000000000000000 ) ;
#1447 = DIRECTION ( 'NONE',  ( 1.000000000000000000, -0.000000000000000000, -0.000000000000000000 ) ) ;
#1449 = LINE ( 'NONE', #25771, #3133 ) ;
#1450 = EDGE_CURVE ( 'NONE', #9747, #13957, #18039, .T. ) ;
#1451 = CIRCLE ( 'NONE', #16950, 7.499999999999992895 ) ;
#1452 = VERTEX_POINT ( 'NONE', #26851 ) ;
#1453 = CARTESIAN_POINT ( 'NONE',  ( -35.52552712174884419, -114.9929510916434339, 12.77960891308624447 ) ) ;
#1454 = ORIENTED_EDGE ( 'NONE', *, *, #21547, .T. ) ;
#1455 = CARTESIAN_POINT ( 'NONE',  ( -36.94073759706868287, -112.0000000000000142, 2.628524454178448710 ) ) ;
#1456 = ORIENTED_EDGE ( 'NONE', *, *, #16234, .F. ) ;
#1457 = FACE_OUTER_BOUND ( 'NONE', #826, .T. ) ;
#1458 = EDGE_LOOP ( 'NONE', ( #11792, #3585, #10476, #29290 ) ) ;
#1459 = AXIS2_PLACEMENT_3D ( 'NONE', #33980, #25881, #34827 ) ;
#1460 = CARTESIAN_POINT ( 'NONE',  ( -34.50000000000000000, -113.0140978167138712, -0.4685323525984296800 ) ) ;
#1461 = DIRECTION ( 'NONE',  ( 0.000000000000000000, 0.000000000000000000, 1.000000000000000000 ) ) ;
#1462 = CARTESIAN_POINT ( 'NONE',  ( -38.37230871539094323, -112.5438815906447729, 6.941024454178449155 ) ) ;
#1463 = ORIENTED_EDGE ( 'NONE', *, *, #1964, .T. ) ;
#1464 = CARTESIAN_POINT ( 'NONE',  ( -38.99999999999999289, -113.9407375970686900, 6.753524454178448266 ) ) ;
#1465 = CIRCLE ( 'NONE', #25055, 7.800000000000051337 ) ;
#1466 = CARTESIAN_POINT ( 'NONE',  ( 0.000000000000000000, 44.25018368420781911, -27.31155879685134735 ) ) ;
#1467 = CARTESIAN_POINT ( 'NONE',  ( -35.50000000000000711, -112.9813730236132585, -1.624774171495860786 ) ) ;
#1468 = ORIENTED_EDGE ( 'NONE', *, *, #7214, .F. ) ;
#1469 = ORIENTED_EDGE ( 'NONE', *, *, #628, .F. ) ;
#1470 = CARTESIAN_POINT ( 'NONE',  ( -42.49999999999999289, -39.98076211353324538, 86.49999999999991473 ) ) ;
#1471 = CARTESIAN_POINT ( 'NONE',  ( 7.999999999999992895, -42.41764978026593269, -20.20639853260333751 ) ) ;
#1472 = ORIENTED_EDGE ( 'NONE', *, *, #16597, .F. ) ;
#1473 = ORIENTED_EDGE ( 'NONE', *, *, #27539, .T. ) ;
#1474 = CARTESIAN_POINT ( 'NONE',  ( -34.50000000000000000, -112.0460568841087223, -0.8839717462762063382 ) ) ;
#1475 = DIRECTION ( 'NONE',  ( 0.000000000000000000, 0.000000000000000000, 1.000000000000000000 ) ) ;
#1476 = CIRCLE ( 'NONE', #12397, 8.000000000000007105 ) ;
#1477 = DIRECTION ( 'NONE',  ( 0.000000000000000000, 0.000000000000000000, 1.000000000000000000 ) ) ;
#1478 = ORIENTED_EDGE ( 'NONE', *, *, #22705, .T. ) ;
#1479 = ORIENTED_EDGE ( 'NONE', *, *, #4647, .F. ) ;
#1480 = DIRECTION ( 'NONE',  ( 0.000000000000000000, 0.000000000000000000, -1.000000000000000000 ) ) ;
#1481 = VECTOR ( 'NONE', #20731, 1000.000000000000114 ) ;
#1482 = AXIS2_PLACEMENT_3D ( 'NONE', #27649, #8181, #32491 ) ;
#1483 = AXIS2_PLACEMENT_3D ( 'NONE', #27788, #939, #24901 ) ;
#1484 = CARTESIAN_POINT ( 'NONE',  ( -35.69272627125608466, -113.9929510916434339, 13.01835785830562209 ) ) ;
#1485 = DIRECTION ( 'NONE',  ( -1.000000000000000000, 0.000000000000000000, 0.000000000000000000 ) ) ;
#1486 = CARTESIAN_POINT ( 'NONE',  ( -36.01562499999997158, -113.9929510916434339, 13.11852480586264846 ) ) ;
#1487 = CARTESIAN_POINT ( 'NONE',  ( -35.50000000000000000, -115.9929510916434481, 10.55026311463432087 ) ) ;
#1488 = CIRCLE ( 'NONE', #20450, 8.000000000000001776 ) ;
#1489 = DIRECTION ( 'NONE',  ( -1.000000000000000000, 0.000000000000000000, 0.000000000000000000 ) ) ;
#1490 = CARTESIAN_POINT ( 'NONE',  ( 8.000000000000000000, 17.47118961583601759, 0.9861715913088272556 ) ) ;
#1491 = EDGE_CURVE ( 'NONE', #24853, #25123, #7740, .T. ) ;
#1492 = ORIENTED_EDGE ( 'NONE', *, *, #25065, .F. ) ;
#1493 = PLANE ( 'NONE',  #24055 ) ;
#1494 = CARTESIAN_POINT ( 'NONE',  ( -34.49999999999998579, 0.4463568765849662556, 113.0433323525902125 ) ) ;
#1495 = CARTESIAN_POINT ( 'NONE',  ( 55.00000000000000000, 0.000000000000000000, 0.000000000000000000 ) ) ;
#1496 = ORIENTED_EDGE ( 'NONE', *, *, #16220, .F. ) ;
#1497 = DIRECTION ( 'NONE',  ( 0.000000000000000000, 0.000000000000000000, 1.000000000000000000 ) ) ;
#1498 = CIRCLE ( 'NONE', #11263, 20.00000000000000355 ) ;
#1499 = CARTESIAN_POINT ( 'NONE',  ( -35.50000000000000711, -112.0140978167138712, 0.7502176474015694874 ) ) ;
#1500 = DIRECTION ( 'NONE',  ( -1.000000000000000000, 0.000000000000000000, 0.000000000000000000 ) ) ;
#1501 = ITEM_DEFINED_TRANSFORMATION ( 'NONE', 'NONE', #5810,  #21307 ) ;
#1502 = EDGE_CURVE ( 'NONE', #1815, #16380, #2008, .T. ) ;
#1503 = FACE_OUTER_BOUND ( 'NONE', #12935, .T. ) ;
#1504 = DIRECTION ( 'NONE',  ( 0.000000000000000000, 0.3420201433256629953, 0.9396926207859104263 ) ) ;
#1505 = MECHANICAL_DESIGN_GEOMETRIC_PRESENTATION_REPRESENTATION (  '', ( #15878 ), #35441 ) ;
#1506 = AXIS2_PLACEMENT_3D ( 'NONE', #11333, #10980, #8612 ) ;
#1507 = ORIENTED_EDGE ( 'NONE', *, *, #19965, .F. ) ;
#1508 = VECTOR ( 'NONE', #30904, 1000.000000000000000 ) ;
#1509 = CARTESIAN_POINT ( 'NONE',  ( 7.999999999999992895, 8.053585752062575764, -46.81126742072014224 ) ) ;
#1510 = CARTESIAN_POINT ( 'NONE',  ( -34.50000000000000000, -115.0631849411758196, -2.624765990393648885 ) ) ;
#1511 = LINE ( 'NONE', #12493, #7664 ) ;
#1512 = ORIENTED_EDGE ( 'NONE', *, *, #33057, .T. ) ;
#1513 = ORIENTED_EDGE ( 'NONE', *, *, #21110, .T. ) ;
#1514 = CARTESIAN_POINT ( 'NONE',  ( -38.02454729103295961, -113.6450488405582462, 9.340225545821551734 ) ) ;
#1515 = CIRCLE ( 'NONE', #9556, 47.49900000000001654 ) ;
#1516 = AXIS2_PLACEMENT_3D ( 'NONE', #30895, #33779, #6052 ) ;
#1517 = EDGE_LOOP ( 'NONE', ( #11963, #9808, #14744, #20075 ) ) ;
#1518 = ORIENTED_EDGE ( 'NONE', *, *, #22975, .F. ) ;
#1519 = CARTESIAN_POINT ( 'NONE',  ( -35.50000000000000000, -114.9932644833805426, -0.6247823525982824089 ) ) ;
#1520 = CARTESIAN_POINT ( 'NONE',  ( 8.000000000000000000, 0.000000000000000000, 0.000000000000000000 ) ) ;
#1521 = EDGE_CURVE ( 'NONE', #16008, #21028, #32422, .T. ) ;
#1522 = DIRECTION ( 'NONE',  ( 1.000000000000000000, -5.339440136655842133E-16, -1.047965281155519420E-16 ) ) ;
#1523 = AXIS2_PLACEMENT_3D ( 'NONE', #1094, #7014, #25409 ) ;
#1524 = VECTOR ( 'NONE', #11116, 1000.000000000000000 ) ;
#1525 = CARTESIAN_POINT ( 'NONE',  ( -35.93473953453761283, -114.9929510916434339, 13.11451721564123574 ) ) ;
#1526 = LINE ( 'NONE', #15540, #12639 ) ;
#1527 = CARTESIAN_POINT ( 'NONE',  ( -34.50000306791346816, -114.9929510916434339, 12.62875129555796150 ) ) ;
#1528 = LINE ( 'NONE', #4424, #20843 ) ;
#1529 = VECTOR ( 'NONE', #28337, 1000.000000000000000 ) ;
#1530 = ADVANCED_FACE ( 'NONE', ( #4718, #7566 ), #29903, .F. ) ;
#1531 = ADVANCED_FACE ( 'NONE', ( #24672 ), #24146, .T. ) ;
#1532 = CIRCLE ( 'NONE', #14752, 8.000000000000000000 ) ;
#1533 = DIRECTION ( 'NONE',  ( 0.000000000000000000, -0.3090169943749350723, -0.9510565162951576390 ) ) ;
#1534 = ORIENTED_EDGE ( 'NONE', *, *, #24682, .F. ) ;
#1535 = CARTESIAN_POINT ( 'NONE',  ( -35.50000102263781798, -115.9929510916434481, 12.62466071271731494 ) ) ;
#1536 = CARTESIAN_POINT ( 'NONE',  ( -35.50000000000000711, -116.0141056290913610, -0.5935324770972248976 ) ) ;
#1537 = FACE_OUTER_BOUND ( 'NONE', #4, .T. ) ;
#1538 = CIRCLE ( 'NONE', #6137, 4.800000000000002487 ) ;
#1539 = DIRECTION ( 'NONE',  ( 0.000000000000000000, 0.000000000000000000, -1.000000000000000000 ) ) ;
#1540 = PLANE ( 'NONE',  #18233 ) ;
#1541 = VECTOR ( 'NONE', #2445, 1000.000000000000000 ) ;
#1542 = CYLINDRICAL_SURFACE ( 'NONE', #10178, 7.199999999999994849 ) ;
#1543 = CARTESIAN_POINT ( 'NONE',  ( -9.999999999999994671, 0.000000000000000000, 0.000000000000000000 ) ) ;
#1544 = CYLINDRICAL_SURFACE ( 'NONE', #27428, 4.000000000000003553 ) ;
#1545 = DIRECTION ( 'NONE',  ( -1.783119874454246424E-31, -1.187911941725854497E-31, 1.000000000000000000 ) ) ;
#1546 = VERTEX_POINT ( 'NONE', #35138 ) ;
#1547 = EDGE_CURVE ( 'NONE', #8636, #2129, #21952, .T. ) ;
#1548 = CARTESIAN_POINT ( 'NONE',  ( -37.97545270896702618, -114.4734759653044023, 7.652725545821552622 ) ) ;
#1549 = LINE ( 'NONE', #34863, #34826 ) ;
#1550 = DIRECTION ( 'NONE',  ( 0.000000000000000000, 1.000000000000000000, 0.000000000000000000 ) ) ;
#1551 = EDGE_CURVE ( 'NONE', #20125, #33416, #27029, .T. ) ;
#1552 = VERTEX_POINT ( 'NONE', #10286 ) ;
#1553 = VECTOR ( 'NONE', #30936, 1000.000000000000000 ) ;
#1554 = ORIENTED_EDGE ( 'NONE', *, *, #29760, .F. ) ;
#1555 = CARTESIAN_POINT ( 'NONE',  ( 9.714451465470119729E-14, 0.9999999999999870104, -52.50000000000000000 ) ) ;
#1556 = AXIS2_PLACEMENT_3D ( 'NONE', #27267, #2609, #13056 ) ;
#1557 = DIRECTION ( 'NONE',  ( 1.000000000000000000, -0.000000000000000000, 0.000000000000000000 ) ) ;
#1558 = ORIENTED_EDGE ( 'NONE', *, *, #20914, .F. ) ;
#1559 = CARTESIAN_POINT ( 'NONE',  ( -35.54388159064475872, -115.3723087153909432, 2.683975545821551290 ) ) ;
#1560 = EDGE_LOOP ( 'NONE', ( #24461, #30077, #34040, #21604 ) ) ;
#1561 = AXIS2_PLACEMENT_3D ( 'NONE', #12165, #14670, #23140 ) ;
#1562 = EDGE_LOOP ( 'NONE', ( #27042, #2895, #16503, #4140 ) ) ;
#1563 = AXIS2_PLACEMENT_3D ( 'NONE', #7966, #2244, #21462 ) ;
#1564 = CYLINDRICAL_SURFACE ( 'NONE', #18869, 8.000000000000000000 ) ;
#1565 = AXIS2_PLACEMENT_3D ( 'NONE', #15918, #5489, #29982 ) ;
#1566 = DIRECTION ( 'NONE',  ( 0.000000000000000000, 0.000000000000000000, -1.000000000000000000 ) ) ;
#1567 = VECTOR ( 'NONE', #22266, 1000.000000000000000 ) ;
#1568 = CIRCLE ( 'NONE', #21677, 20.00000000000000711 ) ;
#1569 = ADVANCED_FACE ( 'NONE', ( #13342 ), #24323, .T. ) ;
#1570 = CARTESIAN_POINT ( 'NONE',  ( 3.799999999999999822, 0.000000000000000000, -43.60000000000000142 ) ) ;
#1571 = EDGE_LOOP ( 'NONE', ( #504, #10423, #21814, #16519 ) ) ;
#1572 = ORIENTED_EDGE ( 'NONE', *, *, #10998, .F. ) ;
#1573 = CARTESIAN_POINT ( 'NONE',  ( 70.00001200000002655, -29.87665282020647695, 83.95300846256282057 ) ) ;
#1574 = LINE ( 'NONE', #12367, #20622 ) ;
#1575 = ORIENTED_EDGE ( 'NONE', *, *, #17609, .T. ) ;
#1576 = DIRECTION ( 'NONE',  ( -1.000000000000000000, -0.000000000000000000, -0.000000000000000000 ) ) ;
#1577 = AXIS2_PLACEMENT_3D ( 'NONE', #7509, #1763, #18490 ) ;
#1578 = CARTESIAN_POINT ( 'NONE',  ( -34.49999999999998579, -25.98076211353322051, 84.99999999999992895 ) ) ;
#1579 = DIRECTION ( 'NONE',  ( 0.000000000000000000, 0.9822872507286879440, 0.1873813145857286533 ) ) ;
#1580 = CARTESIAN_POINT ( 'NONE',  ( -34.50000000000000000, -115.9929510916434481, 12.59102132592610346 ) ) ;
#1581 = CIRCLE ( 'NONE', #34352, 3.999999999999996447 ) ;
#1582 = EDGE_CURVE ( 'NONE', #13818, #6950, #20310, .T. ) ;
#1583 = EDGE_CURVE ( 'NONE', #5158, #6999, #31846, .T. ) ;
#1584 = FACE_OUTER_BOUND ( 'NONE', #20540, .T. ) ;
#1585 = CARTESIAN_POINT ( 'NONE',  ( -36.94073759706868287, -112.0000000000000142, 2.628524454178448710 ) ) ;
#1586 = ADVANCED_FACE ( 'NONE', ( #16721, #16553 ), #14543, .T. ) ;
#1587 = CARTESIAN_POINT ( 'NONE',  ( -34.50000000000000000, -115.9929510916434481, 12.44250253426871033 ) ) ;
#1588 = LINE ( 'NONE', #23359, #27447 ) ;
#1589 = VECTOR ( 'NONE', #10467, 1000.000000000000000 ) ;
#1590 = DIRECTION ( 'NONE',  ( 0.000000000000000000, 0.000000000000000000, 1.000000000000000000 ) ) ;
#1591 = AXIS2_PLACEMENT_3D ( 'NONE', #9571, #1658, #14789 ) ;
#1592 = LINE ( 'NONE', #20641, #29686 ) ;
#1593 = CARTESIAN_POINT ( 'NONE',  ( -9.999999999999994671, 0.000000000000000000, 0.000000000000000000 ) ) ;
#1594 = DIRECTION ( 'NONE',  ( 8.708451184622495809E-17, -6.938893903907203726E-17, -1.000000000000000000 ) ) ;
#1595 = LINE ( 'NONE', #29140, #15472 ) ;
#1596 = ORIENTED_EDGE ( 'NONE', *, *, #33710, .T. ) ;
#1597 = CARTESIAN_POINT ( 'NONE',  ( -35.81662171581203324, -110.9754527089670546, 6.715225545821551734 ) ) ;
#1598 = CIRCLE ( 'NONE', #24017, 0.7500000000000039968 ) ;
#1599 = DIRECTION ( 'NONE',  ( 0.000000000000000000, -0.4817536741017222623, 0.8763066800438598092 ) ) ;
#1600 = CARTESIAN_POINT ( 'NONE',  ( -35.50000000000000000, -113.0140978167139991, 0.8752176474014555785 ) ) ;
#1601 = EDGE_CURVE ( 'NONE', #2400, #19047, #7682, .T. ) ;
#1602 = ORIENTED_EDGE ( 'NONE', *, *, #31055, .T. ) ;
#1603 = VERTEX_POINT ( 'NONE', #14378 ) ;
#1604 = DIRECTION ( 'NONE',  ( -1.000000000000000000, 1.110223024625156540E-16, 0.000000000000000000 ) ) ;
#1605 = VERTEX_POINT ( 'NONE', #22130 ) ;
#1606 = ORIENTED_EDGE ( 'NONE', *, *, #30212, .F. ) ;
#1607 = ORIENTED_EDGE ( 'NONE', *, *, #400, .T. ) ;
#1608 = VECTOR ( 'NONE', #26480, 1000.000000000000000 ) ;
#1609 = CARTESIAN_POINT ( 'NONE',  ( 0.000000000000000000, 0.000000000000000000, 0.000000000000000000 ) ) ;
#1610 = CYLINDRICAL_SURFACE ( 'NONE', #19412, 12.55910585664918422 ) ;
#1611 = TOROIDAL_SURFACE ( 'NONE', #5092, 4.499999999999990230, 3.000000000000000000 ) ;
#1612 = AXIS2_PLACEMENT_3D ( 'NONE', #34734, #34923, #10247 ) ;
#1613 = CARTESIAN_POINT ( 'NONE',  ( 0.000000000000000000, 0.000000000000000000, 0.000000000000000000 ) ) ;
#1614 = EDGE_CURVE ( 'NONE', #4202, #2870, #28977, .T. ) ;
#1615 = CARTESIAN_POINT ( 'NONE',  ( 0.000000000000000000, -2.710505431213761085E-17, 45.00000000000000000 ) ) ;
#1616 = VERTEX_POINT ( 'NONE', #9158 ) ;
#1617 = VERTEX_POINT ( 'NONE', #25384 ) ;
#1618 = CARTESIAN_POINT ( 'NONE',  ( -35.50000000000000000, -114.8474311500471572, -2.624782352598442614 ) ) ;
#1619 = AXIS2_PLACEMENT_3D ( 'NONE', #24813, #19725, #5552 ) ;
#1620 = EDGE_CURVE ( 'NONE', #12194, #27370, #6107, .T. ) ;
#1621 = DIRECTION ( 'NONE',  ( -1.000000000000000000, 0.000000000000000000, 0.000000000000000000 ) ) ;
#1622 = LINE ( 'NONE', #12601, #30461 ) ;
#1623 = ORIENTED_EDGE ( 'NONE', *, *, #17089, .F. ) ;
#1624 = CARTESIAN_POINT ( 'NONE',  ( -37.97447287825094975, -114.9929510916434339, 12.77960891308616809 ) ) ;
#1625 = CARTESIAN_POINT ( 'NONE',  ( -34.50000000000000000, -114.9929510916434339, 10.61627146648203812 ) ) ;
#1626 = DIRECTION ( 'NONE',  ( -1.000000000000000000, 0.000000000000000000, -0.000000000000000000 ) ) ;
#1627 = ADVANCED_FACE ( 'NONE', ( #16893 ), #33129, .T. ) ;
#1628 = CARTESIAN_POINT ( 'NONE',  ( -36.15625000000007816, -114.9929510916434339, 13.11852480586264669 ) ) ;
#1629 = CARTESIAN_POINT ( 'NONE',  ( 39.30000000000000426, 7.219292880973646134E-15, 0.000000000000000000 ) ) ;
#1630 = EDGE_CURVE ( 'NONE', #13647, #34789, #11717, .T. ) ;
#1631 = CARTESIAN_POINT ( 'NONE',  ( -34.50000000000000000, -114.2598117360253696, 9.542047897280109936 ) ) ;
#1632 = FACE_OUTER_BOUND ( 'NONE', #3397, .T. ) ;
#1633 = LINE ( 'NONE', #15813, #6328 ) ;
#1634 = LINE ( 'NONE', #31862, #22234 ) ;
#1635 = VERTEX_POINT ( 'NONE', #13861 ) ;
#1636 = DIRECTION ( 'NONE',  ( 0.000000000000000000, 0.000000000000000000, -1.000000000000000000 ) ) ;
#1637 = DIRECTION ( 'NONE',  ( 0.000000000000000000, 0.000000000000000000, 1.000000000000000000 ) ) ;
#1638 = ORIENTED_EDGE ( 'NONE', *, *, #29883, .T. ) ;
#1639 = CARTESIAN_POINT ( 'NONE',  ( -35.50100302244946704, -114.9929510916434339, 12.65121853911337269 ) ) ;
#1640 = VERTEX_POINT ( 'NONE', #17075 ) ;
#1641 = CIRCLE ( 'NONE', #34441, 7.199999999999995737 ) ;
#1642 = CARTESIAN_POINT ( 'NONE',  ( -39.02454729103295961, -114.7691647218148745, 2.159774454178448710 ) ) ;
#1643 = AXIS2_PLACEMENT_3D ( 'NONE', #35597, #17003, #14133 ) ;
#1644 = CARTESIAN_POINT ( 'NONE',  ( -3.799999999999999822, 4.653657836759942730E-16, 49.10000000000000142 ) ) ;
#1645 = VERTEX_POINT ( 'NONE', #27562 ) ;
#1646 = CARTESIAN_POINT ( 'NONE',  ( -46.00000000000000000, -25.98076211353320275, 92.99999999999991473 ) ) ;
#1647 = ORIENTED_EDGE ( 'NONE', *, *, #13808, .T. ) ;
#1648 = CARTESIAN_POINT ( 'NONE',  ( -34.50000000000000000, -113.0140978167138996, -0.6247823525984306237 ) ) ;
#1649 = DIRECTION ( 'NONE',  ( -1.000000000000000000, 0.000000000000000000, 0.000000000000000000 ) ) ;
#1650 = CARTESIAN_POINT ( 'NONE',  ( -36.94073759706868287, -112.0000000000000142, 7.128524454178449155 ) ) ;
#1651 = ORIENTED_EDGE ( 'NONE', *, *, #19402, .T. ) ;
#1652 = AXIS2_PLACEMENT_3D ( 'NONE', #17026, #25693, #30390 ) ;
#1653 = CARTESIAN_POINT ( 'NONE',  ( -34.00000000000000000, -114.0592624029313242, 3.003524454178448710 ) ) ;
#1654 = CARTESIAN_POINT ( 'NONE',  ( 55.00000000000000000, 0.000000000000000000, 64.00000000000000000 ) ) ;
#1655 = CARTESIAN_POINT ( 'NONE',  ( -35.50000000000000711, -112.2144317118258527, -1.239329810084414341 ) ) ;
#1656 = VERTEX_POINT ( 'NONE', #24846 ) ;
#1657 = VERTEX_POINT ( 'NONE', #8794 ) ;
#1658 = DIRECTION ( 'NONE',  ( -1.000000000000000000, -0.000000000000000000, 0.000000000000000000 ) ) ;
#1659 = EDGE_CURVE ( 'NONE', #8935, #35010, #12896, .T. ) ;
#1660 = CARTESIAN_POINT ( 'NONE',  ( 7.999999999999992895, -42.41764978026593269, -20.20639853260333751 ) ) ;
#1661 = ORIENTED_EDGE ( 'NONE', *, *, #9630, .T. ) ;
#1662 = ORIENTED_EDGE ( 'NONE', *, *, #15007, .F. ) ;
#1663 = CARTESIAN_POINT ( 'NONE',  ( -34.50000000000000000, -115.8137639216009234, -1.239329810084483841 ) ) ;
#1664 = DIRECTION ( 'NONE',  ( 1.000000000000000000, -5.339440136655842133E-16, -1.047965281155519420E-16 ) ) ;
#1665 = EDGE_CURVE ( 'NONE', #29583, #1876, #28085, .T. ) ;
#1666 = AXIS2_PLACEMENT_3D ( 'NONE', #8199, #16112, #18830 ) ;
#1667 = DIRECTION ( 'NONE',  ( 1.000000000000000000, -5.339440136655842133E-16, -1.047965281155519420E-16 ) ) ;
#1668 = EDGE_LOOP ( 'NONE', ( #2169, #17743, #21622, #22182 ) ) ;
#1669 = ORIENTED_EDGE ( 'NONE', *, *, #12636, .T. ) ;
#1670 = LINE ( 'NONE', #12654, #13772 ) ;
#1671 = VECTOR ( 'NONE', #9095, 1000.000000000000000 ) ;
#1672 = AXIS2_PLACEMENT_3D ( 'NONE', #9437, #12867, #15717 ) ;
#1673 = CARTESIAN_POINT ( 'NONE',  ( -34.50000000000000000, -113.9000545103886850, 10.49516883415891577 ) ) ;
#1674 = LINE ( 'NONE', #15504, #30118 ) ;
#1675 = CARTESIAN_POINT ( 'NONE',  ( -35.50000000000000000, -113.9929510916434339, 12.44250253426871033 ) ) ;
#1676 = CARTESIAN_POINT ( 'NONE',  ( -37.53269373325071712, -115.9929510916434481, 13.11752178341324360 ) ) ;
#1677 = CARTESIAN_POINT ( 'NONE',  ( -1.520000000000000018, -3.261632136597012339E-16, -5.016000000000010672 ) ) ;
#1678 = LINE ( 'NONE', #29755, #10646 ) ;
#1679 = ORIENTED_EDGE ( 'NONE', *, *, #12599, .T. ) ;
#1680 = CARTESIAN_POINT ( 'NONE',  ( 0.000000000000000000, 0.000000000000000000, -44.50000000000000000 ) ) ;
#1681 = DIRECTION ( 'NONE',  ( 0.000000000000000000, 0.000000000000000000, 1.000000000000000000 ) ) ;
#1682 = CARTESIAN_POINT ( 'NONE',  ( -36.99999999999999289, -6.699660887819688604, 116.5112005972652014 ) ) ;
#1683 = ORIENTED_EDGE ( 'NONE', *, *, #29106, .F. ) ;
#1684 = DIRECTION ( 'NONE',  ( 0.000000000000000000, 0.000000000000000000, -1.000000000000000000 ) ) ;
#1685 = CARTESIAN_POINT ( 'NONE',  ( -35.50000000000000711, -112.6605569508015350, 1.812590711673265575 ) ) ;
#1686 = FACE_OUTER_BOUND ( 'NONE', #17486, .T. ) ;
#1687 = AXIS2_PLACEMENT_3D ( 'NONE', #17179, #11265, #28357 ) ;
#1688 = DIRECTION ( 'NONE',  ( 0.000000000000000000, -0.8660254037844329345, -0.5000000000000101030 ) ) ;
#1689 = DIRECTION ( 'NONE',  ( -1.000000000000000000, 0.000000000000000000, 0.000000000000000000 ) ) ;
#1690 = CARTESIAN_POINT ( 'NONE',  ( 8.000000000000000000, 16.94522934049224361, -8.128228055638670568 ) ) ;
#1691 = ORIENTED_EDGE ( 'NONE', *, *, #21387, .T. ) ;
#1692 = CIRCLE ( 'NONE', #1126, 4.000000000000000000 ) ;
#1693 = FACE_OUTER_BOUND ( 'NONE', #25240, .T. ) ;
#1694 = CARTESIAN_POINT ( 'NONE',  ( -34.50000000000000000, -116.0215255531121983, -2.372276521655488857 ) ) ;
#1695 = DIRECTION ( 'NONE',  ( -1.000000000000000000, 0.000000000000000000, 0.000000000000000000 ) ) ;
#1696 = EDGE_LOOP ( 'NONE', ( #7796, #14510 ) ) ;
#1697 = ORIENTED_EDGE ( 'NONE', *, *, #13227, .F. ) ;
#1698 = CARTESIAN_POINT ( 'NONE',  ( -37.66520193420439000, -113.2509883718312977, 3.941024454178448710 ) ) ;
#1699 = VECTOR ( 'NONE', #25053, 1000.000000000000000 ) ;
#1700 = ORIENTED_EDGE ( 'NONE', *, *, #28806, .F. ) ;
#1701 = ORIENTED_EDGE ( 'NONE', *, *, #25097, .F. ) ;
#1702 = CARTESIAN_POINT ( 'NONE',  ( -35.50000000000000000, -115.0140978167139707, -0.6091573525984161908 ) ) ;
#1703 = EDGE_CURVE ( 'NONE', #33387, #8613, #31283, .T. ) ;
#1704 = CARTESIAN_POINT ( 'NONE',  ( -2.000000000000001776, 0.000000000000000000, 0.000000000000000000 ) ) ;
#1705 = DIRECTION ( 'NONE',  ( 0.000000000000000000, -0.8660254037844431485, 0.4999999999999921174 ) ) ;
#1706 = CARTESIAN_POINT ( 'NONE',  ( -37.93687354226506869, -114.9929510916434339, 12.87038173996323565 ) ) ;
#1707 = DIRECTION ( 'NONE',  ( 0.000000000000000000, 0.5877852522924738032, -0.8090169943749468962 ) ) ;
#1708 = EDGE_CURVE ( 'NONE', #10690, #33549, #14030, .T. ) ;
#1709 = CARTESIAN_POINT ( 'NONE',  ( -37.54906985245724371, -114.9929510916434339, 14.11777216781844579 ) ) ;
#1710 = FACE_OUTER_BOUND ( 'NONE', #26903, .T. ) ;
#1711 = CIRCLE ( 'NONE', #21825, 2.799122904894268071 ) ;
#1712 = DIRECTION ( 'NONE',  ( -1.000000000000000000, 0.000000000000000000, 0.000000000000000000 ) ) ;
#1713 = ORIENTED_EDGE ( 'NONE', *, *, #14111, .F. ) ;
#1714 = AXIS2_PLACEMENT_3D ( 'NONE', #11283, #19375, #10758 ) ;
#1715 = CARTESIAN_POINT ( 'NONE',  ( -1.799999999999996048, 0.000000000000000000, 0.000000000000000000 ) ) ;
#1716 = CARTESIAN_POINT ( 'NONE',  ( -35.98364338251434447, -115.9929510916434481, 13.11827392651456314 ) ) ;
#1717 = CARTESIAN_POINT ( 'NONE',  ( -35.50000000000000711, -116.0140978167138712, 0.8752176474015622709 ) ) ;
#1718 = DIRECTION ( 'NONE',  ( -1.047965281155519913E-16, -6.938893903907192632E-17, -1.000000000000000000 ) ) ;
#1719 = AXIS2_PLACEMENT_3D ( 'NONE', #8421, #3401, #28059 ) ;
#1720 = DIRECTION ( 'NONE',  ( -1.000000000000000000, 0.000000000000000000, 0.000000000000000000 ) ) ;
#1721 = DIRECTION ( 'NONE',  ( -1.000000000000000000, -1.734723475976807094E-16, -0.000000000000000000 ) ) ;
#1722 = ORIENTED_EDGE ( 'NONE', *, *, #30631, .F. ) ;
#1723 = CARTESIAN_POINT ( 'NONE',  ( -34.49999999999998579, -29.98076211353321341, 84.99999999999994316 ) ) ;
#1724 = DIRECTION ( 'NONE',  ( -1.836970198721029934E-16, 1.000000000000000000, 0.000000000000000000 ) ) ;
#1725 = CARTESIAN_POINT ( 'NONE',  ( 7.999999999999992895, 0.000000000000000000, 0.000000000000000000 ) ) ;
#1726 = PLANE ( 'NONE',  #34542 ) ;
#1727 = ORIENTED_EDGE ( 'NONE', *, *, #3412, .F. ) ;
#1728 = CARTESIAN_POINT ( 'NONE',  ( -37.05926240293133134, -115.0000000000000000, 6.378524454178448266 ) ) ;
#1729 = DIRECTION ( 'NONE',  ( 0.000000000000000000, 0.000000000000000000, -1.000000000000000000 ) ) ;
#1730 = CARTESIAN_POINT ( 'NONE',  ( 50.00000000000000000, 20.00000000000001776, 120.0000000000000000 ) ) ;
#1731 = ORIENTED_EDGE ( 'NONE', *, *, #25116, .T. ) ;
#1732 = VERTEX_POINT ( 'NONE', #11857 ) ;
#1733 =( LENGTH_UNIT ( ) NAMED_UNIT ( * ) SI_UNIT ( .MILLI., .METRE. ) );
#1734 = CARTESIAN_POINT ( 'NONE',  ( -10.00000000000000178, 0.000000000000000000, 0.000000000000000000 ) ) ;
#1735 = EDGE_LOOP ( 'NONE', ( #29650, #4168, #5761, #15446 ) ) ;
#1736 = CIRCLE ( 'NONE', #13264, 19.99999999999998579 ) ;
#1737 = CARTESIAN_POINT ( 'NONE',  ( -38.37230871539094323, -115.4561184093552413, 3.058975545821551290 ) ) ;
#1738 = ORIENTED_EDGE ( 'NONE', *, *, #29262, .T. ) ;
#1739 =( NAMED_UNIT ( * ) PLANE_ANGLE_UNIT ( ) SI_UNIT ( $, .RADIAN. ) );
#1740 = ORIENTED_EDGE ( 'NONE', *, *, #5999, .T. ) ;
#1741 = AXIS2_PLACEMENT_3D ( 'NONE', #11264, #14475, #33059 ) ;
#1742 = VERTEX_POINT ( 'NONE', #19437 ) ;
#1743 = CARTESIAN_POINT ( 'NONE',  ( -46.00000000000000000, 0.000000000000000000, 0.000000000000000000 ) ) ;
#1744 = EDGE_CURVE ( 'NONE', #4405, #6685, #15744, .T. ) ;
#1745 = EDGE_CURVE ( 'NONE', #7407, #24192, #5764, .T. ) ;
#1746 = FACE_OUTER_BOUND ( 'NONE', #7968, .T. ) ;
#1747 = CIRCLE ( 'NONE', #6335, 14.00000000000000000 ) ;
#1748 = CYLINDRICAL_SURFACE ( 'NONE', #21362, 9.499000000000000554 ) ;
#1749 = EDGE_LOOP ( 'NONE', ( #26063, #16857, #20128, #5547 ) ) ;
#1750 = ORIENTED_EDGE ( 'NONE', *, *, #12552, .T. ) ;
#1751 = CARTESIAN_POINT ( 'NONE',  ( 8.000000000000000000, 3.384281271887823461, 18.48663108841358138 ) ) ;
#1752 = PLANE ( 'NONE',  #4563 ) ;
#1753 = EDGE_CURVE ( 'NONE', #16353, #3289, #16331, .T. ) ;
#1754 = EDGE_LOOP ( 'NONE', ( #33184, #22637, #28342, #32874 ) ) ;
#1755 = DIRECTION ( 'NONE',  ( 0.000000000000000000, 0.3090169943749412895, 0.9510565162951555296 ) ) ;
#1756 = CARTESIAN_POINT ( 'NONE',  ( -34.49999999999998579, -5.633167542791597704, 143.9590043477703887 ) ) ;
#1757 = DIRECTION ( 'NONE',  ( -1.000000000000000000, 0.000000000000000000, 0.000000000000000000 ) ) ;
#1758 = CARTESIAN_POINT ( 'NONE',  ( -36.03125000000003553, -115.9929510916434481, 14.11852480586265024 ) ) ;
#1759 = CIRCLE ( 'NONE', #33, 47.49900000000001654 ) ;
#1760 = CARTESIAN_POINT ( 'NONE',  ( 55.00000000000000711, -26.94801722181409431, 85.25380613764163229 ) ) ;
#1761 = CARTESIAN_POINT ( 'NONE',  ( -35.00000000000000000, -114.0592624029313242, 7.503524454178449155 ) ) ;
#1762 = CARTESIAN_POINT ( 'NONE',  ( -34.50000000000000000, -115.9929510916434481, 12.17846912687782712 ) ) ;
#1763 = DIRECTION ( 'NONE',  ( 0.000000000000000000, 0.000000000000000000, -1.000000000000000000 ) ) ;
#1764 = CARTESIAN_POINT ( 'NONE',  ( 7.999999999999992895, 19.44205635905542451, 43.33776004284616334 ) ) ;
#1765 = VECTOR ( 'NONE', #7342, 1000.000000000000000 ) ;
#1766 = ADVANCED_BREP_SHAPE_REPRESENTATION ( '', ( #34287, #21307 ), #1229 ) ;
#1767 = LINE ( 'NONE', #20817, #16991 ) ;
#1768 = CARTESIAN_POINT ( 'NONE',  ( 7.999999999999992895, 24.47917365149947244, 45.87777302070943364 ) ) ;
#1769 = FACE_OUTER_BOUND ( 'NONE', #102, .T. ) ;
#1770 = DIRECTION ( 'NONE',  ( -1.000000000000000000, 0.000000000000000000, 0.000000000000000000 ) ) ;
#1771 = ORIENTED_EDGE ( 'NONE', *, *, #20086, .T. ) ;
#1772 = VECTOR ( 'NONE', #28510, 1000.000000000000000 ) ;
#1773 = MECHANICAL_DESIGN_GEOMETRIC_PRESENTATION_REPRESENTATION (  '', ( #5255 ), #9237 ) ;
#1774 = CARTESIAN_POINT ( 'NONE',  ( -34.00000000000000000, -113.9407375970686758, 9.996475545821549957 ) ) ;
#1775 = AXIS2_PLACEMENT_3D ( 'NONE', #9392, #14792, #34435 ) ;
#1776 = LINE ( 'NONE', #17956, #13518 ) ;
#1777 = EDGE_CURVE ( 'NONE', #11644, #9824, #8275, .T. ) ;
#1778 = CARTESIAN_POINT ( 'NONE',  ( -35.50000000000000000, -113.0140978167138712, -0.4685323525984296800 ) ) ;
#1779 = VERTEX_POINT ( 'NONE', #25208 ) ;
#1780 = EDGE_LOOP ( 'NONE', ( #22222, #6075 ) ) ;
#1782 = FACE_OUTER_BOUND ( 'NONE', #25598, .T. ) ;
#1781 = PRODUCT ( 'winch drum', 'winch drum', '', ( #12191 ) ) ;
#1783 = CYLINDRICAL_SURFACE ( 'NONE', #24407, 17.49900000000000233 ) ;
#1784 = ORIENTED_EDGE ( 'NONE', *, *, #30806, .F. ) ;
#1785 = VERTEX_POINT ( 'NONE', #20655 ) ;
#1786 = ORIENTED_EDGE ( 'NONE', *, *, #16107, .T. ) ;
#1787 = EDGE_CURVE ( 'NONE', #16603, #25611, #17470, .T. ) ;
#1788 = LINE ( 'NONE', #26456, #1047 ) ;
#1789 = EDGE_CURVE ( 'NONE', #14155, #2828, #19197, .T. ) ;
#1790 = SHAPE_REPRESENTATION ( 'Toothed Ratchet Brake Disc', ( #21307 ), #24207 ) ;
#1791 = DIRECTION ( 'NONE',  ( 0.000000000000000000, 0.000000000000000000, 1.000000000000000000 ) ) ;
#1792 = ADVANCED_FACE ( 'NONE', ( #15077 ), #1243, .F. ) ;
#1793 = DIRECTION ( 'NONE',  ( -1.000000000000000000, 0.000000000000000000, 0.000000000000000000 ) ) ;
#1794 = LINE ( 'NONE', #5029, #30003 ) ;
#1795 = ORIENTED_EDGE ( 'NONE', *, *, #17528, .T. ) ;
#1796 = EDGE_LOOP ( 'NONE', ( #2648, #490, #8320, #32587 ) ) ;
#1797 = CARTESIAN_POINT ( 'NONE',  ( -35.50000000000000711, -113.0974311500471714, -1.624782352598427959 ) ) ;
#1798 = LINE ( 'NONE', #15450, #30635 ) ;
#1799 = ADVANCED_FACE ( 'NONE', ( #12041 ), #23016, .T. ) ;
#1800 = DIRECTION ( 'NONE',  ( 1.000000000000000000, -0.000000000000000000, -0.000000000000000000 ) ) ;
#1801 = CIRCLE ( 'NONE', #20164, 20.00000000000000355 ) ;
#1802 = VERTEX_POINT ( 'NONE', #20830 ) ;
#1803 = CIRCLE ( 'NONE', #34001, 4.000000000000003553 ) ;
#1804 = CARTESIAN_POINT ( 'NONE',  ( 0.000000000000000000, 0.000000000000000000, -65.00000000000000000 ) ) ;
#1805 = EDGE_CURVE ( 'NONE', #11039, #33784, #34741, .T. ) ;
#1806 = CARTESIAN_POINT ( 'NONE',  ( -34.50000000000000000, -112.1859307030124739, 1.448610958621386224 ) ) ;
#1807 = CARTESIAN_POINT ( 'NONE',  ( -34.57658136524562309, -114.9929510916434339, 13.10177712753338497 ) ) ;
#1808 = LINE ( 'NONE', #20507, #17106 ) ;
#1809 = CARTESIAN_POINT ( 'NONE',  ( -37.52044295795950291, -114.9929510916434339, 13.11812344617477244 ) ) ;
#1810 = DIRECTION ( 'NONE',  ( -1.000000000000000000, 0.000000000000000000, 0.000000000000000000 ) ) ;
#1811 = CARTESIAN_POINT ( 'NONE',  ( -34.50000000000000000, -114.4026847875275337, 9.592046023459676718 ) ) ;
#1812 = CARTESIAN_POINT ( 'NONE',  ( 4.000000000000003553, -49.65209126885753221, -15.44894276735603356 ) ) ;
#1813 = CARTESIAN_POINT ( 'NONE',  ( -38.00000000000000711, -114.9929510916434339, 10.85830208992306822 ) ) ;
#1814 = DIRECTION ( 'NONE',  ( 0.000000000000000000, 0.000000000000000000, 1.000000000000000000 ) ) ;
#1815 = VERTEX_POINT ( 'NONE', #7167 ) ;
#1816 = CARTESIAN_POINT ( 'NONE',  ( 0.000000000000000000, -2.710505431213761085E-17, 38.90000000000000568 ) ) ;
#1817 = PLANE ( 'NONE',  #32446 ) ;
#1818 = ORIENTED_EDGE ( 'NONE', *, *, #35286, .F. ) ;
#1819 = CARTESIAN_POINT ( 'NONE',  ( -37.98402046630260287, -114.9929510916434339, 12.74811950270164118 ) ) ;
#1820 = EDGE_LOOP ( 'NONE', ( #13899, #19294, #31503, #24102 ) ) ;
#1821 = VECTOR ( 'NONE', #34895, 1000.000000000000000 ) ;
#1822 = CARTESIAN_POINT ( 'NONE',  ( -39.02454729103295961, -114.7691647218148745, 3.659774454178448710 ) ) ;
#1823 = CARTESIAN_POINT ( 'NONE',  ( 0.000000000000000000, 0.000000000000000000, 0.000000000000000000 ) ) ;
#1824 = EDGE_CURVE ( 'NONE', #4708, #15928, #3696, .T. ) ;
#1825 = VERTEX_POINT ( 'NONE', #31305 ) ;
#1826 = LINE ( 'NONE', #2496, #32565 ) ;
#1827 = EDGE_LOOP ( 'NONE', ( #8246, #13023 ) ) ;
#1828 = CARTESIAN_POINT ( 'NONE',  ( -34.50000000000000000, -113.0140978167139991, 0.8752176474014555785 ) ) ;
#1829 = DIRECTION ( 'NONE',  ( 0.000000000000000000, 0.000000000000000000, -1.000000000000000000 ) ) ;
#1830 = ADVANCED_FACE ( 'NONE', ( #28788 ), #26090, .T. ) ;
#1831 = CARTESIAN_POINT ( 'NONE',  ( 0.000000000000000000, 0.000000000000000000, 0.000000000000000000 ) ) ;
#1833 = EDGE_CURVE ( 'NONE', #209, #6280, #4137, .T. ) ;
#1832 = AXIS2_PLACEMENT_3D ( 'NONE', #6498, #6856, #14948 ) ;
#1834 = ORIENTED_EDGE ( 'NONE', *, *, #23660, .T. ) ;
#1835 = AXIS2_PLACEMENT_3D ( 'NONE', #34697, #7844, #15755 ) ;
#1836 = CARTESIAN_POINT ( 'NONE',  ( -34.00000000000000000, -114.0592624029313242, 1.503524454178448710 ) ) ;
#1837 = DIRECTION ( 'NONE',  ( 0.000000000000000000, 0.9048270524660205760, -0.4257792915650703836 ) ) ;
#1838 = CARTESIAN_POINT ( 'NONE',  ( 8.000000000000000000, 2.494040418455619523, -18.62763138773847871 ) ) ;
#1839 = VERTEX_POINT ( 'NONE', #29151 ) ;
#1840 = ORIENTED_EDGE ( 'NONE', *, *, #5603, .T. ) ;
#1841 = EDGE_CURVE ( 'NONE', #2812, #27419, #31874, .T. ) ;
#1842 = CARTESIAN_POINT ( 'NONE',  ( 8.000000000000007105, -8.725776631572617958, -3.753907720749127819 ) ) ;
#1843 = EDGE_CURVE ( 'NONE', #25616, #5216, #33585, .T. ) ;
#1844 =( NAMED_UNIT ( * ) SI_UNIT ( $, .STERADIAN. ) SOLID_ANGLE_UNIT ( ) );
#1845 = FACE_OUTER_BOUND ( 'NONE', #31583, .T. ) ;
#1846 = ORIENTED_EDGE ( 'NONE', *, *, #19121, .F. ) ;
#1847 = VERTEX_POINT ( 'NONE', #9518 ) ;
#1848 = CARTESIAN_POINT ( 'NONE',  ( -34.50000000000000000, -114.8057644833805853, -2.624782352598442614 ) ) ;
#1849 = DIRECTION ( 'NONE',  ( -1.734723475976807094E-16, -1.000000000000000000, 1.067522139062650474E-15 ) ) ;
#1850 = VERTEX_POINT ( 'NONE', #26266 ) ;
#1851 = ORIENTED_EDGE ( 'NONE', *, *, #2245, .F. ) ;
#1852 = CARTESIAN_POINT ( 'NONE',  ( 0.000000000000000000, 0.000000000000000000, -39.50000000000000711 ) ) ;
#1853 = ADVANCED_FACE ( 'NONE', ( #12398 ), #34017, .T. ) ;
#1854 = CARTESIAN_POINT ( 'NONE',  ( -34.50000000000000000, -113.9929510916434339, 10.50625754673588474 ) ) ;
#1855 = DIRECTION ( 'NONE',  ( -1.000000000000000000, -0.000000000000000000, -0.000000000000000000 ) ) ;
#1856 = AXIS2_PLACEMENT_3D ( 'NONE', #29919, #7940, #2564 ) ;
#1857 = PRESENTATION_LAYER_ASSIGNMENT (  '', '', ( #18512 ) ) ;
#1858 = AXIS2_PLACEMENT_3D ( 'NONE', #20395, #33939, #9270 ) ;
#1859 = CARTESIAN_POINT ( 'NONE',  ( -38.00000000000000711, -113.9929510916434339, 12.26648026267477221 ) ) ;
#1860 = CARTESIAN_POINT ( 'NONE',  ( -36.01562499999997158, -115.9929510916434481, 13.11852480586264846 ) ) ;
#1861 = LINE ( 'NONE', #9769, #1481 ) ;
#1862 = FACE_OUTER_BOUND ( 'NONE', #34954, .T. ) ;
#1863 = ORIENTED_EDGE ( 'NONE', *, *, #11605, .F. ) ;
#1864 = LINE ( 'NONE', #23266, #22863 ) ;
#1865 = CARTESIAN_POINT ( 'NONE',  ( 4.121423858225409909, -12.61643262889541894, 0.000000000000000000 ) ) ;
#1866 = CARTESIAN_POINT ( 'NONE',  ( 0.000000000000000000, -2.710505431213761085E-17, 45.10000000000000142 ) ) ;
#1867 = EDGE_CURVE ( 'NONE', #13043, #6684, #17784, .T. ) ;
#1868 = VERTEX_POINT ( 'NONE', #25917 ) ;
#1869 = CIRCLE ( 'NONE', #16244, 4.000000000000000000 ) ;
#1870 = DIRECTION ( 'NONE',  ( -1.000000000000000000, 0.000000000000000000, 0.000000000000000000 ) ) ;
#1871 = EDGE_CURVE ( 'NONE', #26262, #6240, #25561, .T. ) ;
#1872 = CARTESIAN_POINT ( 'NONE',  ( -35.50000000000000711, -112.0154707866092707, 0.9357013553229778235 ) ) ;
#1873 = DIRECTION ( 'NONE',  ( -1.000000000000000000, 0.000000000000000000, -0.000000000000000000 ) ) ;
#1874 = DIRECTION ( 'NONE',  ( -1.000000000000000000, 0.000000000000000000, -0.000000000000000000 ) ) ;
#1875 = CARTESIAN_POINT ( 'NONE',  ( -90.00000000000002842, 0.000000000000000000, 6.938893903907228378E-15 ) ) ;
#1876 = VERTEX_POINT ( 'NONE', #34375 ) ;
#1877 = CARTESIAN_POINT ( 'NONE',  ( -90.00000000000002842, -3.455569164145799535E-16, -4.980000000000010196 ) ) ;
#1878 = CARTESIAN_POINT ( 'NONE',  ( -34.50000000000000000, -111.0173113992184710, -0.7556348869410824953 ) ) ;
#1879 = TOROIDAL_SURFACE ( 'NONE', #9930, 6.983999999999990216, 0.04100000000000673939 ) ;
#1880 = CARTESIAN_POINT ( 'NONE',  ( 4.000000000000003553, -49.65209126885775248, 15.44894276735532479 ) ) ;
#1881 = ORIENTED_EDGE ( 'NONE', *, *, #30112, .F. ) ;
#1882 = VERTEX_POINT ( 'NONE', #12759 ) ;
#1883 = ADVANCED_FACE ( 'NONE', ( #26448 ), #1783, .T. ) ;
#1884 = CARTESIAN_POINT ( 'NONE',  ( -35.02454729103298803, -114.8876895276775087, 1.597274454178448710 ) ) ;
#1885 = CIRCLE ( 'NONE', #23711, 47.49900000000003075 ) ;
#1886 = AXIS2_PLACEMENT_3D ( 'NONE', #15897, #7452, #7275 ) ;
#1887 = EDGE_CURVE ( 'NONE', #6697, #28711, #25741, .T. ) ;
#1888 =( NAMED_UNIT ( * ) PLANE_ANGLE_UNIT ( ) SI_UNIT ( $, .RADIAN. ) );
#1889 = DIRECTION ( 'NONE',  ( 0.000000000000000000, 0.000000000000000000, 1.000000000000000000 ) ) ;
#1890 = EDGE_LOOP ( 'NONE', ( #6488, #9616, #27724, #30292 ) ) ;
#1891 = ORIENTED_EDGE ( 'NONE', *, *, #27121, .F. ) ;
#1892 = CARTESIAN_POINT ( 'NONE',  ( -35.50000000000000000, -115.0140978167138712, -0.4685323525984309012 ) ) ;
#1893 = CARTESIAN_POINT ( 'NONE',  ( 4.000000000000003553, 49.65209126885784485, -15.44894276735497840 ) ) ;
#1894 = CARTESIAN_POINT ( 'NONE',  ( 0.000000000000000000, 0.000000000000000000, -55.00000000000000000 ) ) ;
#1895 = CIRCLE ( 'NONE', #19137, 52.00000000000000711 ) ;
#1896 = CARTESIAN_POINT ( 'NONE',  ( -35.50000000000000000, -113.9836614335179377, 10.50514867547815534 ) ) ;
#1897 = CARTESIAN_POINT ( 'NONE',  ( -21.15833593587365513, -17.68172400785659448, 96.37435565298210349 ) ) ;
#1898 = CARTESIAN_POINT ( 'NONE',  ( -36.31249999999995026, -114.9929510916434339, 14.11852480586264846 ) ) ;
#1899 = CARTESIAN_POINT ( 'NONE',  ( -49.99999999999998579, -64.99999999999997158, 120.0000000000000000 ) ) ;
#1900 = AXIS2_PLACEMENT_3D ( 'NONE', #29623, #32852, #8343 ) ;
#1901 = AXIS2_PLACEMENT_3D ( 'NONE', #34945, #12784, #12963 ) ;
#1902 = FACE_OUTER_BOUND ( 'NONE', #33338, .T. ) ;
#1903 = ORIENTED_EDGE ( 'NONE', *, *, #26827, .T. ) ;
#1904 = CARTESIAN_POINT ( 'NONE',  ( -35.50005019975638021, -115.9929510916434481, 12.62670525340498351 ) ) ;
#1905 = CARTESIAN_POINT ( 'NONE',  ( -35.50000000000000711, -114.8057644833805568, -1.624782352598427959 ) ) ;
#1906 = DIRECTION ( 'NONE',  ( 1.000000000000000000, -5.339440136655842133E-16, -1.047965281155519420E-16 ) ) ;
#1907 = CARTESIAN_POINT ( 'NONE',  ( -34.49999999999998579, -20.27980021920970799, 72.12564434701783966 ) ) ;
#1908 = DIRECTION ( 'NONE',  ( 1.000000000000000000, -0.000000000000000000, 0.000000000000000000 ) ) ;
#1909 = VERTEX_POINT ( 'NONE', #10590 ) ;
#1910 = CARTESIAN_POINT ( 'NONE',  ( -55.00000000000000000, 7.347880794884122694E-16, 76.00000000000001421 ) ) ;
#1911 = CARTESIAN_POINT ( 'NONE',  ( 7.999999999999992895, 0.000000000000000000, 0.000000000000000000 ) ) ;
#1912 = ADVANCED_FACE ( 'NONE', ( #1962 ), #23923, .T. ) ;
#1913 = DIRECTION ( 'NONE',  ( 0.000000000000000000, 0.000000000000000000, 1.000000000000000000 ) ) ;
#1914 = DIRECTION ( 'NONE',  ( -0.000000000000000000, 0.000000000000000000, -1.000000000000000000 ) ) ;
#1915 = ORIENTED_EDGE ( 'NONE', *, *, #20368, .T. ) ;
#1916 = CARTESIAN_POINT ( 'NONE',  ( -37.99999999999998579, -113.9407375970686758, 5.253524454178449155 ) ) ;
#1917 = CARTESIAN_POINT ( 'NONE',  ( 8.000000000000000000, 21.80633394113450052, -2.912696353505896951 ) ) ;
#1918 = LINE ( 'NONE', #4971, #30830 ) ;
#1919 = ORIENTED_EDGE ( 'NONE', *, *, #34578, .F. ) ;
#1920 = AXIS2_PLACEMENT_3D ( 'NONE', #6427, #20269, #30568 ) ;
#1921 = ORIENTED_EDGE ( 'NONE', *, *, #32147, .T. ) ;
#1922 = CARTESIAN_POINT ( 'NONE',  ( -6.938893903907228378E-15, 0.7408941433508786645, -1.200000000000006617 ) ) ;
#1923 = CARTESIAN_POINT ( 'NONE',  ( 50.00005079999999680, 0.000000000000000000, 3.999999999999996447 ) ) ;
#1924 = VERTEX_POINT ( 'NONE', #21543 ) ;
#1925 = CARTESIAN_POINT ( 'NONE',  ( -36.94073759706868287, -116.9999999999999858, 7.371475545821551734 ) ) ;
#1926 = VERTEX_POINT ( 'NONE', #2503 ) ;
#1927 = ORIENTED_EDGE ( 'NONE', *, *, #25819, .F. ) ;
#1928 = ORIENTED_EDGE ( 'NONE', *, *, #1210, .T. ) ;
#1929 = FACE_OUTER_BOUND ( 'NONE', #31203, .T. ) ;
#1930 = CIRCLE ( 'NONE', #27805, 6.765000000000044977 ) ;
#1931 = AXIS2_PLACEMENT_3D ( 'NONE', #3409, #3050, #22460 ) ;
#1932 = CIRCLE ( 'NONE', #6508, 20.00000000000000355 ) ;
#1933 = CARTESIAN_POINT ( 'NONE',  ( -3.983177536951265640, -13.66651769228263724, 0.000000000000000000 ) ) ;
#1934 = VERTEX_POINT ( 'NONE', #24451 ) ;
#1935 = VERTEX_POINT ( 'NONE', #26804 ) ;
#1936 = DIRECTION ( 'NONE',  ( 1.783119874454246424E-31, 1.187911941725854497E-31, -1.000000000000000000 ) ) ;
#1937 = DIRECTION ( 'NONE',  ( 0.000000000000000000, 0.000000000000000000, 1.000000000000000000 ) ) ;
#1938 = ORIENTED_EDGE ( 'NONE', *, *, #26880, .F. ) ;
#1939 = DIRECTION ( 'NONE',  ( -1.000000000000000000, 0.000000000000000000, 0.000000000000000000 ) ) ;
#1940 = CIRCLE ( 'NONE', #1920, 2.447112362156710574 ) ;
#1941 = CARTESIAN_POINT ( 'NONE',  ( 0.000000000000000000, 47.00885577955422434, -6.806061952191799769 ) ) ;
#1942 = CARTESIAN_POINT ( 'NONE',  ( -34.49999999999998579, -25.98076211353322051, 84.99999999999992895 ) ) ;
#1943 = CARTESIAN_POINT ( 'NONE',  ( -35.95093014754292682, -115.9929510916434481, 14.11777216781842625 ) ) ;
#1944 = LINE ( 'NONE', #4657, #30693 ) ;
#1945 = CARTESIAN_POINT ( 'NONE',  ( -39.02454729103295961, -114.7691647218148745, 8.159774454178448266 ) ) ;
#1946 = CARTESIAN_POINT ( 'NONE',  ( -34.50000000000000000, -114.8124184834118324, 8.677834500183694288 ) ) ;
#1947 = DIRECTION ( 'NONE',  ( -1.000000000000000000, -1.836970198721029934E-16, -0.000000000000000000 ) ) ;
#1948 = FACE_OUTER_BOUND ( 'NONE', #6910, .T. ) ;
#1949 = DIRECTION ( 'NONE',  ( 0.000000000000000000, 0.000000000000000000, 1.000000000000000000 ) ) ;
#1950 = DIRECTION ( 'NONE',  ( -1.000000000000000000, 0.000000000000000000, 0.000000000000000000 ) ) ;
#1951 = ADVANCED_FACE ( 'NONE', ( #32372, #32541 ), #35096, .F. ) ;
#1952 = CARTESIAN_POINT ( 'NONE',  ( 7.999999999999992895, -38.92705108641712286, -27.21837053747841395 ) ) ;
#1953 = SURFACE_STYLE_FILL_AREA ( #20820 ) ;
#1954 = VERTEX_POINT ( 'NONE', #21205 ) ;
#1955 = CARTESIAN_POINT ( 'NONE',  ( -38.37230871539094323, -115.4561184093552413, 4.558975545821550845 ) ) ;
#1956 = CARTESIAN_POINT ( 'NONE',  ( 0.000000000000000000, 19.44205635905542451, 43.33776004284616334 ) ) ;
#1957 = CARTESIAN_POINT ( 'NONE',  ( -35.50000000000000000, -113.0140978167138712, 0.6252176474015680441 ) ) ;
#1958 = ORIENTED_EDGE ( 'NONE', *, *, #17210, .T. ) ;
#1959 = ORIENTED_EDGE ( 'NONE', *, *, #3260, .F. ) ;
#1960 = AXIS2_PLACEMENT_3D ( 'NONE', #2687, #5893, #33431 ) ;
#1961 = LINE ( 'NONE', #29150, #27512 ) ;
#1962 = FACE_OUTER_BOUND ( 'NONE', #32821, .T. ) ;
#1963 = EDGE_LOOP ( 'NONE', ( #1818, #33515, #756, #19170 ) ) ;
#1964 = EDGE_CURVE ( 'NONE', #30554, #5386, #23236, .T. ) ;
#1965 = VERTEX_POINT ( 'NONE', #4843 ) ;
#1966 = EDGE_LOOP ( 'NONE', ( #21280, #17394, #22966, #10202 ) ) ;
#1967 = VECTOR ( 'NONE', #12919, 1000.000000000000000 ) ;
#1968 = CARTESIAN_POINT ( 'NONE',  ( 0.9999999999999870104, -5.408326913195881325, -0.7999999999999951594 ) ) ;
#1969 = CARTESIAN_POINT ( 'NONE',  ( -34.97545270896703329, -114.7691647218148745, 8.590225545821551734 ) ) ;
#1970 = CARTESIAN_POINT ( 'NONE',  ( 47.99999999999998579, 9.267276614348616649E-16, 5.112980201019946931E-16 ) ) ;
#1971 = LINE ( 'NONE', #32208, #9850 ) ;
#1972 = ORIENTED_EDGE ( 'NONE', *, *, #26406, .F. ) ;
#1973 = ORIENTED_EDGE ( 'NONE', *, *, #5562, .T. ) ;
#1974 = CARTESIAN_POINT ( 'NONE',  ( -35.50000000000000711, -112.0577668799241309, 1.173706424699810569 ) ) ;
#1975 = AXIS2_PLACEMENT_3D ( 'NONE', #6813, #4502, #17962 ) ;
#1976 = CIRCLE ( 'NONE', #33587, 4.800000000000000711 ) ;
#1977 = FACE_BOUND ( 'NONE', #1696, .T. ) ;
#1978 = DIRECTION ( 'NONE',  ( -1.000000000000000000, -0.000000000000000000, -0.000000000000000000 ) ) ;
#1979 = ORIENTED_EDGE ( 'NONE', *, *, #20002, .F. ) ;
#1980 = DIRECTION ( 'NONE',  ( 0.8432271980573220471, -4.875366479720417855E-16, -0.5375573387615479870 ) ) ;
#1981 = EDGE_CURVE ( 'NONE', #18606, #26760, #7528, .T. ) ;
#1982 = CARTESIAN_POINT ( 'NONE',  ( 8.000000000000000000, -14.18878633068163708, 6.236773481718040024 ) ) ;
#1983 = CARTESIAN_POINT ( 'NONE',  ( -34.50000000000000000, -114.9929510916434339, 10.52000928670414126 ) ) ;
#1984 = DIRECTION ( 'NONE',  ( -1.000000000000000000, 0.000000000000000000, -0.000000000000000000 ) ) ;
#1985 = CARTESIAN_POINT ( 'NONE',  ( -37.58145695302688694, -114.9929510916434339, 13.11211614918362756 ) ) ;
#1986 = CARTESIAN_POINT ( 'NONE',  ( 0.000000000000000000, 0.000000000000000000, 0.000000000000000000 ) ) ;
#1987 = CARTESIAN_POINT ( 'NONE',  ( -34.50000000000000000, -114.1302255537607095, 9.515717283514957714 ) ) ;
#1988 = CYLINDRICAL_SURFACE ( 'NONE', #23361, 8.000000000000001776 ) ;
#1989 = CARTESIAN_POINT ( 'NONE',  ( -0.1085714285714300953, -3.798448662927791819, -0.7999999999999951594 ) ) ;
#1990 = DIRECTION ( 'NONE',  ( 0.000000000000000000, 0.000000000000000000, 1.000000000000000000 ) ) ;
#1991 = AXIS2_PLACEMENT_3D ( 'NONE', #12118, #6888, #7062 ) ;
#1992 = VERTEX_POINT ( 'NONE', #32021 ) ;
#1993 = DIRECTION ( 'NONE',  ( -1.734723475976806848E-16, -0.5000000000000032196, 0.8660254037844368202 ) ) ;
#1994 = CARTESIAN_POINT ( 'NONE',  ( 0.000000000000000000, -15.46619997295644033, 1.007799283846635863 ) ) ;
#1995 = ADVANCED_FACE ( 'NONE', ( #15784 ), #2332, .T. ) ;
#1996 = ORIENTED_EDGE ( 'NONE', *, *, #26272, .F. ) ;
#1997 = EDGE_CURVE ( 'NONE', #15000, #23250, #32199, .T. ) ;
#1998 = CARTESIAN_POINT ( 'NONE',  ( -37.48437500000004263, -114.9929510916434339, 13.11852480586264669 ) ) ;
#1999 = EDGE_LOOP ( 'NONE', ( #25556, #11854, #21246, #31123 ) ) ;
#2000 = EDGE_CURVE ( 'NONE', #6343, #26262, #18329, .T. ) ;
#2001 = CARTESIAN_POINT ( 'NONE',  ( -38.45611840935523418, -115.3723087153909432, 6.566024454178448266 ) ) ;
#2002 = CARTESIAN_POINT ( 'NONE',  ( 7.999999999999992895, -17.08890430202781374, 43.76671000081938701 ) ) ;
#2003 = ORIENTED_EDGE ( 'NONE', *, *, #8806, .F. ) ;
#2004 = EDGE_LOOP ( 'NONE', ( #5462, #27280, #12409, #29157 ) ) ;
#2005 = SHAPE_REPRESENTATION ( 'circlip for shafts normal_din_Circlip DIN 471 - 8 x 0.8', ( #21307 ), #12197 ) ;
#2006 = CIRCLE ( 'NONE', #8296, 52.00000000000000711 ) ;
#2007 = VECTOR ( 'NONE', #8781, 1000.000000000000000 ) ;
#2008 = LINE ( 'NONE', #10634, #17443 ) ;
#2009 = ADVANCED_FACE ( 'NONE', ( #10048 ), #13131, .T. ) ;
#2010 = EDGE_LOOP ( 'NONE', ( #15652, #9423, #26123, #30004 ) ) ;
#2011 = CARTESIAN_POINT ( 'NONE',  ( -34.02454729103298092, -115.3019030900506294, 4.597274454178449155 ) ) ;
#2012 = EDGE_CURVE ( 'NONE', #5174, #9474, #13646, .T. ) ;
#2013 = CIRCLE ( 'NONE', #14696, 8.000000000000007105 ) ;
#2014 = LINE ( 'NONE', #15484, #3866 ) ;
#2015 = FACE_OUTER_BOUND ( 'NONE', #31439, .T. ) ;
#2016 = EDGE_LOOP ( 'NONE', ( #21254, #27790, #4374, #33130 ) ) ;
#2017 = EDGE_LOOP ( 'NONE', ( #17165, #833, #1097, #12056 ) ) ;
#2018 = CARTESIAN_POINT ( 'NONE',  ( 8.000000000000000000, 15.17386234660406785, -15.92965478239604948 ) ) ;
#2019 =( NAMED_UNIT ( * ) PLANE_ANGLE_UNIT ( ) SI_UNIT ( $, .RADIAN. ) );
#2020 = DIRECTION ( 'NONE',  ( -1.000000000000000000, 0.000000000000000000, 0.000000000000000000 ) ) ;
#2022 = VERTEX_POINT ( 'NONE', #24110 ) ;
#2021 = CIRCLE ( 'NONE', #6590, 7.199999999999994849 ) ;
#2023 = EDGE_LOOP ( 'NONE', ( #27120, #25925, #32769, #521 ) ) ;
#2024 = CARTESIAN_POINT ( 'NONE',  ( -34.50000000000000000, -111.0140978167138570, 0.5627176474015715968 ) ) ;
#2025 = DIRECTION ( 'NONE',  ( 8.708451184622495809E-17, -6.938893903907203726E-17, -1.000000000000000000 ) ) ;
#2026 = ORIENTED_EDGE ( 'NONE', *, *, #21631, .T. ) ;
#2027 = EDGE_LOOP ( 'NONE', ( #13304, #13650, #27522, #7305 ) ) ;
#2028 = CARTESIAN_POINT ( 'NONE',  ( -35.50000000000000711, -114.0650276068786582, 9.507762098804159123 ) ) ;
#2029 = EDGE_CURVE ( 'NONE', #10094, #13248, #18637, .T. ) ;
#2030 = AXIS2_PLACEMENT_3D ( 'NONE', #10176, #9640, #31425 ) ;
#2031 = CARTESIAN_POINT ( 'NONE',  ( -34.50000000000000000, -113.9929510916434339, 10.50625754673586876 ) ) ;
#2032 = CIRCLE ( 'NONE', #12365, 7.199999999999993960 ) ;
#2033 = EDGE_CURVE ( 'NONE', #8928, #4539, #21500, .T. ) ;
#2034 = CARTESIAN_POINT ( 'NONE',  ( 4.000000000000003553, -15.92965478239607968, -15.17386234660401101 ) ) ;
#2035 = CARTESIAN_POINT ( 'NONE',  ( 0.000000000000000000, 3.840921266749832252, 47.34345070675172451 ) ) ;
#2036 = CARTESIAN_POINT ( 'NONE',  ( -34.50000000000000000, -113.9743717753924699, 10.50403980422039396 ) ) ;
#2037 = AXIS2_PLACEMENT_3D ( 'NONE', #13813, #8223, #5538 ) ;
#2038 = CARTESIAN_POINT ( 'NONE',  ( -37.98402046630260287, -115.9929510916434481, 12.74811950270164296 ) ) ;
#2039 = DIRECTION ( 'NONE',  ( 0.000000000000000000, -6.938893903907226800E-15, 1.000000000000000000 ) ) ;
#2040 = VECTOR ( 'NONE', #8936, 1000.000000000000000 ) ;
#2041 = CYLINDRICAL_SURFACE ( 'NONE', #14651, 9.999999999999994671 ) ;
#2042 = EDGE_CURVE ( 'NONE', #7369, #15707, #5996, .T. ) ;
#2043 = ADVANCED_FACE ( 'NONE', ( #26631 ), #2680, .T. ) ;
#2044 = VERTEX_POINT ( 'NONE', #34916 ) ;
#2045 = ADVANCED_FACE ( 'NONE', ( #10242 ), #21015, .F. ) ;
#2046 = CARTESIAN_POINT ( 'NONE',  ( 7.999999999999992895, 47.22458491092828581, -5.098390039073752433 ) ) ;
#2047 = CARTESIAN_POINT ( 'NONE',  ( 8.000000000000007105, -7.613867765417531075, 5.679790370316011305 ) ) ;
#2048 = CARTESIAN_POINT ( 'NONE',  ( 7.999999999999992895, -47.49120266317495975, -0.8606222198180163430 ) ) ;
#2049 = CIRCLE ( 'NONE', #23886, 20.00000000000000000 ) ;
#2050 = ORIENTED_EDGE ( 'NONE', *, *, #20408, .T. ) ;
#2051 = CARTESIAN_POINT ( 'NONE',  ( 0.000000000000000000, 0.000000000000000000, -1.000000000000000888 ) ) ;
#2052 = CARTESIAN_POINT ( 'NONE',  ( -35.50000000000000711, -112.0140900043366088, -0.5935324770972457697 ) ) ;
#2053 = CARTESIAN_POINT ( 'NONE',  ( -46.00000000000000000, 0.000000000000000000, 0.000000000000000000 ) ) ;
#2054 = CARTESIAN_POINT ( 'NONE',  ( -35.50000000000000711, -114.4026847875275337, 9.592046023459676718 ) ) ;
#2055 = CARTESIAN_POINT ( 'NONE',  ( -21.15833593587365513, -41.45319397786874305, 92.20096189432315725 ) ) ;
#2056 = EDGE_CURVE ( 'NONE', #20209, #34767, #10030, .T. ) ;
#2057 = ORIENTED_EDGE ( 'NONE', *, *, #7109, .T. ) ;
#2058 = DIRECTION ( 'NONE',  ( 1.000000000000000000, -5.339440136655842133E-16, -1.047965281155519420E-16 ) ) ;
#2059 = CARTESIAN_POINT ( 'NONE',  ( -35.50000000000000000, -113.3474311500483935, -2.624782352598442614 ) ) ;
#2060 = DIRECTION ( 'NONE',  ( 5.339440136655842133E-16, 1.000000000000000000, -1.918536189538073087E-16 ) ) ;
#2061 = ORIENTED_EDGE ( 'NONE', *, *, #29229, .T. ) ;
#2062 = ORIENTED_EDGE ( 'NONE', *, *, #18309, .T. ) ;
#2063 = CARTESIAN_POINT ( 'NONE',  ( -36.25098837183129774, -113.3347980657956242, 5.816024454178450043 ) ) ;
#2064 = ADVANCED_FACE ( 'NONE', ( #14500 ), #4316, .T. ) ;
#2065 = AXIS2_PLACEMENT_3D ( 'NONE', #10185, #21155, #35049 ) ;
#2066 = FILL_AREA_STYLE_COLOUR ( '', #21340 ) ;
#2067 = CYLINDRICAL_SURFACE ( 'NONE', #11799, 20.00000000000000355 ) ;
#2068 = ORIENTED_EDGE ( 'NONE', *, *, #14371, .T. ) ;
#2069 = ORIENTED_EDGE ( 'NONE', *, *, #2492, .T. ) ;
#2070 = CARTESIAN_POINT ( 'NONE',  ( -34.50000000000000000, -113.0140978167138712, -0.6247823525988807081 ) ) ;
#2071 = DIRECTION ( 'NONE',  ( -1.000000000000000000, 0.000000000000000000, 0.000000000000000000 ) ) ;
#2072 = EDGE_CURVE ( 'NONE', #25710, #20884, #22267, .T. ) ;
#2073 = DIRECTION ( 'NONE',  ( -1.000000000000000000, 0.000000000000000000, 0.000000000000000000 ) ) ;
#2074 = AXIS2_PLACEMENT_3D ( 'NONE', #14194, #22117, #32936 ) ;
#2075 = EDGE_CURVE ( 'NONE', #6952, #3956, #9457, .T. ) ;
#2076 = CARTESIAN_POINT ( 'NONE',  ( -37.99839555572501837, -114.9929510916434339, 12.65937477241748965 ) ) ;
#2077 = EDGE_CURVE ( 'NONE', #7954, #25710, #12338, .T. ) ;
#2078 = CARTESIAN_POINT ( 'NONE',  ( 0.000000000000000000, -5.908880290975456973, -9.604183132802479150 ) ) ;
#2079 = DIRECTION ( 'NONE',  ( -1.000000000000000000, 0.000000000000000000, 0.000000000000000000 ) ) ;
#2080 = CARTESIAN_POINT ( 'NONE',  ( -34.50000000000000000, -112.0269151300720409, -0.7876962586524208776 ) ) ;
#2081 = LINE ( 'NONE', #13061, #11372 ) ;
#2082 = CARTESIAN_POINT ( 'NONE',  ( 0.000000000000000000, 0.000000000000000000, 0.000000000000000000 ) ) ;
#2083 = CIRCLE ( 'NONE', #15818, 3.999999999999996447 ) ;
#2084 = EDGE_CURVE ( 'NONE', #25259, #21336, #4883, .T. ) ;
#2085 = DIRECTION ( 'NONE',  ( 0.000000000000000000, -1.000000000000000000, 0.000000000000000000 ) ) ;
#2086 = VERTEX_POINT ( 'NONE', #489 ) ;
#2087 = CARTESIAN_POINT ( 'NONE',  ( -35.50000000000000000, -115.9929510916434481, 12.57451923796416260 ) ) ;
#2088 = CARTESIAN_POINT ( 'NONE',  ( -35.50000000000000711, -115.9821387493194891, -0.8839717462762166633 ) ) ;
#2089 = LINE ( 'NONE', #5145, #15629 ) ;
#2090 = EDGE_CURVE ( 'NONE', #3377, #6697, #2006, .T. ) ;
#2091 = CARTESIAN_POINT ( 'NONE',  ( 0.000000000000000000, 0.000000000000000000, 0.000000000000000000 ) ) ;
#2092 = AXIS2_PLACEMENT_3D ( 'NONE', #17775, #33632, #17418 ) ;
#2093 = DIRECTION ( 'NONE',  ( -1.000000000000000000, -0.000000000000000000, 0.000000000000000000 ) ) ;
#2094 = VERTEX_POINT ( 'NONE', #6067 ) ;
#2095 = CIRCLE ( 'NONE', #3323, 47.49900000000000944 ) ;
#2096 = CARTESIAN_POINT ( 'NONE',  ( -55.00000000000000000, 19.99999999999998934, -15.00000000000001421 ) ) ;
#2097 = CARTESIAN_POINT ( 'NONE',  ( 3.999999999999996447, -21.80633394113452539, 2.912696353505744185 ) ) ;
#2098 = DIRECTION ( 'NONE',  ( -1.783119874454246424E-31, -1.187911941725854497E-31, 1.000000000000000000 ) ) ;
#2099 = CARTESIAN_POINT ( 'NONE',  ( -54.99999999999998579, -64.99999999999997158, 120.0000000000000000 ) ) ;
#2100 = CARTESIAN_POINT ( 'NONE',  ( -37.66520193420439000, -113.2509883718312977, 6.941024454178450043 ) ) ;
#2101 = VECTOR ( 'NONE', #30695, 1000.000000000000000 ) ;
#2102 = CARTESIAN_POINT ( 'NONE',  ( 8.000000000000000000, 0.000000000000000000, 0.000000000000000000 ) ) ;
#2103 = DIRECTION ( 'NONE',  ( 1.000000000000000000, 0.000000000000000000, 0.000000000000000000 ) ) ;
#2104 = ORIENTED_EDGE ( 'NONE', *, *, #28162, .F. ) ;
#2105 = AXIS2_PLACEMENT_3D ( 'NONE', #31118, #28073, #6620 ) ;
#2106 = VERTEX_POINT ( 'NONE', #22608 ) ;
#2107 =( REPRESENTATION_RELATIONSHIP ('NONE','NONE', #26607, #2005 ) REPRESENTATION_RELATIONSHIP_WITH_TRANSFORMATION ( #23469 )SHAPE_REPRESENTATION_RELATIONSHIP( ) );
#2108 = CARTESIAN_POINT ( 'NONE',  ( 0.000000000000000000, 0.000000000000000000, 0.000000000000000000 ) ) ;
#2109 = DIRECTION ( 'NONE',  ( 1.000000000000000000, 0.000000000000000000, 0.000000000000000000 ) ) ;
#2110 = CARTESIAN_POINT ( 'NONE',  ( 0.000000000000000000, 0.000000000000000000, 0.000000000000000000 ) ) ;
#2111 = VERTEX_POINT ( 'NONE', #22091 ) ;
#2112 = CARTESIAN_POINT ( 'NONE',  ( -37.05926240293131713, -112.0000000000000142, 5.121475545821551734 ) ) ;
#2113 = ORIENTED_EDGE ( 'NONE', *, *, #8351, .T. ) ;
#2114 = ORIENTED_EDGE ( 'NONE', *, *, #23354, .F. ) ;
#2115 = VERTEX_POINT ( 'NONE', #19389 ) ;
#2116 = CARTESIAN_POINT ( 'NONE',  ( 4.000000000000003553, 15.17386234660407140, -15.92965478239605304 ) ) ;
#2117 = VECTOR ( 'NONE', #31383, 1000.000000000000000 ) ;
#2118 = CIRCLE ( 'NONE', #30271, 4.800000000000005151 ) ;
#2119 = AXIS2_PLACEMENT_3D ( 'NONE', #20819, #4833, #23543 ) ;
#2120 = EDGE_CURVE ( 'NONE', #21198, #7610, #10947, .T. ) ;
#2121 = FACE_OUTER_BOUND ( 'NONE', #15572, .T. ) ;
#2122 = EDGE_LOOP ( 'NONE', ( #10353, #19149, #3304, #34630 ) ) ;
#2123 = EDGE_LOOP ( 'NONE', ( #19667, #24283, #27688, #14747 ) ) ;
#2124 = VECTOR ( 'NONE', #11080, 1000.000000000000000 ) ;
#2125 = ADVANCED_FACE ( 'NONE', ( #13990 ), #27692, .T. ) ;
#2126 = CARTESIAN_POINT ( 'NONE',  ( 0.000000000000000000, 0.000000000000000000, 0.000000000000000000 ) ) ;
#2127 = FACE_OUTER_BOUND ( 'NONE', #12727, .T. ) ;
#2128 = VECTOR ( 'NONE', #14487, 1000.000000000000114 ) ;
#2129 = VERTEX_POINT ( 'NONE', #21915 ) ;
#2130 = DIRECTION ( 'NONE',  ( 1.000000000000000000, -5.339440136655839175E-16, 0.000000000000000000 ) ) ;
#2131 = STYLED_ITEM ( 'NONE', ( #16410 ), #34958 ) ;
#2132 = AXIS2_PLACEMENT_3D ( 'NONE', #26977, #16129, #35605 ) ;
#2133 = DIRECTION ( 'NONE',  ( 1.000000000000000000, 0.000000000000000000, 0.000000000000000000 ) ) ;
#2134 = DIRECTION ( 'NONE',  ( -1.000000000000000000, -0.000000000000000000, -0.000000000000000000 ) ) ;
#2135 = DIRECTION ( 'NONE',  ( 0.000000000000000000, 1.000000000000000000, 0.000000000000000000 ) ) ;
#2136 = CARTESIAN_POINT ( 'NONE',  ( -38.45611840935523418, -115.3723087153909432, 5.066024454178449155 ) ) ;
#2137 = CARTESIAN_POINT ( 'NONE',  ( -34.50000000000000000, -115.6492853190479337, 9.359470924297957239 ) ) ;
#2138 = DIRECTION ( 'NONE',  ( -1.783119874454246424E-31, -1.187911941725854497E-31, 1.000000000000000000 ) ) ;
#2139 = CIRCLE ( 'NONE', #25120, 47.49900000000001654 ) ;
#2140 = CARTESIAN_POINT ( 'NONE',  ( -39.49999999999999289, -13.10640646055107084, 90.70096189432331357 ) ) ;
#2141 = AXIS2_PLACEMENT_3D ( 'NONE', #4828, #4661, #4297 ) ;
#2142 = DIRECTION ( 'NONE',  ( -1.000000000000000000, -0.000000000000000000, -0.000000000000000000 ) ) ;
#2143 = DIRECTION ( 'NONE',  ( -1.000000000000000000, 0.000000000000000000, 0.000000000000000000 ) ) ;
#2144 = AXIS2_PLACEMENT_3D ( 'NONE', #8926, #2852, #6060 ) ;
#2145 = DIRECTION ( 'NONE',  ( 1.000000000000000000, -5.339440136655842133E-16, -1.047965281155519420E-16 ) ) ;
#2146 = FACE_OUTER_BOUND ( 'NONE', #10993, .T. ) ;
#2147 = ORIENTED_EDGE ( 'NONE', *, *, #19604, .F. ) ;
#2148 = CARTESIAN_POINT ( 'NONE',  ( -35.62769128460905677, -112.5438815906447729, 5.308975545821551734 ) ) ;
#2149 = AXIS2_PLACEMENT_3D ( 'NONE', #20325, #28990, #26298 ) ;
#2150 = DIRECTION ( 'NONE',  ( -1.000000000000000000, 0.000000000000000000, 0.000000000000000000 ) ) ;
#2151 = AXIS2_PLACEMENT_3D ( 'NONE', #17549, #33959, #6233 ) ;
#2152 = DIRECTION ( 'NONE',  ( 1.047965281155515106E-16, -6.938893903907203726E-17, -1.000000000000000000 ) ) ;
#2153 = ORIENTED_EDGE ( 'NONE', *, *, #1887, .T. ) ;
#2154 = EDGE_LOOP ( 'NONE', ( #32633, #8100, #15394, #33809 ) ) ;
#2155 = CIRCLE ( 'NONE', #32018, 4.800000000000000711 ) ;
#2156 = CARTESIAN_POINT ( 'NONE',  ( 0.000000000000000000, 46.11014828289842882, -9.022736828080857308 ) ) ;
#2157 = CARTESIAN_POINT ( 'NONE',  ( 0.000000000000000000, -11.90021268425521939, -45.45261810511225065 ) ) ;
#2158 = VERTEX_POINT ( 'NONE', #5888 ) ;
#2159 = AXIS2_PLACEMENT_3D ( 'NONE', #24105, #29857, #15780 ) ;
#2160 = ORIENTED_EDGE ( 'NONE', *, *, #21209, .T. ) ;
#2161 = VECTOR ( 'NONE', #5248, 1000.000000000000000 ) ;
#2162 = AXIS2_PLACEMENT_3D ( 'NONE', #34855, #34495, #26203 ) ;
#2163 = CARTESIAN_POINT ( 'NONE',  ( 7.999999999999992895, 8.053585752061906078, 46.81126742072027014 ) ) ;
#2164 = CARTESIAN_POINT ( 'NONE',  ( -37.05926240293131713, -112.0000000000000142, 9.621475545821551734 ) ) ;
#2165 = DIRECTION ( 'NONE',  ( 1.000000000000000000, 0.000000000000000000, 0.000000000000000000 ) ) ;
#2166 = DIRECTION ( 'NONE',  ( -1.000000000000000000, 0.000000000000000000, 0.000000000000000000 ) ) ;
#2167 = CIRCLE ( 'NONE', #11345, 4.000000000000003553 ) ;
#2168 = ORIENTED_EDGE ( 'NONE', *, *, #34254, .F. ) ;
#2169 = ORIENTED_EDGE ( 'NONE', *, *, #33690, .T. ) ;
#2170 = CARTESIAN_POINT ( 'NONE',  ( -35.50000000000000711, -112.0140978167138712, 0.7502176474015694874 ) ) ;
#2171 = EDGE_CURVE ( 'NONE', #13101, #10171, #22102, .T. ) ;
#2172 = AXIS2_PLACEMENT_3D ( 'NONE', #9053, #6001, #11576 ) ;
#2173 = LINE ( 'NONE', #21746, #32980 ) ;
#2174 = DIRECTION ( 'NONE',  ( -1.000000000000000000, 0.000000000000000000, 0.000000000000000000 ) ) ;
#2175 = VERTEX_POINT ( 'NONE', #654 ) ;
#2176 = DIRECTION ( 'NONE',  ( -1.000000000000000000, 0.000000000000000000, 0.000000000000000000 ) ) ;
#2177 = AXIS2_PLACEMENT_3D ( 'NONE', #3570, #14517, #25531 ) ;
#2178 = AXIS2_PLACEMENT_3D ( 'NONE', #35388, #16804, #8534 ) ;
#2179 = FACE_OUTER_BOUND ( 'NONE', #13270, .T. ) ;
#2180 = CIRCLE ( 'NONE', #30327, 47.49900000000000944 ) ;
#2181 = CARTESIAN_POINT ( 'NONE',  ( -34.80050084267117683, -114.9929510916434339, 13.54034599209289169 ) ) ;
#2182 = DIRECTION ( 'NONE',  ( -1.000000000000000000, 0.000000000000000000, 0.000000000000000000 ) ) ;
#2183 = CARTESIAN_POINT ( 'NONE',  ( -37.98402046630260287, -114.9929510916434339, 12.74811950270164118 ) ) ;
#2184 = LINE ( 'NONE', #23948, #2502 ) ;
#2185 = EDGE_CURVE ( 'NONE', #12261, #34373, #29027, .T. ) ;
#2186 = CARTESIAN_POINT ( 'NONE',  ( -34.50000000000000000, -114.9656200615856818, 10.26631071845107179 ) ) ;
#2187 = CARTESIAN_POINT ( 'NONE',  ( -3.799999999999999822, 4.382607293638566128E-16, 38.00000000000000711 ) ) ;
#2188 = AXIS2_PLACEMENT_3D ( 'NONE', #11595, #3159, #25470 ) ;
#2189 = CARTESIAN_POINT ( 'NONE',  ( 8.000000000000007105, 1.111908866155100650, 9.433698091065117808 ) ) ;
#2190 = DIRECTION ( 'NONE',  ( 1.000000000000000000, -4.524158825347490025E-15, -1.174092375852883357E-15 ) ) ;
#2191 = VERTEX_POINT ( 'NONE', #33599 ) ;
#2192 = DIRECTION ( 'NONE',  ( -1.000000000000000000, 1.110223024625156540E-16, 0.000000000000000000 ) ) ;
#2193 = LINE ( 'NONE', #27017, #17471 ) ;
#2194 = ORIENTED_EDGE ( 'NONE', *, *, #3621, .F. ) ;
#2195 = CARTESIAN_POINT ( 'NONE',  ( -38.00000068757622529, -114.9929510916434339, 12.61439929482944855 ) ) ;
#2196 = ORIENTED_EDGE ( 'NONE', *, *, #2411, .T. ) ;
#2197 = CARTESIAN_POINT ( 'NONE',  ( -39.99999999999999289, -113.9407375970686758, 2.253524454178448710 ) ) ;
#2198 = CARTESIAN_POINT ( 'NONE',  ( 8.000000000000000000, -16.59870953437682672, 3.253005020243791456 ) ) ;
#2199 = AXIS2_PLACEMENT_3D ( 'NONE', #33545, #14447, #424 ) ;
#2200 = ORIENTED_EDGE ( 'NONE', *, *, #30624, .T. ) ;
#2201 = EDGE_LOOP ( 'NONE', ( #10508, #26216 ) ) ;
#2202 = AXIS2_PLACEMENT_3D ( 'NONE', #2838, #30368, #33062 ) ;
#2203 = CARTESIAN_POINT ( 'NONE',  ( -44.00000000000000000, 11.00000000000000000, 1.347111479062088405E-15 ) ) ;
#2204 = VERTEX_POINT ( 'NONE', #16506 ) ;
#2205 = CARTESIAN_POINT ( 'NONE',  ( -34.92058450342251064, -116.1632251905417945, 4.691024454178447378 ) ) ;
#2206 = AXIS2_PLACEMENT_3D ( 'NONE', #1609, #34195, #28792 ) ;
#2207 = AXIS2_PLACEMENT_3D ( 'NONE', #18684, #26994, #13309 ) ;
#2208 = DIRECTION ( 'NONE',  ( -1.000000000000000000, 0.000000000000000000, -0.000000000000000000 ) ) ;
#2209 = DIRECTION ( 'NONE',  ( -1.000000000000000000, 0.000000000000000000, 0.000000000000000000 ) ) ;
#2210 = VERTEX_POINT ( 'NONE', #8932 ) ;
#2211 = VERTEX_POINT ( 'NONE', #33087 ) ;
#2212 = DIRECTION ( 'NONE',  ( -1.000000000000000000, -0.000000000000000000, -0.000000000000000000 ) ) ;
#2213 = AXIS2_PLACEMENT_3D ( 'NONE', #31489, #26629, #31832 ) ;
#2214 = CARTESIAN_POINT ( 'NONE',  ( 4.000000000000003553, 15.92965478239641008, -15.17386234660366284 ) ) ;
#2215 = ORIENTED_EDGE ( 'NONE', *, *, #19628, .T. ) ;
#2216 = ORIENTED_EDGE ( 'NONE', *, *, #904, .F. ) ;
#2217 = CARTESIAN_POINT ( 'NONE',  ( -34.50000000000000000, -111.0140978167138570, 0.2502176474015764263 ) ) ;
#2218 = ADVANCED_FACE ( 'NONE', ( #30909 ), #6245, .T. ) ;
#2219 = EDGE_CURVE ( 'NONE', #1802, #4018, #27520, .T. ) ;
#2220 = FACE_OUTER_BOUND ( 'NONE', #24548, .T. ) ;
#2221 = ORIENTED_EDGE ( 'NONE', *, *, #22660, .F. ) ;
#2222 = CARTESIAN_POINT ( 'NONE',  ( -35.50000000000000711, -114.9925223117477202, 10.47601618151863079 ) ) ;
#2223 = CARTESIAN_POINT ( 'NONE',  ( -38.00000000000000711, -113.9929510916434339, 10.85830208992306822 ) ) ;
#2224 = CARTESIAN_POINT ( 'NONE',  ( -9.999999999999994671, 0.000000000000000000, 0.000000000000000000 ) ) ;
#2225 = FACE_OUTER_BOUND ( 'NONE', #18607, .T. ) ;
#2226 = ADVANCED_FACE ( 'NONE', ( #3202 ), #13820, .T. ) ;
#2227 = CARTESIAN_POINT ( 'NONE',  ( -37.58145695302688694, -113.9929510916434339, 13.11211614918362756 ) ) ;
#2228 = EDGE_CURVE ( 'NONE', #14555, #32804, #26047, .T. ) ;
#2229 = CARTESIAN_POINT ( 'NONE',  ( -37.37500000000009237, -115.9929510916434481, 13.11852480586264846 ) ) ;
#2230 = CARTESIAN_POINT ( 'NONE',  ( 8.000000000000007105, -8.725776631572701447, 3.753907720749016796 ) ) ;
#2231 = CIRCLE ( 'NONE', #18875, 8.000000000000051514 ) ;
#2232 = PLANE ( 'NONE',  #16375 ) ;
#2233 = EDGE_LOOP ( 'NONE', ( #14028, #3994, #27129, #18101 ) ) ;
#2234 = DIRECTION ( 'NONE',  ( -1.000000000000000000, 0.000000000000000000, 0.000000000000000000 ) ) ;
#2235 = LINE ( 'NONE', #24354, #1309 ) ;
#2236 = AXIS2_PLACEMENT_3D ( 'NONE', #15972, #26802, #5204 ) ;
#2237 = CARTESIAN_POINT ( 'NONE',  ( 7.999999999999992895, -0.2227391519113268437, -46.98410307550732057 ) ) ;
#2238 = ORIENTED_EDGE ( 'NONE', *, *, #6902, .T. ) ;
#2239 = ADVANCED_BREP_SHAPE_REPRESENTATION ( '', ( #22718, #21307 ), #12197 ) ;
#2240 = LINE ( 'NONE', #24180, #6682 ) ;
#2241 = CARTESIAN_POINT ( 'NONE',  ( -35.50000000000000711, -112.6043641208289188, 1.789429170677330649 ) ) ;
#2242 = FACE_OUTER_BOUND ( 'NONE', #30179, .T. ) ;
#2243 = CARTESIAN_POINT ( 'NONE',  ( -35.50000000000000711, -114.9929510916434339, 12.44250253426871033 ) ) ;
#2244 = DIRECTION ( 'NONE',  ( -1.000000000000000000, 0.000000000000000000, 0.000000000000000000 ) ) ;
#2245 = EDGE_CURVE ( 'NONE', #13869, #27693, #12180, .T. ) ;
#2246 = ORIENTED_EDGE ( 'NONE', *, *, #21285, .T. ) ;
#2247 = DIRECTION ( 'NONE',  ( 9.615983791445651082E-17, -6.938893903907203726E-17, -1.000000000000000000 ) ) ;
#2248 = CARTESIAN_POINT ( 'NONE',  ( -35.50000000000000000, -114.3474311500471572, -2.624782352598442614 ) ) ;
#2249 = ORIENTED_EDGE ( 'NONE', *, *, #7391, .F. ) ;
#2250 = ORIENTED_EDGE ( 'NONE', *, *, #33891, .T. ) ;
#2251 = CARTESIAN_POINT ( 'NONE',  ( -37.76916472181487450, -111.9754527089670404, 2.534774454178448710 ) ) ;
#2252 = AXIS2_PLACEMENT_3D ( 'NONE', #10917, #4983, #24777 ) ;
#2253 = VECTOR ( 'NONE', #6220, 1000.000000000000114 ) ;
#2254 = DIRECTION ( 'NONE',  ( 0.000000000000000000, 0.000000000000000000, -1.000000000000000000 ) ) ;
#2255 = ORIENTED_EDGE ( 'NONE', *, *, #8629, .F. ) ;
#2256 = ORIENTED_EDGE ( 'NONE', *, *, #27606, .T. ) ;
#2257 = VECTOR ( 'NONE', #1343, 1000.000000000000000 ) ;
#2258 = CARTESIAN_POINT ( 'NONE',  ( -34.50000000000000000, -112.9977353549762000, -0.6247823525983134951 ) ) ;
#2259 = EDGE_CURVE ( 'NONE', #6879, #19623, #19786, .T. ) ;
#2260 = EDGE_CURVE ( 'NONE', #17795, #35062, #21522, .T. ) ;
#2261 = EDGE_CURVE ( 'NONE', #18178, #17571, #6573, .T. ) ;
#2262 = DIRECTION ( 'NONE',  ( -1.000000000000000000, 0.000000000000000000, 0.000000000000000000 ) ) ;
#2263 = CARTESIAN_POINT ( 'NONE',  ( 0.000000000000000000, 0.5097555531875970214, -19.99350267651952606 ) ) ;
#2264 = CARTESIAN_POINT ( 'NONE',  ( -38.00000000000000711, -114.9929510916434339, 12.60752341388803721 ) ) ;
#2265 = DIRECTION ( 'NONE',  ( 0.000000000000000000, 0.8660254037844444808, -0.4999999999999898415 ) ) ;
#2266 = DIRECTION ( 'NONE',  ( -0.000000000000000000, 1.000000000000000000, 0.000000000000000000 ) ) ;
#2267 = EDGE_CURVE ( 'NONE', #21074, #13818, #12004, .T. ) ;
#2268 = CARTESIAN_POINT ( 'NONE',  ( -34.50000000000000000, -113.4307644833805000, -1.624782352598427959 ) ) ;
#2269 = EDGE_CURVE ( 'NONE', #8899, #20033, #2601, .T. ) ;
#2270 = CARTESIAN_POINT ( 'NONE',  ( 7.999999999999992895, 36.34385289850631295, -29.77717097092039111 ) ) ;
#2271 = CARTESIAN_POINT ( 'NONE',  ( -36.49999999999999289, -12.47865190846804495, 110.2774766518096925 ) ) ;
#2272 = ORIENTED_EDGE ( 'NONE', *, *, #11488, .F. ) ;
#2273 = CARTESIAN_POINT ( 'NONE',  ( -35.50000000000000711, -114.0882517521923489, 9.510534276948430232 ) ) ;
#2274 = CARTESIAN_POINT ( 'NONE',  ( -3.799999999999999822, 4.653657836759942730E-16, 36.00000000000000000 ) ) ;
#2275 = LINE ( 'NONE', #13243, #709 ) ;
#2276 = DIRECTION ( 'NONE',  ( 0.000000000000000000, 0.000000000000000000, 1.000000000000000000 ) ) ;
#2277 = DIRECTION ( 'NONE',  ( -1.000000000000000000, 5.339440136655861854E-16, 0.000000000000000000 ) ) ;
#2278 = ORIENTED_EDGE ( 'NONE', *, *, #26040, .F. ) ;
#2279 = CIRCLE ( 'NONE', #10897, 10.49999999999999645 ) ;
#2280 = DIRECTION ( 'NONE',  ( 3.154042683594195121E-16, -1.000000000000000000, 0.000000000000000000 ) ) ;
#2281 = CARTESIAN_POINT ( 'NONE',  ( 0.000000000000000000, -2.710505431213761085E-17, 45.89999999999999858 ) ) ;
#2282 = DIRECTION ( 'NONE',  ( -1.000000000000000000, 0.000000000000000000, 0.000000000000000000 ) ) ;
#2283 = DIRECTION ( 'NONE',  ( 0.000000000000000000, 0.000000000000000000, 1.000000000000000000 ) ) ;
#2284 = LINE ( 'NONE', #16455, #19273 ) ;
#2285 = DIRECTION ( 'NONE',  ( 0.000000000000000000, 0.000000000000000000, -1.000000000000000000 ) ) ;
#2286 = ADVANCED_FACE ( 'NONE', ( #20615 ), #34149, .T. ) ;
#2287 = EDGE_LOOP ( 'NONE', ( #13173, #12637, #23366, #24486 ) ) ;
#2288 = VERTEX_POINT ( 'NONE', #17558 ) ;
#2289 = DIRECTION ( 'NONE',  ( 0.000000000000000000, -6.983129352544636959E-15, 1.000000000000000000 ) ) ;
#2290 = CYLINDRICAL_SURFACE ( 'NONE', #32641, 4.000000000000000000 ) ;
#2291 = ADVANCED_FACE ( 'NONE', ( #17924 ), #9471, .F. ) ;
#2292 = DIRECTION ( 'NONE',  ( -1.000000000000000000, -0.000000000000000000, -0.000000000000000000 ) ) ;
#2293 = ORIENTED_EDGE ( 'NONE', *, *, #2616, .T. ) ;
#2294 = CARTESIAN_POINT ( 'NONE',  ( -35.54388159064475872, -115.3723087153909432, 7.183975545821551734 ) ) ;
#2295 = ORIENTED_EDGE ( 'NONE', *, *, #1583, .T. ) ;
#2296 = EDGE_CURVE ( 'NONE', #31709, #31717, #8888, .T. ) ;
#2297 = ORIENTED_EDGE ( 'NONE', *, *, #11976, .F. ) ;
#2298 = ORIENTED_EDGE ( 'NONE', *, *, #1210, .F. ) ;
#2299 = FACE_OUTER_BOUND ( 'NONE', #28981, .T. ) ;
#2300 = EDGE_CURVE ( 'NONE', #17838, #10539, #13512, .T. ) ;
#2301 = AXIS2_PLACEMENT_3D ( 'NONE', #14881, #3933, #26600 ) ;
#2302 = EDGE_CURVE ( 'NONE', #19176, #17996, #9826, .T. ) ;
#2303 = FACE_OUTER_BOUND ( 'NONE', #6582, .T. ) ;
#2304 = VERTEX_POINT ( 'NONE', #7127 ) ;
#2305 = EDGE_LOOP ( 'NONE', ( #16724, #26388, #32363, #12762 ) ) ;
#2306 = CARTESIAN_POINT ( 'NONE',  ( -4.121423858225413461, -12.61643262889540473, 0.000000000000000000 ) ) ;
#2307 = DIRECTION ( 'NONE',  ( 0.000000000000000000, 0.000000000000000000, 1.000000000000000000 ) ) ;
#2308 = AXIS2_PLACEMENT_3D ( 'NONE', #11711, #24881, #6143 ) ;
#2309 = AXIS2_PLACEMENT_3D ( 'NONE', #26097, #1249, #34387 ) ;
#2310 = CARTESIAN_POINT ( 'NONE',  ( -1.479000000000007420, -4.846123502488801633E-16, -6.984000000000015085 ) ) ;
#2311 = AXIS2_PLACEMENT_3D ( 'NONE', #28801, #12776, #4327 ) ;
#2312 = CARTESIAN_POINT ( 'NONE',  ( 2.141980652367342586, -6.189445006155629869, 0.000000000000000000 ) ) ;
#2313 = DIRECTION ( 'NONE',  ( 1.000000000000000000, -1.110223024625156540E-16, 0.000000000000000000 ) ) ;
#2314 = CARTESIAN_POINT ( 'NONE',  ( -37.76916472181487450, -111.9754527089670404, 4.034774454178449155 ) ) ;
#2315 = CARTESIAN_POINT ( 'NONE',  ( -34.50000000000000000, -115.9929510916434481, 12.26648026267477398 ) ) ;
#2316 = DIRECTION ( 'NONE',  ( -1.000000000000000000, -8.673617379884000959E-17, -1.502314598737161250E-16 ) ) ;
#2317 = DIRECTION ( 'NONE',  ( -1.000000000000000000, 0.000000000000000000, 0.000000000000000000 ) ) ;
#2318 = DIRECTION ( 'NONE',  ( -1.000000000000000000, 0.000000000000000000, 0.000000000000000000 ) ) ;
#2319 = CARTESIAN_POINT ( 'NONE',  ( 7.999999999999992895, 17.08890430202814059, -43.76671000081924490 ) ) ;
#2320 = DIRECTION ( 'NONE',  ( 0.000000000000000000, 0.8090169943749448977, 0.5877852522924766898 ) ) ;
#2321 = CARTESIAN_POINT ( 'NONE',  ( 0.000000000000000000, -2.710505431213761085E-17, -45.10000000000000142 ) ) ;
#2322 = EDGE_LOOP ( 'NONE', ( #32675, #6013, #15390, #21965 ) ) ;
#2323 = AXIS2_PLACEMENT_3D ( 'NONE', #12509, #34482, #9801 ) ;
#2324 = CARTESIAN_POINT ( 'NONE',  ( -34.83677480945821259, -116.0794154965774965, 8.683975545821549957 ) ) ;
#2325 = CARTESIAN_POINT ( 'NONE',  ( 3.872983346207429900, -1.000000000000003553, -30.00000000000000711 ) ) ;
#2326 = CARTESIAN_POINT ( 'NONE',  ( 8.000000000000000000, 0.000000000000000000, 0.000000000000000000 ) ) ;
#2327 = ADVANCED_FACE ( 'NONE', ( #28384 ), #31441, .T. ) ;
#2328 = ORIENTED_EDGE ( 'NONE', *, *, #10515, .T. ) ;
#2329 = CIRCLE ( 'NONE', #5778, 20.00000000000000711 ) ;
#2330 = VERTEX_POINT ( 'NONE', #28745 ) ;
#2331 = ADVANCED_FACE ( 'NONE', ( #31792 ), #18100, .T. ) ;
#2332 = CYLINDRICAL_SURFACE ( 'NONE', #35340, 52.00000000000000711 ) ;
#2333 = ORIENTED_EDGE ( 'NONE', *, *, #28174, .T. ) ;
#2334 = ORIENTED_EDGE ( 'NONE', *, *, #3653, .T. ) ;
#2335 = VECTOR ( 'NONE', #23318, 999.9999999999998863 ) ;
#2336 = PRODUCT_DEFINITION_FORMATION_WITH_SPECIFIED_SOURCE ( 'ANY', '', #29075, .NOT_KNOWN. ) ;
#2337 = VECTOR ( 'NONE', #32741, 1000.000000000000000 ) ;
#2338 = FACE_OUTER_BOUND ( 'NONE', #3922, .T. ) ;
#2339 = CARTESIAN_POINT ( 'NONE',  ( -36.23083527818513261, -111.9754527089670404, 9.715225545821551734 ) ) ;
#2340 = DIRECTION ( 'NONE',  ( 1.000000000000000000, 1.006139616066547868E-16, 5.551115123125782702E-17 ) ) ;
#2341 = CARTESIAN_POINT ( 'NONE',  ( 7.999999999999992895, 0.000000000000000000, 0.000000000000000000 ) ) ;
#2342 = EDGE_LOOP ( 'NONE', ( #31787, #21630, #16161, #3142, #11858 ) ) ;
#2343 = ORIENTED_EDGE ( 'NONE', *, *, #14120, .F. ) ;
#2344 = CARTESIAN_POINT ( 'NONE',  ( -35.50000000000000711, -112.0141059978162019, -0.6575071456984691309 ) ) ;
#2345 = FACE_OUTER_BOUND ( 'NONE', #31950, .T. ) ;
#2346 = AXIS2_PLACEMENT_3D ( 'NONE', #11575, #33536, #11404 ) ;
#2347 = DIRECTION ( 'NONE',  ( 1.084202172485500613E-16, -6.938893903907203726E-17, -1.000000000000000000 ) ) ;
#2348 = ORIENTED_EDGE ( 'NONE', *, *, #9015, .F. ) ;
#2349 = DIRECTION ( 'NONE',  ( 0.000000000000000000, 0.9822872507286891652, -0.1873813145857216034 ) ) ;
#2350 = CARTESIAN_POINT ( 'NONE',  ( -34.50000000000000000, -116.0012805033554883, -0.7876962586524312027 ) ) ;
#2351 = CARTESIAN_POINT ( 'NONE',  ( -36.24999999999983658, -114.9929510916434339, 14.11852480586264846 ) ) ;
#2352 = FACE_OUTER_BOUND ( 'NONE', #34563, .T. ) ;
#2353 = CARTESIAN_POINT ( 'NONE',  ( -35.50000000000000000, -113.9929510916434339, 10.53376102667243508 ) ) ;
#2354 = CARTESIAN_POINT ( 'NONE',  ( 0.000000000000000000, 0.000000000000000000, -40.40000000000000568 ) ) ;
#2355 = VECTOR ( 'NONE', #11953, 1000.000000000000000 ) ;
#2356 = CARTESIAN_POINT ( 'NONE',  ( -34.50000000000000000, -114.9929510916434339, 10.52826033068511435 ) ) ;
#2357 = DIRECTION ( 'NONE',  ( -1.000000000000000000, 0.000000000000000000, 0.000000000000000000 ) ) ;
#2358 = CARTESIAN_POINT ( 'NONE',  ( -37.80727372874345349, -114.9929510916434339, 13.01835785830664527 ) ) ;
#2359 = CARTESIAN_POINT ( 'NONE',  ( 0.000000000000000000, -5.908880290975582206, 9.604183132802395662 ) ) ;
#2360 = ORIENTED_EDGE ( 'NONE', *, *, #664, .F. ) ;
#2361 = CARTESIAN_POINT ( 'NONE',  ( 0.000000000000000000, 0.000000000000000000, -0.7999999999999951594 ) ) ;
#2362 = FACE_OUTER_BOUND ( 'NONE', #12722, .T. ) ;
#2363 = EDGE_LOOP ( 'NONE', ( #14878, #11766, #29319, #29549 ) ) ;
#2364 = CARTESIAN_POINT ( 'NONE',  ( -37.99359134332094357, -114.9929510916434339, 12.69998175888958158 ) ) ;
#2365 = ORIENTED_EDGE ( 'NONE', *, *, #14298, .T. ) ;
#2366 = CARTESIAN_POINT ( 'NONE',  ( -36.94073759706868287, -112.0000000000000142, 4.128524454178449155 ) ) ;
#2367 = DIRECTION ( 'NONE',  ( -1.000000000000000000, 0.000000000000000000, 0.000000000000000000 ) ) ;
#2368 = ORIENTED_EDGE ( 'NONE', *, *, #29562, .F. ) ;
#2369 = ORIENTED_EDGE ( 'NONE', *, *, #34308, .T. ) ;
#2370 = EDGE_CURVE ( 'NONE', #688, #26487, #25513, .T. ) ;
#2371 = LINE ( 'NONE', #24845, #7352 ) ;
#2372 = FACE_OUTER_BOUND ( 'NONE', #14967, .T. ) ;
#2373 = AXIS2_PLACEMENT_3D ( 'NONE', #30750, #22812, #9139 ) ;
#2374 = ORIENTED_EDGE ( 'NONE', *, *, #11027, .F. ) ;
#2375 = CARTESIAN_POINT ( 'NONE',  ( -39.97545270896702618, -112.6980969099493990, 5.347274454178449155 ) ) ;
#2376 = CARTESIAN_POINT ( 'NONE',  ( 0.000000000000000000, 44.47301969247445186, 16.68249143361927267 ) ) ;
#2377 = CARTESIAN_POINT ( 'NONE',  ( 7.999999999999992895, -40.47821179127737423, 32.64221760512746329 ) ) ;
#2378 = ORIENTED_EDGE ( 'NONE', *, *, #7347, .T. ) ;
#2379 = ORIENTED_EDGE ( 'NONE', *, *, #3575, .F. ) ;
#2380 = CARTESIAN_POINT ( 'NONE',  ( 70.00001200000004076, -24.93377057609608372, 88.89589070667321380 ) ) ;
#2381 = EDGE_CURVE ( 'NONE', #19761, #12261, #3715, .T. ) ;
#2382 = CIRCLE ( 'NONE', #22462, 22.00000000000000000 ) ;
#2383 =( GEOMETRIC_REPRESENTATION_CONTEXT ( 3 ) GLOBAL_UNCERTAINTY_ASSIGNED_CONTEXT ( ( #20016 ) ) GLOBAL_UNIT_ASSIGNED_CONTEXT ( ( #33391, #27658, #14121 ) ) REPRESENTATION_CONTEXT ( 'NONE', 'WORKASPACE' ) );
#2384 = CIRCLE ( 'NONE', #29383, 47.49900000000002365 ) ;
#2385 = CYLINDRICAL_SURFACE ( 'NONE', #21308, 6.000000000000005329 ) ;
#2386 = EDGE_LOOP ( 'NONE', ( #30983, #31580, #18187, #1336 ) ) ;
#2387 = ORIENTED_EDGE ( 'NONE', *, *, #33522, .F. ) ;
#2388 = CARTESIAN_POINT ( 'NONE',  ( -34.50000000000000000, -112.5389594332240222, 2.818899826424027477 ) ) ;
#2389 = DIRECTION ( 'NONE',  ( -0.000000000000000000, 0.000000000000000000, -1.000000000000000000 ) ) ;
#2390 = ORIENTED_EDGE ( 'NONE', *, *, #3525, .T. ) ;
#2391 = CARTESIAN_POINT ( 'NONE',  ( 8.000000000000000000, 11.06713717293261467, -13.55483219355716606 ) ) ;
#2392 = CARTESIAN_POINT ( 'NONE',  ( -34.50000000000000000, -113.9929510916434339, 10.50625754673587409 ) ) ;
#2393 = CARTESIAN_POINT ( 'NONE',  ( -1.387778780781445676E-14, 0.4273491293403097746, 0.000000000000000000 ) ) ;
#2394 = CIRCLE ( 'NONE', #19595, 4.000000000000000000 ) ;
#2395 = CYLINDRICAL_SURFACE ( 'NONE', #17961, 0.5000000000000004441 ) ;
#2396 = CARTESIAN_POINT ( 'NONE',  ( -37.46093750000000711, -113.9929510916434339, 13.11852480586264846 ) ) ;
#2397 = CARTESIAN_POINT ( 'NONE',  ( -37.99999897736217491, -115.9929510916434481, 12.62466071271733092 ) ) ;
#2398 = DIRECTION ( 'NONE',  ( 0.000000000000000000, 0.000000000000000000, -1.000000000000000000 ) ) ;
#2399 = FACE_OUTER_BOUND ( 'NONE', #21454, .T. ) ;
#2400 = VERTEX_POINT ( 'NONE', #31264 ) ;
#2401 = VECTOR ( 'NONE', #34422, 1000.000000000000000 ) ;
#2402 =( GEOMETRIC_REPRESENTATION_CONTEXT ( 3 ) GLOBAL_UNCERTAINTY_ASSIGNED_CONTEXT ( ( #2802 ) ) GLOBAL_UNIT_ASSIGNED_CONTEXT ( ( #29781, #13389, #18603 ) ) REPRESENTATION_CONTEXT ( 'NONE', 'WORKASPACE' ) );
#2403 = DIRECTION ( 'NONE',  ( 0.000000000000000000, -2.775557561562888984E-15, 1.000000000000000000 ) ) ;
#2404 = LINE ( 'NONE', #13020, #8767 ) ;
#2405 = LINE ( 'NONE', #13372, #28354 ) ;
#2406 = VERTEX_POINT ( 'NONE', #3727 ) ;
#2407 = DIRECTION ( 'NONE',  ( 1.226634733346697831E-16, -0.9659258262890715319, 0.2588190451025083605 ) ) ;
#2408 = EDGE_CURVE ( 'NONE', #7160, #28086, #34768, .T. ) ;
#2409 = CARTESIAN_POINT ( 'NONE',  ( -35.50000000000000000, -113.0140978167138712, 0.8752176474015934682 ) ) ;
#2410 = PLANE ( 'NONE',  #29969 ) ;
#2411 = EDGE_CURVE ( 'NONE', #26625, #9040, #7308, .T. ) ;
#2412 = CARTESIAN_POINT ( 'NONE',  ( -35.50000000000000711, -114.9929510916434339, 10.52000928670414126 ) ) ;
#2413 = CARTESIAN_POINT ( 'NONE',  ( 65.00000000000001421, -25.98076211353320986, 88.99999999999994316 ) ) ;
#2414 = ORIENTED_EDGE ( 'NONE', *, *, #14799, .T. ) ;
#2415 = DIRECTION ( 'NONE',  ( -1.047965281155519913E-16, -6.938893903907192632E-17, -1.000000000000000000 ) ) ;
#2416 = CARTESIAN_POINT ( 'NONE',  ( -35.50000000000000000, -111.0140978167138570, -0.3122823525984338988 ) ) ;
#2417 = ORIENTED_EDGE ( 'NONE', *, *, #6, .F. ) ;
#2418 = VERTEX_POINT ( 'NONE', #34686 ) ;
#2419 = CARTESIAN_POINT ( 'NONE',  ( -38.45611840935523418, -115.3723087153909432, 2.066024454178448710 ) ) ;
#2420 = ADVANCED_FACE ( 'NONE', ( #12719 ), #15748, .T. ) ;
#2421 = DIRECTION ( 'NONE',  ( 0.000000000000000000, 0.000000000000000000, -1.000000000000000000 ) ) ;
#2422 = ORIENTED_EDGE ( 'NONE', *, *, #31724, .F. ) ;
#2423 = ORIENTED_EDGE ( 'NONE', *, *, #24195, .T. ) ;
#2424 = CARTESIAN_POINT ( 'NONE',  ( -34.50000000000000000, -113.0140978167138712, 0.8127176474015720409 ) ) ;
#2425 = CARTESIAN_POINT ( 'NONE',  ( 4.000000000000000000, 19.77827456857338007, -2.969824084036535528 ) ) ;
#2426 = AXIS2_PLACEMENT_3D ( 'NONE', #4905, #31716, #7048 ) ;
#2427 = AXIS2_PLACEMENT_3D ( 'NONE', #25707, #6783, #31624 ) ;
#2428 = DIRECTION ( 'NONE',  ( 0.000000000000000000, -0.7705132427757949154, 0.6374239897486828621 ) ) ;
#2429 = DIRECTION ( 'NONE',  ( 0.000000000000000000, 0.000000000000000000, -1.000000000000000000 ) ) ;
#2430 = CARTESIAN_POINT ( 'NONE',  ( -37.53269373325071712, -114.9929510916434339, 13.11752178341324360 ) ) ;
#2431 = CYLINDRICAL_SURFACE ( 'NONE', #25329, 4.980000000000017302 ) ;
#2432 = CARTESIAN_POINT ( 'NONE',  ( -4.000000000000000000, 0.000000000000000000, -40.89999999999999858 ) ) ;
#2433 = CARTESIAN_POINT ( 'NONE',  ( -34.50000000000000000, -115.1446187476384040, -1.616767172155725740 ) ) ;
#2434 = ADVANCED_FACE ( 'NONE', ( #24236 ), #21335, .T. ) ;
#2435 = CARTESIAN_POINT ( 'NONE',  ( 8.000000000000000000, 12.96676809804150565, 13.60411018104323411 ) ) ;
#2436 = AXIS2_PLACEMENT_3D ( 'NONE', #26748, #31599, #6753 ) ;
#2437 = CARTESIAN_POINT ( 'NONE',  ( 0.000000000000000000, 0.000000000000000000, 0.000000000000000000 ) ) ;
#2438 = ORIENTED_EDGE ( 'NONE', *, *, #30780, .T. ) ;
#2439 = CARTESIAN_POINT ( 'NONE',  ( -38.00000000000000711, -115.9929510916434481, 11.21034663311206181 ) ) ;
#2440 = CARTESIAN_POINT ( 'NONE',  ( 2.000000000000002665, 1.462249188368523427E-15, 7.800000000000023803 ) ) ;
#2441 = CARTESIAN_POINT ( 'NONE',  ( 0.000000000000000000, 24.72041153920734047, 40.55929306992698002 ) ) ;
#2442 = LINE ( 'NONE', #10894, #13963 ) ;
#2443 = DIRECTION ( 'NONE',  ( 5.339440136655842133E-16, 1.000000000000000000, -1.918536189538073087E-16 ) ) ;
#2444 = ORIENTED_EDGE ( 'NONE', *, *, #21190, .T. ) ;
#2445 = DIRECTION ( 'NONE',  ( -1.000000000000000000, 0.000000000000000000, 0.000000000000000000 ) ) ;
#2446 = LINE ( 'NONE', #21493, #310 ) ;
#2447 = EDGE_CURVE ( 'NONE', #26362, #542, #27119, .T. ) ;
#2448 = DIRECTION ( 'NONE',  ( -1.000000000000000000, 0.000000000000000000, 0.000000000000000000 ) ) ;
#2449 = CARTESIAN_POINT ( 'NONE',  ( 1.498621416870293155, -4.936931676003361682E-14, -7.020000000000020890 ) ) ;
#2450 = ADVANCED_FACE ( 'NONE', ( #15932 ), #18461, .T. ) ;
#2451 = EDGE_CURVE ( 'NONE', #9311, #26508, #15764, .T. ) ;
#2452 = CIRCLE ( 'NONE', #16207, 4.800000000000006040 ) ;
#2453 = DIRECTION ( 'NONE',  ( 0.000000000000000000, 0.000000000000000000, 1.000000000000000000 ) ) ;
#2454 = CARTESIAN_POINT ( 'NONE',  ( 50.00000000000000711, 0.000000000000000000, -5.000000000000011546 ) ) ;
#2455 = EDGE_LOOP ( 'NONE', ( #24664, #34048, #10957, #30998 ) ) ;
#2456 = VERTEX_POINT ( 'NONE', #10009 ) ;
#2457 = DIRECTION ( 'NONE',  ( -1.000000000000000000, 0.000000000000000000, 0.000000000000000000 ) ) ;
#2458 = FACE_OUTER_BOUND ( 'NONE', #27702, .T. ) ;
#2459 = DIRECTION ( 'NONE',  ( -1.000000000000000000, -0.000000000000000000, 0.000000000000000000 ) ) ;
#2460 = EDGE_LOOP ( 'NONE', ( #26962, #477, #20585, #28253 ) ) ;
#2461 = CARTESIAN_POINT ( 'NONE',  ( -39.02454729103295961, -113.2308352781851539, 4.840225545821551734 ) ) ;
#2462 = EDGE_CURVE ( 'NONE', #20834, #17030, #15565, .T. ) ;
#2463 = ORIENTED_EDGE ( 'NONE', *, *, #5481, .F. ) ;
#2464 = EDGE_CURVE ( 'NONE', #23346, #16643, #4977, .T. ) ;
#2466 = ORIENTED_EDGE ( 'NONE', *, *, #33726, .F. ) ;
#2465 = CIRCLE ( 'NONE', #13931, 4.000000000000000000 ) ;
#2467 = VERTEX_POINT ( 'NONE', #32694 ) ;
#2468 = CARTESIAN_POINT ( 'NONE',  ( 8.000000000000000000, -18.62763138773852134, 2.494040418455287345 ) ) ;
#2469 = DIRECTION ( 'NONE',  ( -1.000000000000000000, 0.000000000000000000, -0.000000000000000000 ) ) ;
#2470 = ORIENTED_EDGE ( 'NONE', *, *, #22024, .F. ) ;
#2471 = ORIENTED_EDGE ( 'NONE', *, *, #34763, .F. ) ;
#2472 = DIRECTION ( 'NONE',  ( 0.000000000000000000, 1.000000000000000000, 3.491564676272318479E-15 ) ) ;
#2473 = AXIS2_PLACEMENT_3D ( 'NONE', #11702, #11181, #32975 ) ;
#2474 = DIRECTION ( 'NONE',  ( 0.000000000000000000, 0.000000000000000000, -1.000000000000000000 ) ) ;
#2475 = CIRCLE ( 'NONE', #30621, 22.00000000000000000 ) ;
#2476 = CARTESIAN_POINT ( 'NONE',  ( 3.999999999999996447, 21.63912866391145684, -3.968388925834583247 ) ) ;
#2477 = EDGE_CURVE ( 'NONE', #27617, #14457, #18543, .T. ) ;
#2478 = CARTESIAN_POINT ( 'NONE',  ( 1.566204647097418912, -6.822536405429468154, -0.7999999999999951594 ) ) ;
#2479 = CARTESIAN_POINT ( 'NONE',  ( -1.387778780781445676E-14, 0.4273491293403097746, -0.7999999999999951594 ) ) ;
#2480 = PRODUCT_RELATED_PRODUCT_CATEGORY ( 'part', '', ( #31947 ) ) ;
#2481 = CARTESIAN_POINT ( 'NONE',  ( -36.23083527818513261, -116.0245472910329880, 3.284774454178449155 ) ) ;
#2482 = EDGE_CURVE ( 'NONE', #16891, #15563, #13430, .T. ) ;
#2483 = CARTESIAN_POINT ( 'NONE',  ( -37.37500000000009237, -115.9929510916434481, 14.11852480586265024 ) ) ;
#2484 = CARTESIAN_POINT ( 'NONE',  ( -21.15833593587365513, -27.48076211353304998, 70.99999999999988631 ) ) ;
#2485 = DIRECTION ( 'NONE',  ( -1.000000000000000000, 0.000000000000000000, 0.000000000000000000 ) ) ;
#2486 = CIRCLE ( 'NONE', #34683, 0.7500000000000006661 ) ;
#2487 = CIRCLE ( 'NONE', #15659, 20.00000000000000355 ) ;
#2488 = CARTESIAN_POINT ( 'NONE',  ( 7.999999999999992895, -24.72041153920704915, -40.55929306992714345 ) ) ;
#2489 = DIRECTION ( 'NONE',  ( 0.02857142857142376188, 0.9995917534020517525, 3.884870526907702978E-16 ) ) ;
#2490 = CYLINDRICAL_SURFACE ( 'NONE', #936, 11.00000000000000000 ) ;
#2491 = EDGE_LOOP ( 'NONE', ( #14434, #3402, #29476, #33688 ) ) ;
#2492 = EDGE_CURVE ( 'NONE', #8765, #31548, #12899, .T. ) ;
#2493 = ADVANCED_FACE ( 'NONE', ( #24411 ), #35398, .T. ) ;
#2494 = CARTESIAN_POINT ( 'NONE',  ( -36.11231047232249125, -115.9754527089670262, 4.277725545821551734 ) ) ;
#2495 = DIRECTION ( 'NONE',  ( -1.783119874454246424E-31, -1.187911941725854497E-31, 1.000000000000000000 ) ) ;
#2496 = CARTESIAN_POINT ( 'NONE',  ( -55.00000000000000000, 19.99999999999998934, 120.0000000000000000 ) ) ;
#2497 = CARTESIAN_POINT ( 'NONE',  ( 70.00000000000001421, -29.60243954609234507, 93.25429903592612391 ) ) ;
#2498 = VERTEX_POINT ( 'NONE', #32328 ) ;
#2499 = ORIENTED_EDGE ( 'NONE', *, *, #4647, .T. ) ;
#2500 = AXIS2_PLACEMENT_3D ( 'NONE', #4387, #17693, #18044 ) ;
#2501 = SURFACE_SIDE_STYLE ('',( #10769 ) ) ;
#2502 = VECTOR ( 'NONE', #35296, 1000.000000000000000 ) ;
#2503 = CARTESIAN_POINT ( 'NONE',  ( 0.000000000000000000, -30.93515269692138503, 36.04401931830242489 ) ) ;
#2504 = VERTEX_POINT ( 'NONE', #21694 ) ;
#2505 = AXIS2_PLACEMENT_3D ( 'NONE', #32867, #8544, #33045 ) ;
#2506 = EDGE_LOOP ( 'NONE', ( #10673, #1199, #407, #34930 ) ) ;
#2507 = EDGE_CURVE ( 'NONE', #26405, #1934, #8015, .T. ) ;
#2508 = CARTESIAN_POINT ( 'NONE',  ( 0.000000000000000000, 14.48509162075963985, 8.733917826871412160 ) ) ;
#2509 = CARTESIAN_POINT ( 'NONE',  ( -50.00000000000000000, 19.99999999999998934, 120.0000000000000000 ) ) ;
#2510 = CARTESIAN_POINT ( 'NONE',  ( 70.00000000000001421, -25.98076211353321341, 84.99999999999994316 ) ) ;
#2511 = CARTESIAN_POINT ( 'NONE',  ( 7.999999999999992895, -45.78515115856034612, -12.64416602183715455 ) ) ;
#2512 = ORIENTED_EDGE ( 'NONE', *, *, #15046, .T. ) ;
#2513 = ORIENTED_EDGE ( 'NONE', *, *, #34592, .F. ) ;
#2514 = CIRCLE ( 'NONE', #23173, 20.00000000000000711 ) ;
#2515 = CARTESIAN_POINT ( 'NONE',  ( -35.50000000000000711, -112.9185811467682754, 1.870920967077121411 ) ) ;
#2516 = CARTESIAN_POINT ( 'NONE',  ( 7.999999999999992895, 34.03046037009305280, -33.13733193845769165 ) ) ;
#2517 = DIRECTION ( 'NONE',  ( -1.000000000000000000, 0.000000000000000000, 0.000000000000000000 ) ) ;
#2518 = ORIENTED_EDGE ( 'NONE', *, *, #16282, .T. ) ;
#2519 = CARTESIAN_POINT ( 'NONE',  ( -2.600000000000004530, -12.74999999999999822, -1.200000000000006617 ) ) ;
#2520 = EDGE_CURVE ( 'NONE', #32530, #7199, #35056, .T. ) ;
#2521 = CARTESIAN_POINT ( 'NONE',  ( -34.50000000000000000, -112.0140978167138712, -0.1247823525984259746 ) ) ;
#2523 = EDGE_CURVE ( 'NONE', #4350, #6950, #13086, .T. ) ;
#2522 = APPLICATION_CONTEXT ( 'automotive_design' ) ;
#2524 = CIRCLE ( 'NONE', #24921, 7.199999999999998401 ) ;
#2525 = CARTESIAN_POINT ( 'NONE',  ( -37.59808119975203766, -114.9929510916434339, 14.11551573851448893 ) ) ;
#2526 = AXIS2_PLACEMENT_3D ( 'NONE', #11105, #13623, #8039 ) ;
#2527 = EDGE_CURVE ( 'NONE', #10299, #10915, #31973, .T. ) ;
#2528 = CARTESIAN_POINT ( 'NONE',  ( 5.400000000000085620, -1.000000000000049516, -32.00000000000000000 ) ) ;
#2529 = CARTESIAN_POINT ( 'NONE',  ( -38.00000000000000711, -114.9929510916434339, 12.56351784598954779 ) ) ;
#2530 = CARTESIAN_POINT ( 'NONE',  ( -42.49999999999999289, -29.98076211353323828, 83.49999999999990052 ) ) ;
#2531 = CARTESIAN_POINT ( 'NONE',  ( -34.50000000000000000, -114.9929510916434339, 10.85830208992344303 ) ) ;
#2532 = CARTESIAN_POINT ( 'NONE',  ( 8.000000000000000000, -21.63912866391137513, -3.968388925835035330 ) ) ;
#2533 = DIRECTION ( 'NONE',  ( 0.000000000000000000, -1.000000000000000000, 0.000000000000000000 ) ) ;
#2534 = ORIENTED_EDGE ( 'NONE', *, *, #1620, .T. ) ;
#2535 = CARTESIAN_POINT ( 'NONE',  ( 0.9999999999999870104, -5.408326913195881325, 0.000000000000000000 ) ) ;
#2536 = FACE_OUTER_BOUND ( 'NONE', #20607, .T. ) ;
#2537 = ORIENTED_EDGE ( 'NONE', *, *, #1089, .T. ) ;
#2538 = CARTESIAN_POINT ( 'NONE',  ( -35.97955704204053262, -114.9929510916434339, 13.11812344617474579 ) ) ;
#2539 = VERTEX_POINT ( 'NONE', #32154 ) ;
#2540 = ADVANCED_FACE ( 'NONE', ( #10376 ), #24072, .F. ) ;
#2541 = CARTESIAN_POINT ( 'NONE',  ( -37.76916472181487450, -111.9754527089670404, 8.534774454178448266 ) ) ;
#2542 = ADVANCED_FACE ( 'NONE', ( #25294 ), #5851, .T. ) ;
#2543 = FACE_OUTER_BOUND ( 'NONE', #19549, .T. ) ;
#2544 = VERTEX_POINT ( 'NONE', #5505 ) ;
#2545 = CIRCLE ( 'NONE', #18605, 3.799999999999999822 ) ;
#2546 = ORIENTED_EDGE ( 'NONE', *, *, #31900, .T. ) ;
#2547 = AXIS2_PLACEMENT_3D ( 'NONE', #16252, #21483, #32476 ) ;
#2548 = CARTESIAN_POINT ( 'NONE',  ( 8.000000000000007105, -9.919332006307138627, -5.363026430117212584 ) ) ;
#2549 = CARTESIAN_POINT ( 'NONE',  ( 7.999999999999992895, 36.06787431788733045, -37.45808914225451502 ) ) ;
#2550 = ORIENTED_EDGE ( 'NONE', *, *, #33478, .T. ) ;
#2551 = CARTESIAN_POINT ( 'NONE',  ( -35.69809690994938478, -111.0245472910330022, 7.222274454178449155 ) ) ;
#2552 = DIRECTION ( 'NONE',  ( -1.000000000000000000, 0.000000000000000000, 0.000000000000000000 ) ) ;
#2553 = AXIS2_PLACEMENT_3D ( 'NONE', #1831, #9562, #20530 ) ;
#2554 = CARTESIAN_POINT ( 'NONE',  ( -35.50000000000000711, -116.0140978167138712, -0.3747823525984422255 ) ) ;
#2555 = AXIS2_PLACEMENT_3D ( 'NONE', #6224, #11791, #31419 ) ;
#2556 = ORIENTED_EDGE ( 'NONE', *, *, #17988, .F. ) ;
#2557 = VERTEX_POINT ( 'NONE', #8359 ) ;
#2558 = CYLINDRICAL_SURFACE ( 'NONE', #34939, 4.800000000000000711 ) ;
#2559 = SHAPE_REPRESENTATION_RELATIONSHIP ( 'NONE' , 'NONE' ,  #5681, #8640 ) ;
#2560 = CARTESIAN_POINT ( 'NONE',  ( 0.000000000000000000, -5.363026430117032284, -9.919332006307277183 ) ) ;
#2561 = ORIENTED_EDGE ( 'NONE', *, *, #28176, .F. ) ;
#2562 = ORIENTED_EDGE ( 'NONE', *, *, #10206, .T. ) ;
#2563 = CARTESIAN_POINT ( 'NONE',  ( -34.50000000000000000, -113.1807644833805426, -2.624782352598442614 ) ) ;
#2564 = DIRECTION ( 'NONE',  ( 0.000000000000000000, -0.5877852522924620349, -0.8090169943749554449 ) ) ;
#2565 = VERTEX_POINT ( 'NONE', #27993 ) ;
#2566 = CARTESIAN_POINT ( 'NONE',  ( -35.50000000000000711, -114.9929510916434339, 10.94631322572069365 ) ) ;
#2567 = ADVANCED_FACE ( 'NONE', ( #19515 ), #22569, .T. ) ;
#2568 = CARTESIAN_POINT ( 'NONE',  ( -35.61121590948313553, -113.9929510916434339, 14.07058620477040733 ) ) ;
#2569 = CARTESIAN_POINT ( 'NONE',  ( 65.00000000000001421, 75.33903961282865680, 25.84872029956372330 ) ) ;
#2570 = DIRECTION ( 'NONE',  ( 1.000000000000000000, -0.000000000000000000, 0.000000000000000000 ) ) ;
#2571 = CARTESIAN_POINT ( 'NONE',  ( -37.46874999999995737, -113.9929510916434339, 13.11852480586264846 ) ) ;
#2572 = CARTESIAN_POINT ( 'NONE',  ( -35.50000000000000711, -114.9929510916434339, 10.53376102667243508 ) ) ;
#2573 = DIRECTION ( 'NONE',  ( 1.047965281155515106E-16, -6.938893903907203726E-17, -1.000000000000000000 ) ) ;
#2574 =( REPRESENTATION_RELATIONSHIP ('NONE','NONE', #26607, #2005 ) REPRESENTATION_RELATIONSHIP_WITH_TRANSFORMATION ( #23096 )SHAPE_REPRESENTATION_RELATIONSHIP( ) );
#2576 = AXIS2_PLACEMENT_3D ( 'NONE', #11160, #33643, #875 ) ;
#2575 = CARTESIAN_POINT ( 'NONE',  ( 7.999999999999992895, 50.95304419620825342, 10.38206564895680017 ) ) ;
#2577 = CIRCLE ( 'NONE', #22079, 52.00000000000000711 ) ;
#2578 = VERTEX_POINT ( 'NONE', #3343 ) ;
#2579 = CARTESIAN_POINT ( 'NONE',  ( -3.799999999999999822, 4.653657836759942730E-16, 49.10000000000000142 ) ) ;
#2580 = DIRECTION ( 'NONE',  ( 1.000000000000000000, -5.339440136655834244E-16, 0.000000000000000000 ) ) ;
#2581 = CARTESIAN_POINT ( 'NONE',  ( 4.000000000000000000, -6.359167119270592750, 18.96209359615092183 ) ) ;
#2582 = CIRCLE ( 'NONE', #29610, 4.000000000000000000 ) ;
#2583 = EDGE_LOOP ( 'NONE', ( #34138, #24817, #3479, #17301 ) ) ;
#2584 = CARTESIAN_POINT ( 'NONE',  ( 8.000000000000007105, 0.3151488735048668666, 11.27190672109269798 ) ) ;
#2585 = ORIENTED_EDGE ( 'NONE', *, *, #25973, .T. ) ;
#2586 = CARTESIAN_POINT ( 'NONE',  ( -35.50000000000000711, -116.0140978167138712, -0.4685323525984310677 ) ) ;
#2587 = FACE_OUTER_BOUND ( 'NONE', #19208, .T. ) ;
#2588 = CARTESIAN_POINT ( 'NONE',  ( -35.50000000000000711, -114.9912366357066986, 10.44580456020104720 ) ) ;
#2589 = CARTESIAN_POINT ( 'NONE',  ( 8.000000000000007105, 5.363026430117226795, 9.919332006307262972 ) ) ;
#2590 = ORIENTED_EDGE ( 'NONE', *, *, #20513, .T. ) ;
#2591 = CARTESIAN_POINT ( 'NONE',  ( 2.000000000000002665, -4.771817072227797033E-14, 6.765000000000020997 ) ) ;
#2592 = CARTESIAN_POINT ( 'NONE',  ( -35.50000000000000000, -111.6790780953339066, 2.383953864837686343 ) ) ;
#2593 = ORIENTED_EDGE ( 'NONE', *, *, #13307, .T. ) ;
#2594 = ORIENTED_EDGE ( 'NONE', *, *, #8316, .F. ) ;
#2595 = CARTESIAN_POINT ( 'NONE',  ( -35.62769128460905677, -115.4561184093552413, 3.191024454178449155 ) ) ;
#2596 = CARTESIAN_POINT ( 'NONE',  ( 1.599999999999990985, -4.871103520542888323E-16, -7.020000000000045759 ) ) ;
#2597 = ORIENTED_EDGE ( 'NONE', *, *, #11936, .T. ) ;
#2598 = ORIENTED_EDGE ( 'NONE', *, *, #28445, .F. ) ;
#2599 = CARTESIAN_POINT ( 'NONE',  ( -34.50000000000000000, -114.1807644833817648, -0.6247823525984269599 ) ) ;
#2600 = DIRECTION ( 'NONE',  ( 1.000000000000000000, -5.339440136655842133E-16, -1.047965281155519420E-16 ) ) ;
#2601 = CIRCLE ( 'NONE', #26731, 7.199999999999998401 ) ;
#2602 = CIRCLE ( 'NONE', #11188, 14.00000000000000000 ) ;
#2603 = DIRECTION ( 'NONE',  ( -0.000000000000000000, 0.000000000000000000, -1.000000000000000000 ) ) ;
#2604 = AXIS2_PLACEMENT_3D ( 'NONE', #21534, #4497, #31827 ) ;
#2605 = CARTESIAN_POINT ( 'NONE',  ( 0.000000000000000000, -49.65209126885775248, 15.44894276735533900 ) ) ;
#2606 = ADVANCED_FACE ( 'NONE', ( #8190 ), #11596, .T. ) ;
#2607 = CARTESIAN_POINT ( 'NONE',  ( -35.50000000000000000, -113.9929510916430075, 10.50625754673586876 ) ) ;
#2608 = CARTESIAN_POINT ( 'NONE',  ( -3.799999999999999822, 0.000000000000000000, -33.50000000000000711 ) ) ;
#2609 = DIRECTION ( 'NONE',  ( -1.000000000000000000, 0.000000000000000000, 0.000000000000000000 ) ) ;
#2610 = CARTESIAN_POINT ( 'NONE',  ( -34.50000000000000000, -112.7549084230351752, -1.592823285203595285 ) ) ;
#2611 = CARTESIAN_POINT ( 'NONE',  ( -36.99999999999988631, -115.9929510916434481, 14.11852480586265024 ) ) ;
#2612 = AXIS2_PLACEMENT_3D ( 'NONE', #30286, #27413, #19276 ) ;
#2613 = DIRECTION ( 'NONE',  ( -1.000000000000000000, 0.000000000000000000, 0.000000000000000000 ) ) ;
#2614 = DIRECTION ( 'NONE',  ( -0.000000000000000000, 0.2538061376417689585, 0.9672551082808338307 ) ) ;
#2615 = VERTEX_POINT ( 'NONE', #16277 ) ;
#2616 = EDGE_CURVE ( 'NONE', #34867, #19376, #7075, .T. ) ;
#2617 = CARTESIAN_POINT ( 'NONE',  ( -38.00000000000000711, -115.9929510916434481, 12.53051367006571937 ) ) ;
#2618 = DIRECTION ( 'NONE',  ( 1.000000000000000000, -0.000000000000000000, -0.000000000000000000 ) ) ;
#2619 = FILL_AREA_STYLE_COLOUR ( '', #3610 ) ;
#2620 = DIRECTION ( 'NONE',  ( -1.000000000000000000, 0.000000000000000000, 0.000000000000000000 ) ) ;
#2621 = DIRECTION ( 'NONE',  ( -1.000000000000000000, 0.000000000000000000, 0.000000000000000000 ) ) ;
#2622 = ORIENTED_EDGE ( 'NONE', *, *, #16268, .T. ) ;
#2623 = DIRECTION ( 'NONE',  ( -1.000000000000000000, 0.000000000000000000, 0.000000000000000000 ) ) ;
#2624 = DIRECTION ( 'NONE',  ( -1.000000000000000000, 0.000000000000000000, 0.000000000000000000 ) ) ;
#2625 = VECTOR ( 'NONE', #16350, 1000.000000000000000 ) ;
#2626 = AXIS2_PLACEMENT_3D ( 'NONE', #1543, #3714, #11994 ) ;
#2627 = DIRECTION ( 'NONE',  ( 1.000000000000000000, -0.000000000000000000, -0.000000000000000000 ) ) ;
#2628 = LINE ( 'NONE', #10536, #17242 ) ;
#2629 = DIRECTION ( 'NONE',  ( -1.000000000000000000, -1.836970198721029934E-16, -0.000000000000000000 ) ) ;
#2630 = CARTESIAN_POINT ( 'NONE',  ( 0.000000000000000000, -46.90537658765333617, 2.727856614654147638 ) ) ;
#2631 = AXIS2_PLACEMENT_3D ( 'NONE', #9421, #6368, #23097 ) ;
#2632 = ORIENTED_EDGE ( 'NONE', *, *, #28492, .T. ) ;
#2633 = ORIENTED_EDGE ( 'NONE', *, *, #13327, .T. ) ;
#2634 = AXIS2_PLACEMENT_3D ( 'NONE', #1034, #14505, #834 ) ;
#2635 = CARTESIAN_POINT ( 'NONE',  ( 0.000000000000000000, -35.11945359308137427, 38.34871548466002622 ) ) ;
#2636 = CYLINDRICAL_SURFACE ( 'NONE', #35102, 5.000000000000004441 ) ;
#2637 = CYLINDRICAL_SURFACE ( 'NONE', #11671, 8.000000000000001776 ) ;
#2638 = ORIENTED_EDGE ( 'NONE', *, *, #16294, .T. ) ;
#2639 = CARTESIAN_POINT ( 'NONE',  ( -35.62769128460905677, -112.5438815906447729, 8.308975545821549957 ) ) ;
#2640 = ORIENTED_EDGE ( 'NONE', *, *, #29026, .T. ) ;
#2641 =( NAMED_UNIT ( * ) SI_UNIT ( $, .STERADIAN. ) SOLID_ANGLE_UNIT ( ) );
#2642 = CIRCLE ( 'NONE', #10670, 52.00000000000000711 ) ;
#2643 = ORIENTED_EDGE ( 'NONE', *, *, #33970, .T. ) ;
#2644 = ORIENTED_EDGE ( 'NONE', *, *, #496, .F. ) ;
#2645 = CARTESIAN_POINT ( 'NONE',  ( 2.000000000000002220, 4.434986294202125852E-16, 4.724999999999999645 ) ) ;
#2646 = DIRECTION ( 'NONE',  ( -1.000000000000000000, 0.000000000000000000, 0.000000000000000000 ) ) ;
#2647 = EDGE_LOOP ( 'NONE', ( #29100, #1130, #4213, #18407 ) ) ;
#2648 = ORIENTED_EDGE ( 'NONE', *, *, #32954, .F. ) ;
#2649 = ADVANCED_FACE ( 'NONE', ( #30519 ), #2637, .T. ) ;
#2650 = VECTOR ( 'NONE', #31959, 1000.000000000000000 ) ;
#2651 = CARTESIAN_POINT ( 'NONE',  ( 7.999999999999992895, 46.87740477351712798, 3.172455868806031809 ) ) ;
#2652 = CARTESIAN_POINT ( 'NONE',  ( 8.000000000000000000, 0.000000000000000000, 0.000000000000000000 ) ) ;
#2653 = EDGE_CURVE ( 'NONE', #17256, #16010, #11249, .T. ) ;
#2654 = FACE_OUTER_BOUND ( 'NONE', #14905, .T. ) ;
#2655 = CIRCLE ( 'NONE', #7232, 4.000000000000003553 ) ;
#2656 = AXIS2_PLACEMENT_3D ( 'NONE', #3682, #14632, #19675 ) ;
#2657 = CARTESIAN_POINT ( 'NONE',  ( -34.49999999999998579, -36.56745899286261192, 82.16330312067040609 ) ) ;
#2658 = CARTESIAN_POINT ( 'NONE',  ( 8.000000000000007105, 5.908880290975540461, 9.604183132802438294 ) ) ;
#2659 = FACE_OUTER_BOUND ( 'NONE', #8842, .T. ) ;
#2660 = EDGE_CURVE ( 'NONE', #15153, #17557, #13600, .T. ) ;
#2661 = CARTESIAN_POINT ( 'NONE',  ( -38.95206139890799335, -115.9929510916434481, 13.00730889637963550 ) ) ;
#2662 = DIRECTION ( 'NONE',  ( -1.000000000000000000, -0.000000000000000000, 0.000000000000000000 ) ) ;
#2663 = EDGE_CURVE ( 'NONE', #3203, #18596, #9362, .T. ) ;
#2664 = CYLINDRICAL_SURFACE ( 'NONE', #12460, 45.00000000000000000 ) ;
#2665 = AXIS2_PLACEMENT_3D ( 'NONE', #16709, #18893, #16351 ) ;
#2666 = LINE ( 'NONE', #19195, #34893 ) ;
#2667 = CYLINDRICAL_SURFACE ( 'NONE', #18683, 4.800000000000000711 ) ;
#2668 = LINE ( 'NONE', #30545, #14166 ) ;
#2669 = DIRECTION ( 'NONE',  ( 0.000000000000000000, 0.000000000000000000, 1.000000000000000000 ) ) ;
#2670 = EDGE_LOOP ( 'NONE', ( #20970, #14422, #16376, #5466, #10981, #179, #16771, #20477, #24151, #2069 ) ) ;
#2671 = CARTESIAN_POINT ( 'NONE',  ( -36.52652403469559061, -114.9754527089670262, 4.277725545821552622 ) ) ;
#2672 = CARTESIAN_POINT ( 'NONE',  ( 50.00005079999999680, 4.898587196589412829E-16, -4.000000000000000000 ) ) ;
#2673 = LINE ( 'NONE', #27156, #7841 ) ;
#2674 = LINE ( 'NONE', #29500, #397 ) ;
#2675 = VERTEX_POINT ( 'NONE', #27479 ) ;
#2676 = VERTEX_POINT ( 'NONE', #2825 ) ;
#2678 = LINE ( 'NONE', #13302, #14269 ) ;
#2677 = PRODUCT_DEFINITION_SHAPE ( 'NONE', 'NONE',  #35639 ) ;
#2679 = AXIS2_PLACEMENT_3D ( 'NONE', #9068, #15159, #17327 ) ;
#2680 = CYLINDRICAL_SURFACE ( 'NONE', #5442, 20.00000000000000711 ) ;
#2681 = VERTEX_POINT ( 'NONE', #10910 ) ;
#2682 = ORIENTED_EDGE ( 'NONE', *, *, #27285, .T. ) ;
#2683 = AXIS2_PLACEMENT_3D ( 'NONE', #10663, #10846, #35164 ) ;
#2684 = EDGE_CURVE ( 'NONE', #19439, #23884, #32970, .T. ) ;
#2685 = VECTOR ( 'NONE', #21530, 1000.000000000000000 ) ;
#2686 = CIRCLE ( 'NONE', #22185, 3.799999999999999822 ) ;
#2687 = CARTESIAN_POINT ( 'NONE',  ( -39.49999999999999289, -14.67619866229204284, 93.25874355921412473 ) ) ;
#2688 = CYLINDRICAL_SURFACE ( 'NONE', #1619, 52.00000000000000711 ) ;
#2689 = AXIS2_PLACEMENT_3D ( 'NONE', #10908, #18996, #7832 ) ;
#2690 = LINE ( 'NONE', #11643, #24823 ) ;
#2692 = ORIENTED_EDGE ( 'NONE', *, *, #312, .T. ) ;
#2691 = CIRCLE ( 'NONE', #10149, 0.5000000000000004441 ) ;
#2693 = VERTEX_POINT ( 'NONE', #11083 ) ;
#2694 = EDGE_CURVE ( 'NONE', #3168, #31652, #1932, .T. ) ;
#2695 = DIRECTION ( 'NONE',  ( 1.174092375852890260E-15, -4.222049128630259891E-16, -1.000000000000000000 ) ) ;
#2696 = EDGE_CURVE ( 'NONE', #21748, #18374, #15700, .T. ) ;
#2697 = EDGE_CURVE ( 'NONE', #8613, #11997, #33386, .T. ) ;
#2698 = CARTESIAN_POINT ( 'NONE',  ( 7.999999999999992895, 0.000000000000000000, 0.000000000000000000 ) ) ;
#2699 = ORIENTED_EDGE ( 'NONE', *, *, #1491, .F. ) ;
#2700 = PLANE ( 'NONE',  #25279 ) ;
#2701 = VECTOR ( 'NONE', #3450, 1000.000000000000000 ) ;
#2702 = CARTESIAN_POINT ( 'NONE',  ( -34.50000000000000000, -115.3362660311619692, -1.573728109101206085 ) ) ;
#2703 = CARTESIAN_POINT ( 'NONE',  ( -35.75562914091914024, -114.9929510916434339, 14.09929883582542409 ) ) ;
#2704 = CIRCLE ( 'NONE', #18196, 0.04099999999999937028 ) ;
#2705 = CARTESIAN_POINT ( 'NONE',  ( -35.50000000000000000, -113.9929510916438460, 10.50625754673626133 ) ) ;
#2706 = CARTESIAN_POINT ( 'NONE',  ( -34.49999999999998579, -24.48076211353326315, 88.99999999999994316 ) ) ;
#2707 = CARTESIAN_POINT ( 'NONE',  ( -36.01562499999996447, -114.9929510916434339, 14.11852480586264846 ) ) ;
#2708 = LINE ( 'NONE', #29885, #33163 ) ;
#2709 = PRESENTATION_LAYER_ASSIGNMENT (  '', '', ( #29113 ) ) ;
#2710 = AXIS2_PLACEMENT_3D ( 'NONE', #15922, #29091, #26393 ) ;
#2711 = EDGE_CURVE ( 'NONE', #26583, #1113, #24942, .T. ) ;
#2712 = CARTESIAN_POINT ( 'NONE',  ( 0.000000000000000000, 3.872983346207417021, 0.9999999999999985567 ) ) ;
#2713 = SURFACE_STYLE_USAGE ( .BOTH. , #16349 ) ;
#2714 = DIRECTION ( 'NONE',  ( 0.000000000000000000, 0.000000000000000000, 1.000000000000000000 ) ) ;
#2715 = CIRCLE ( 'NONE', #14726, 52.00000000000000711 ) ;
#2716 = LINE ( 'NONE', #27886, #30807 ) ;
#2717 = CARTESIAN_POINT ( 'NONE',  ( 7.999999999999992895, 47.00885577955422434, -6.806061952191799769 ) ) ;
#2718 = EDGE_LOOP ( 'NONE', ( #11417, #19553, #16467, #11464 ) ) ;
#2719 = CYLINDRICAL_SURFACE ( 'NONE', #32546, 20.00000000000000355 ) ;
#2720 = ORIENTED_EDGE ( 'NONE', *, *, #4952, .T. ) ;
#2721 = CARTESIAN_POINT ( 'NONE',  ( -37.05926240293133134, -116.9999999999999858, 1.878524454178448710 ) ) ;
#2722 = VECTOR ( 'NONE', #8673, 1000.000000000000000 ) ;
#2723 = CARTESIAN_POINT ( 'NONE',  ( 38.00000000000000000, 14.30000000000001492, -3.000000000000002665 ) ) ;
#2724 = VECTOR ( 'NONE', #29273, 1000.000000000000000 ) ;
#2725 = ORIENTED_EDGE ( 'NONE', *, *, #5182, .F. ) ;
#2726 = ORIENTED_EDGE ( 'NONE', *, *, #6928, .F. ) ;
#2727 = DIRECTION ( 'NONE',  ( -1.000000000000000000, 0.000000000000000000, -0.000000000000000000 ) ) ;
#2728 = FACE_BOUND ( 'NONE', #146, .T. ) ;
#2729 = VERTEX_POINT ( 'NONE', #265 ) ;
#2730 = CARTESIAN_POINT ( 'NONE',  ( -39.16322519054179452, -116.0794154965774823, 8.066024454178448266 ) ) ;
#2731 = EDGE_CURVE ( 'NONE', #5795, #2094, #27824, .T. ) ;
#2732 = VECTOR ( 'NONE', #6441, 1000.000000000000000 ) ;
#2733 = DIRECTION ( 'NONE',  ( -1.000000000000000000, 0.000000000000000000, 0.000000000000000000 ) ) ;
#2734 = AXIS2_PLACEMENT_3D ( 'NONE', #30386, #483, #11461 ) ;
#2735 = DIRECTION ( 'NONE',  ( 0.000000000000000000, 0.000000000000000000, -1.000000000000000000 ) ) ;
#2736 = EDGE_LOOP ( 'NONE', ( #16922, #13731, #9263, #6785 ) ) ;
#2738 = ORIENTED_EDGE ( 'NONE', *, *, #27732, .F. ) ;
#2737 = EDGE_CURVE ( 'NONE', #19471, #14555, #13967, .T. ) ;
#2739 = DIRECTION ( 'NONE',  ( -1.000000000000000000, -0.000000000000000000, -0.000000000000000000 ) ) ;
#2740 = VECTOR ( 'NONE', #9136, 1000.000000000000000 ) ;
#2741 = AXIS2_PLACEMENT_3D ( 'NONE', #19253, #30776, #2735 ) ;
#2742 =( NAMED_UNIT ( * ) SI_UNIT ( $, .STERADIAN. ) SOLID_ANGLE_UNIT ( ) );
#2743 = CARTESIAN_POINT ( 'NONE',  ( 0.000000000000000000, -46.11014828289837197, -9.022736828081189486 ) ) ;
#2744 = ORIENTED_EDGE ( 'NONE', *, *, #29021, .F. ) ;
#2745 = ORIENTED_EDGE ( 'NONE', *, *, #4160, .F. ) ;
#2746 = CARTESIAN_POINT ( 'NONE',  ( -34.50000000000000000, -116.6134300264884445, -1.853877267570539944 ) ) ;
#2747 = CIRCLE ( 'NONE', #10168, 15.49900000000000233 ) ;
#2748 = EDGE_CURVE ( 'NONE', #9169, #3468, #3872, .T. ) ;
#2749 = CIRCLE ( 'NONE', #19392, 17.49900000000000233 ) ;
#2750 = DIRECTION ( 'NONE',  ( -1.174092375852890260E-15, 4.222049128630259891E-16, 1.000000000000000000 ) ) ;
#2751 = ORIENTED_EDGE ( 'NONE', *, *, #26717, .T. ) ;
#2752 = EDGE_CURVE ( 'NONE', #17749, #32986, #9426, .T. ) ;
#2753 = CARTESIAN_POINT ( 'NONE',  ( -35.50000000000000711, -114.9929296450195721, 10.49869535309826674 ) ) ;
#2754 = CARTESIAN_POINT ( 'NONE',  ( -37.34375000000001421, -113.9929510916434339, 14.11852480586265024 ) ) ;
#2755 = DIRECTION ( 'NONE',  ( -1.000000000000000000, 0.000000000000000000, -0.000000000000000000 ) ) ;
#2756 = CARTESIAN_POINT ( 'NONE',  ( -2.000000000000000888, 1.569037991101640822E-15, 7.800000000000023803 ) ) ;
#2757 = CARTESIAN_POINT ( 'NONE',  ( -34.50000000000000000, -113.9929510916430075, 10.50625754673586876 ) ) ;
#2758 = CARTESIAN_POINT ( 'NONE',  ( -39.00000000000000711, -114.9929510916434339, 12.59102132592608925 ) ) ;
#2759 = CARTESIAN_POINT ( 'NONE',  ( -35.50000000000000711, -114.0882517521923489, 9.510534276948430232 ) ) ;
#2760 = AXIS2_PLACEMENT_3D ( 'NONE', #29979, #21488, #19151 ) ;
#2761 = CARTESIAN_POINT ( 'NONE',  ( 7.999999999999992895, 0.000000000000000000, 0.000000000000000000 ) ) ;
#2762 = CYLINDRICAL_SURFACE ( 'NONE', #9475, 4.000000000000000000 ) ;
#2763 = ORIENTED_EDGE ( 'NONE', *, *, #23606, .T. ) ;
#2764 = CARTESIAN_POINT ( 'NONE',  ( 0.000000000000000000, 9.919332006307387317, -5.363026430117004750 ) ) ;
#2765 = DIRECTION ( 'NONE',  ( 0.000000000000000000, -1.000000000000000000, 0.000000000000000000 ) ) ;
#2766 = AXIS2_PLACEMENT_3D ( 'NONE', #23713, #32516, #7330 ) ;
#2767 = VECTOR ( 'NONE', #22739, 1000.000000000000000 ) ;
#2768 = VERTEX_POINT ( 'NONE', #20038 ) ;
#2769 = AXIS2_PLACEMENT_3D ( 'NONE', #15840, #18731, #4557 ) ;
#2770 = CARTESIAN_POINT ( 'NONE',  ( 0.000000000000000000, -2.710505431213761085E-17, 38.00000000000000711 ) ) ;
#2771 = ORIENTED_EDGE ( 'NONE', *, *, #16151, .T. ) ;
#2772 = CARTESIAN_POINT ( 'NONE',  ( -35.50000000000000000, -113.0140978167136581, 0.8752176474015690433 ) ) ;
#2773 = LINE ( 'NONE', #13736, #622 ) ;
#2774 = CARTESIAN_POINT ( 'NONE',  ( -38.02454729103296671, -114.3549511594417396, 5.159774454178449155 ) ) ;
#2775 = AXIS2_PLACEMENT_3D ( 'NONE', #27205, #24322, #16184 ) ;
#2776 = DIRECTION ( 'NONE',  ( -1.000000000000000000, 0.000000000000000000, 0.000000000000000000 ) ) ;
#2777 = EDGE_CURVE ( 'NONE', #34614, #5335, #31042, .T. ) ;
#2778 = ORIENTED_EDGE ( 'NONE', *, *, #4611, .T. ) ;
#2779 = EDGE_CURVE ( 'NONE', #9066, #22316, #7634, .T. ) ;
#2780 =( NAMED_UNIT ( * ) PLANE_ANGLE_UNIT ( ) SI_UNIT ( $, .RADIAN. ) );
#2781 = CARTESIAN_POINT ( 'NONE',  ( -35.50000000000000000, -111.2304026862503719, 1.811733666967775713 ) ) ;
#2782 = ORIENTED_EDGE ( 'NONE', *, *, #11756, .T. ) ;
#2783 = ORIENTED_EDGE ( 'NONE', *, *, #25393, .T. ) ;
#2784 = CARTESIAN_POINT ( 'NONE',  ( -35.00000000000000000, -114.0592624029313242, 4.503524454178448266 ) ) ;
#2785 =( NAMED_UNIT ( * ) SI_UNIT ( $, .STERADIAN. ) SOLID_ANGLE_UNIT ( ) );
#2786 = DIRECTION ( 'NONE',  ( -1.000000000000000000, -1.836970198721029934E-16, -0.000000000000000000 ) ) ;
#2787 = VERTEX_POINT ( 'NONE', #33745 ) ;
#2788 = ORIENTED_EDGE ( 'NONE', *, *, #35495, .T. ) ;
#2789 = CARTESIAN_POINT ( 'NONE',  ( -34.50000000000000000, -113.4307644833805142, -0.6247823525984269599 ) ) ;
#2790 = LINE ( 'NONE', #12548, #11992 ) ;
#2791 = AXIS2_PLACEMENT_3D ( 'NONE', #4865, #10442, #16343 ) ;
#2792 = DIRECTION ( 'NONE',  ( -1.000000000000000000, 0.000000000000000000, 0.000000000000000000 ) ) ;
#2793 = AXIS2_PLACEMENT_3D ( 'NONE', #9523, #6992, #31309 ) ;
#2794 = DIRECTION ( 'NONE',  ( 0.000000000000000000, 0.6427876096865403621, -0.7660444431189772363 ) ) ;
#2795 =( REPRESENTATION_RELATIONSHIP ('NONE','NONE', #26607, #31216 ) REPRESENTATION_RELATIONSHIP_WITH_TRANSFORMATION ( #22561 )SHAPE_REPRESENTATION_RELATIONSHIP( ) );
#2796 = CARTESIAN_POINT ( 'NONE',  ( -35.50000102263781798, -113.9929510916434339, 12.62466071271731494 ) ) ;
#2797 = CYLINDRICAL_SURFACE ( 'NONE', #16693, 7.199999999999994849 ) ;
#2798 = DIRECTION ( 'NONE',  ( -1.783119874454246424E-31, -1.187911941725854497E-31, 1.000000000000000000 ) ) ;
#2799 = COLOUR_RGB ( '', 0.09019608, 0.27058824, 0.51372549) ;
#2800 = CARTESIAN_POINT ( 'NONE',  ( -34.50000000000000000, -111.0140978167138570, -0.4997823525984338988 ) ) ;
#2801 = CARTESIAN_POINT ( 'NONE',  ( -38.95206139890799335, -115.9929510916434481, 13.00730889637963550 ) ) ;
#2802 = UNCERTAINTY_MEASURE_WITH_UNIT (LENGTH_MEASURE( 1.000000000000000082E-05 ), #29781, 'distance_accuracy_value', 'NONE');
#2803 = CARTESIAN_POINT ( 'NONE',  ( 0.000000000000000000, 5.679790370316031733, 7.613867765417614564 ) ) ;
#2804 = DIRECTION ( 'NONE',  ( 0.000000000000000000, -0.8443279255020087470, -0.5358267949790064266 ) ) ;
#2805 = FACE_BOUND ( 'NONE', #34964, .T. ) ;
#2806 = ORIENTED_EDGE ( 'NONE', *, *, #2856, .T. ) ;
#2807 = CARTESIAN_POINT ( 'NONE',  ( -38.00000000000000711, -115.9929510916434481, 12.17846912687782179 ) ) ;
#2808 = LINE ( 'NONE', #27101, #18817 ) ;
#2809 = CARTESIAN_POINT ( 'NONE',  ( 65.00000000000001421, 87.62632027716348659, 34.45236684482946288 ) ) ;
#2810 = CARTESIAN_POINT ( 'NONE',  ( 8.000000000000000000, 3.384281271888069487, -18.48663108841355296 ) ) ;
#2811 = LINE ( 'NONE', #13769, #21103 ) ;
#2812 = VERTEX_POINT ( 'NONE', #12134 ) ;
#2813 = CARTESIAN_POINT ( 'NONE',  ( -34.49999999999998579, -27.48076211353304643, 71.08058909292485339 ) ) ;
#2814 = CARTESIAN_POINT ( 'NONE',  ( 0.000000000000000000, 13.24207120356986422, -14.98824707027428005 ) ) ;
#2815 = DIRECTION ( 'NONE',  ( 0.000000000000000000, -6.866613759074853001E-15, 1.000000000000000000 ) ) ;
#2816 = CARTESIAN_POINT ( 'NONE',  ( 0.000000000000000000, 0.000000000000000000, -34.40000000000000568 ) ) ;
#2817 = AXIS2_PLACEMENT_3D ( 'NONE', #31798, #6779, #34335 ) ;
#2818 = CYLINDRICAL_SURFACE ( 'NONE', #11245, 17.49900000000000233 ) ;
#2819 = CARTESIAN_POINT ( 'NONE',  ( 1.599999999999986766, -5.408326913195883989, 7.044554255117328346E-16 ) ) ;
#2820 = ORIENTED_EDGE ( 'NONE', *, *, #11636, .F. ) ;
#2821 = VECTOR ( 'NONE', #6341, 1000.000000000000000 ) ;
#2822 = EDGE_CURVE ( 'NONE', #11394, #4405, #32374, .T. ) ;
#2823 = FACE_OUTER_BOUND ( 'NONE', #6455, .T. ) ;
#2824 = CYLINDRICAL_SURFACE ( 'NONE', #17671, 20.00000000000000355 ) ;
#2825 = CARTESIAN_POINT ( 'NONE',  ( 7.999999999999992895, 30.93515269692163372, -36.04401931830219752 ) ) ;
#2826 = ORIENTED_EDGE ( 'NONE', *, *, #5262, .T. ) ;
#2827 = CARTESIAN_POINT ( 'NONE',  ( -34.97545270896703329, -114.7691647218148745, 7.090225545821550845 ) ) ;
#2828 = VERTEX_POINT ( 'NONE', #26002 ) ;
#2829 = ORIENTED_EDGE ( 'NONE', *, *, #29760, .T. ) ;
#2830 = ORIENTED_EDGE ( 'NONE', *, *, #33480, .F. ) ;
#2831 = DIRECTION ( 'NONE',  ( 1.000000000000000000, -0.000000000000000000, -0.000000000000000000 ) ) ;
#2832 = ADVANCED_FACE ( 'NONE', ( #14460 ), #6373, .T. ) ;
#2833 = DIRECTION ( 'NONE',  ( -1.000000000000000000, 0.000000000000000000, -0.000000000000000000 ) ) ;
#2834 = ORIENTED_EDGE ( 'NONE', *, *, #18767, .T. ) ;
#2835 = CARTESIAN_POINT ( 'NONE',  ( -35.50000000000000711, -114.1068310684433129, 9.512752019463897923 ) ) ;
#2836 = DIRECTION ( 'NONE',  ( 0.000000000000000000, -1.000000000000000000, 0.000000000000000000 ) ) ;
#2837 = CARTESIAN_POINT ( 'NONE',  ( 7.999999999999992895, 0.000000000000000000, 0.000000000000000000 ) ) ;
#2838 = CARTESIAN_POINT ( 'NONE',  ( 0.000000000000000000, 0.000000000000000000, 0.000000000000000000 ) ) ;
#2839 = CARTESIAN_POINT ( 'NONE',  ( 1.520000000000018447, -3.699466227802803499E-16, -5.016000000000010672 ) ) ;
#2840 = VECTOR ( 'NONE', #7984, 1000.000000000000000 ) ;
#2841 = CARTESIAN_POINT ( 'NONE',  ( 4.000000000000000000, -0.5097555531871980072, -19.99350267651955804 ) ) ;
#2842 = CARTESIAN_POINT ( 'NONE',  ( -38.99984940073100148, -115.9929510916434481, 12.64306614848957544 ) ) ;
#2843 = DIRECTION ( 'NONE',  ( 1.000000000000000000, 0.000000000000000000, 0.000000000000000000 ) ) ;
#2844 = CARTESIAN_POINT ( 'NONE',  ( 0.000000000000000000, 9.604183132802424083, -5.908880290975567995 ) ) ;
#2845 = CARTESIAN_POINT ( 'NONE',  ( 4.000000000000003553, -9.508666619816789733, 19.83898331853681896 ) ) ;
#2846 = CARTESIAN_POINT ( 'NONE',  ( -37.49999999999999289, -4.676198662292047281, 104.0227405789415798 ) ) ;
#2847 = DIRECTION ( 'NONE',  ( -1.000000000000000000, 0.000000000000000000, 0.000000000000000000 ) ) ;
#2848 = FACE_OUTER_BOUND ( 'NONE', #11113, .T. ) ;
#2849 = ORIENTED_EDGE ( 'NONE', *, *, #24871, .F. ) ;
#2850 = CARTESIAN_POINT ( 'NONE',  ( -36.25098837183130485, -114.6652019342044184, 4.183975545821551734 ) ) ;
#2851 = CARTESIAN_POINT ( 'NONE',  ( -42.49999999999999289, -10.50833024919764469, 77.79903810567677169 ) ) ;
#2852 = DIRECTION ( 'NONE',  ( 1.174092375852890260E-15, -4.222049128630259891E-16, -1.000000000000000000 ) ) ;
#2853 = DIRECTION ( 'NONE',  ( 0.000000000000000000, 0.000000000000000000, -1.000000000000000000 ) ) ;
#2854 = VERTEX_POINT ( 'NONE', #6203 ) ;
#2855 = ORIENTED_EDGE ( 'NONE', *, *, #6898, .T. ) ;
#2856 = EDGE_CURVE ( 'NONE', #1839, #25395, #10526, .T. ) ;
#2857 = LINE ( 'NONE', #16320, #15912 ) ;
#2858 = DIRECTION ( 'NONE',  ( -0.000000000000000000, -0.2538061376417690140, -0.9672551082808337197 ) ) ;
#2859 = ORIENTED_EDGE ( 'NONE', *, *, #16384, .F. ) ;
#2860 = EDGE_CURVE ( 'NONE', #5109, #16923, #19694, .T. ) ;
#2861 = AXIS2_PLACEMENT_3D ( 'NONE', #7141, #18116, #29121 ) ;
#2862 = ORIENTED_EDGE ( 'NONE', *, *, #6391, .F. ) ;
#2863 = VECTOR ( 'NONE', #27050, 1000.000000000000000 ) ;
#2864 = CARTESIAN_POINT ( 'NONE',  ( 7.999999999999992895, -42.03146605346803000, 22.12489237027305577 ) ) ;
#2865 = CARTESIAN_POINT ( 'NONE',  ( 0.000000000000000000, 0.000000000000000000, 0.000000000000000000 ) ) ;
#2866 = ADVANCED_FACE ( 'NONE', ( #9255 ), #14998, .F. ) ;
#2867 = AXIS2_PLACEMENT_3D ( 'NONE', #22513, #14409, #16756 ) ;
#2868 = DIRECTION ( 'NONE',  ( -1.110223024625156540E-16, 0.2829836251474256992, -0.9591247405308765961 ) ) ;
#2869 = DIRECTION ( 'NONE',  ( -1.000000000000000000, 0.000000000000000000, 0.000000000000000000 ) ) ;
#2870 = VERTEX_POINT ( 'NONE', #12310 ) ;
#2871 = ORIENTED_EDGE ( 'NONE', *, *, #30764, .F. ) ;
#2872 = DIRECTION ( 'NONE',  ( 0.000000000000000000, 0.000000000000000000, -1.000000000000000000 ) ) ;
#2873 = CARTESIAN_POINT ( 'NONE',  ( -1.000000000000014655, -4.808326913196006913, -0.7999999999999951594 ) ) ;
#2874 = VERTEX_POINT ( 'NONE', #14639 ) ;
#2875 = CARTESIAN_POINT ( 'NONE',  ( 8.000000000000007105, 9.637487275701129619, 10.15474465512053470 ) ) ;
#2876 = CARTESIAN_POINT ( 'NONE',  ( -34.50000000000000000, -112.1403507321855528, -1.128496220798856253 ) ) ;
#2877 = CARTESIAN_POINT ( 'NONE',  ( -37.18750000000006395, -114.9929510916434339, 14.11852480586264846 ) ) ;
#2878 = CARTESIAN_POINT ( 'NONE',  ( -35.50000000000000000, -113.9186338266397058, 10.49738657667399266 ) ) ;
#2879 = LINE ( 'NONE', #153, #33543 ) ;
#2880 = CARTESIAN_POINT ( 'NONE',  ( -36.00976557831293690, -114.9929510916434339, 14.11852773550420359 ) ) ;
#2881 = DIRECTION ( 'NONE',  ( -1.000000000000000000, 0.000000000000000000, 0.000000000000000000 ) ) ;
#2882 = ADVANCED_FACE ( 'NONE', ( #34281 ), #28876, .F. ) ;
#2883 = CARTESIAN_POINT ( 'NONE',  ( -9.999999999999994671, 0.000000000000000000, 0.000000000000000000 ) ) ;
#2884 = CARTESIAN_POINT ( 'NONE',  ( 0.000000000000000000, -2.710505431213761085E-17, -45.10000000000000142 ) ) ;
#2885 = FACE_BOUND ( 'NONE', #33804, .T. ) ;
#2886 = DIRECTION ( 'NONE',  ( 0.000000000000000000, 0.000000000000000000, -1.000000000000000000 ) ) ;
#2887 = EDGE_LOOP ( 'NONE', ( #26162, #35518, #4200, #22277 ) ) ;
#2888 = DIRECTION ( 'NONE',  ( 0.000000000000000000, 0.000000000000000000, 1.000000000000000000 ) ) ;
#2889 = ORIENTED_EDGE ( 'NONE', *, *, #10154, .F. ) ;
#2890 = AXIS2_PLACEMENT_3D ( 'NONE', #21151, #32145, #26941 ) ;
#2891 = CIRCLE ( 'NONE', #14930, 7.199999999999991296 ) ;
#2892 = CARTESIAN_POINT ( 'NONE',  ( -39.07941549657748936, -111.8367748094582055, 6.941024454178450043 ) ) ;
#2893 = AXIS2_PLACEMENT_3D ( 'NONE', #19566, #5902, #6080 ) ;
#2894 = DIRECTION ( 'NONE',  ( 0.000000000000000000, -0.8660254037844327124, -0.5000000000000101030 ) ) ;
#2895 = ORIENTED_EDGE ( 'NONE', *, *, #33936, .T. ) ;
#2896 = VERTEX_POINT ( 'NONE', #9612 ) ;
#2897 = EDGE_CURVE ( 'NONE', #25998, #4505, #24923, .T. ) ;
#2898 = DIRECTION ( 'NONE',  ( 0.000000000000000000, 0.000000000000000000, 1.000000000000000000 ) ) ;
#2899 = CARTESIAN_POINT ( 'NONE',  ( 0.000000000000000000, 0.000000000000000000, -40.89999999999999858 ) ) ;
#2900 = ADVANCED_FACE ( 'NONE', ( #31578 ), #17880, .F. ) ;
#2901 = EDGE_CURVE ( 'NONE', #13424, #2693, #1511, .T. ) ;
#2902 = EDGE_LOOP ( 'NONE', ( #9794, #22603, #23283, #8221 ) ) ;
#2903 = CARTESIAN_POINT ( 'NONE',  ( -35.81662171581204746, -117.0245472910329738, 7.784774454178449155 ) ) ;
#2904 = DIRECTION ( 'NONE',  ( 0.000000000000000000, 0.000000000000000000, 1.000000000000000000 ) ) ;
#2905 = DIRECTION ( 'NONE',  ( -1.000000000000000000, 0.000000000000000000, 0.000000000000000000 ) ) ;
#2906 = EDGE_LOOP ( 'NONE', ( #24197, #13132, #7241, #3218 ) ) ;
#2907 = EDGE_LOOP ( 'NONE', ( #5346, #10050 ) ) ;
#2908 = LINE ( 'NONE', #11351, #30907 ) ;
#2909 = EDGE_CURVE ( 'NONE', #14462, #19761, #12277, .T. ) ;
#2910 = EDGE_CURVE ( 'NONE', #7078, #26596, #21460, .T. ) ;
#2911 = FACE_BOUND ( 'NONE', #26913, .T. ) ;
#2912 = ORIENTED_EDGE ( 'NONE', *, *, #11957, .F. ) ;
#2913 = ORIENTED_EDGE ( 'NONE', *, *, #26815, .F. ) ;
#2914 = CIRCLE ( 'NONE', #9205, 13.99999999999999645 ) ;
#2915 = CARTESIAN_POINT ( 'NONE',  ( -34.50000000000000000, -115.1449503510569059, -2.621568770093253953 ) ) ;
#2916 = DIRECTION ( 'NONE',  ( -1.000000000000000000, 0.000000000000000000, 0.000000000000000000 ) ) ;
#2917 = AXIS2_PLACEMENT_3D ( 'NONE', #2816, #87, #29987 ) ;
#2918 = CIRCLE ( 'NONE', #599, 19.99999999999998579 ) ;
#2919 = ORIENTED_EDGE ( 'NONE', *, *, #24743, .T. ) ;
#2920 = CARTESIAN_POINT ( 'NONE',  ( -37.50613590685470911, -114.9929510916434339, 13.11852378322482515 ) ) ;
#2921 = CARTESIAN_POINT ( 'NONE',  ( -34.49999793727135966, -113.9929510916434339, 12.61164896875036767 ) ) ;
#2922 = DIRECTION ( 'NONE',  ( 0.000000000000000000, 0.000000000000000000, -1.000000000000000000 ) ) ;
#2923 = LINE ( 'NONE', #16913, #6457 ) ;
#2924 = CARTESIAN_POINT ( 'NONE',  ( -34.50000000000000000, -113.9929510916434339, 10.50625754673577994 ) ) ;
#2925 = CARTESIAN_POINT ( 'NONE',  ( -38.99924736195578134, -114.9929510916434339, 12.66759465831984777 ) ) ;
#2926 = EDGE_CURVE ( 'NONE', #26998, #31709, #11771, .T. ) ;
#2927 = CARTESIAN_POINT ( 'NONE',  ( -35.50000000000000711, -114.1712995509219724, 9.522174004479579068 ) ) ;
#2928 = CARTESIAN_POINT ( 'NONE',  ( 8.000000000000007105, 0.000000000000000000, 0.000000000000000000 ) ) ;
#2929 = ORIENTED_EDGE ( 'NONE', *, *, #9500, .T. ) ;
#2930 = ADVANCED_FACE ( 'NONE', ( #10143 ), #18419, .T. ) ;
#2931 = ORIENTED_EDGE ( 'NONE', *, *, #35217, .F. ) ;
#2932 = AXIS2_PLACEMENT_3D ( 'NONE', #34706, #15585, #20808 ) ;
#2933 = ADVANCED_FACE ( 'NONE', ( #32112 ), #31924, .T. ) ;
#2934 = DIRECTION ( 'NONE',  ( -1.000000000000000000, 0.000000000000000000, 0.000000000000000000 ) ) ;
#2935 = DIRECTION ( 'NONE',  ( -1.000000000000000000, 0.000000000000000000, 0.000000000000000000 ) ) ;
#2936 = ORIENTED_EDGE ( 'NONE', *, *, #24914, .F. ) ;
#2937 = AXIS2_PLACEMENT_3D ( 'NONE', #2844, #32715, #21899 ) ;
#2938 = LINE ( 'NONE', #8303, #31408 ) ;
#2939 = VERTEX_POINT ( 'NONE', #29418 ) ;
#2940 = CARTESIAN_POINT ( 'NONE',  ( -35.50000000000000711, -116.0140978167138712, -0.5622823525984409487 ) ) ;
#2941 = CARTESIAN_POINT ( 'NONE',  ( -55.00000000000000000, 19.99999999999998934, 120.0000000000000000 ) ) ;
#2942 = CARTESIAN_POINT ( 'NONE',  ( -36.02454729103298092, -114.4734759653044307, 6.097274454178449155 ) ) ;
#2943 = ADVANCED_FACE ( 'NONE', ( #26546 ), #12681, .T. ) ;
#2944 = EDGE_CURVE ( 'NONE', #6784, #32680, #30679, .T. ) ;
#2945 = AXIS2_PLACEMENT_3D ( 'NONE', #1471, #25798, #28671 ) ;
#2946 = DIRECTION ( 'NONE',  ( -1.000000000000000000, 0.000000000000000000, 0.000000000000000000 ) ) ;
#2947 = AXIS2_PLACEMENT_3D ( 'NONE', #15443, #21386, #13138 ) ;
#2948 = EDGE_LOOP ( 'NONE', ( #12283, #16111, #1287, #33253 ) ) ;
#2949 = CARTESIAN_POINT ( 'NONE',  ( 0.000000000000000000, 5.908880290975540461, 9.604183132802438294 ) ) ;
#2950 = CARTESIAN_POINT ( 'NONE',  ( -35.50000000000000000, -115.5324766040685631, -2.560864217809699195 ) ) ;
#2951 = VERTEX_POINT ( 'NONE', #4590 ) ;
#2952 = EDGE_LOOP ( 'NONE', ( #28785, #26177, #20547, #21737 ) ) ;
#2953 = CARTESIAN_POINT ( 'NONE',  ( -37.88768952767750164, -115.9754527089670262, 6.472274454178450043 ) ) ;
#2954 = EDGE_CURVE ( 'NONE', #9823, #7205, #23657, .T. ) ;
#2955 = DIRECTION ( 'NONE',  ( 0.000000000000000000, 0.000000000000000000, 1.000000000000000000 ) ) ;
#2956 = ORIENTED_EDGE ( 'NONE', *, *, #21274, .F. ) ;
#2957 = ORIENTED_EDGE ( 'NONE', *, *, #8447, .F. ) ;
#2958 = CARTESIAN_POINT ( 'NONE',  ( -34.50000000000000000, -115.0140978167140986, -0.6247823525984417259 ) ) ;
#2959 = CARTESIAN_POINT ( 'NONE',  ( 3.799999999999999822, 4.382607293638566128E-16, 45.89999999999999858 ) ) ;
#2960 =( BOUNDED_SURFACE ( )  B_SPLINE_SURFACE ( 3, 3, ( 
 ( #31743, #31917, #12675, #4396, #15162, #31572, #17700, #14993, #34273, #26718, #12851, #1324, #15344, #26356, #23652, #18414, #9960, #12304, #15521, #26539, #23828, #21106, #2054, #32107, #7436, #4757, #23275, #13028, #24018, #35004, #32284, #16050, #2588, #32455, #7782, #7965, #29772, #5285, #5113, #18768, #16225, #27069, #2412, #13380, #13552, #15876, #10676, #18593, #8138, #24362, #24187, #35180, #35350, #21636, #26901, #10496, #27247, #32642, #18945, #29945, #2243, #24540, #19118, #21461, #35535, #10862, #21821, #5456, #32819, #7603, #30119, #16407, #27426, #29593, #4932, #13209, #34751, #18354, #10072, #12783, #21038, #32399, #20855, #4701, #35119, #23763, #7718, #26110, #7189, #32046, #29179, #31856, #24128, #7381, #15633, #34574, #29354, #4333, #4528, #18701, #1628, #28985, #7011, #26655, #15459, #4158, #15100, #1440, #32223, #9720, #12420, #7550, #23405, #21228, #18168, #34402, #18529, #26474, #9889, #20679, #1809, #31677, #34944, #12607, #1985, #17986, #12962, #23947, #26293, #10266, #15278, #29533, #2183, #23581, #4866, #15809, #26829, #13153, #10443, #21402, #16344, #11144, #11319, #7901, #3049, #16082, #2529, #19226, #5741, #30057, #27008, #19058, #10969, #21570, #22111, #24652, #33107, #35295 ),
 ( #10795, #35464, #2878, #5397, #24476, #13494, #8431, #24304, #21934, #5049, #14008, #21754, #18886, #29881, #27357, #32749, #10613, #5227, #16532, #32929, #30232, #8251, #32567, #2705, #25001, #8075, #13840, #13672, #5570, #326, #24828, #29700, #27186, #16167, #27542, #152, #19415, #27711, #30413, #16699, #22289, #33284, #8600, #15993, #2353, #13323, #9404, #25813, #23083, #26340, #6523, #3846, #29031, #18034, #12289, #31559, #1139, #14975, #31193, #6704, #1675, #17858, #7058, #25982, #31018, #12469, #4380, #31374, #15325, #26152, #20361, #9940, #28498, #20188, #33901, #6884, #17685, #34620, #6350, #23634, #23455, #953, #17316, #34450, #14617, #9767, #28684, #28321, #20728, #12112, #34079, #3667, #4031, #11937, #1486, #14806, #1305, #9230, #23260, #34257, #17498, #9590, #25628, #28855, #12657, #22908, #20558, #4207, #31727, #15147, #13538, #35162, #7590, #2396, #2571, #34797, #29928, #26881, #29400, #10483, #32618, #21270, #18217, #10309, #2227, #12830, #13364, #15858, #24346, #26525, #13195, #20903, #24168, #24524, #21444, #16208, #4745, #18929, #32441, #7765, #7948, #32269, #18577, #18398, #18747, #5269, #27229, #15682, #35513, #29578, #31901, #1859, #21086, #7236, #29223, #10660, #4571, #23813 ),
 ( #15505, #35336, #10119, #32091, #7421, #26700, #2036, #13012, #23997, #34988, #4913, #21617, #29751, #5095, #16036, #27054, #30279, #198, #24873, #5619, #2924, #6135, #21980, #32976, #27755, #13883, #2757, #16389, #5956, #19271, #16580, #24698, #30460, #11182, #8291, #22154, #25408, #8650, #8819, #19102, #33152, #3448, #14228, #3095, #14400, #25045, #8481, #27921, #28105, #25, #19781, #16745, #27588, #368, #22504, #19461, #8120, #5788, #14048, #13719, #3270, #11365, #25228, #27408, #22331, #10842, #33327, #21801, #19617, #17097, #30622, #30794, #16915, #551, #33494, #11538, #32799, #30099, #5437, #11014, #34404, #20145, #15280, #25764, #11703, #6307, #901, #31679, #22672, #26112, #28987, #17274, #1442, #12064, #28638, #33664, #4335, #9722, #4161, #722, #3624, #9001, #7013, #14569, #19966, #12422, #30973, #28279, #17810, #23038, #31151, #15103, #23408, #6482, #1093, #14755, #17455, #28453, #17989, #11883, #22860, #17635, #3798, #25583, #20682, #20322, #33856, #28811, #9183, #34036, #9363, #31516, #31330, #6656, #3984, #14929, #25940, #12248, #1262, #23221, #34214, #9544, #20510, #6838, #5229, #18703, #9891, #7720, #4703, #29884, #29702, #7383, #21040, #26295, #18356, #21230, #4868, #32227 ),
 ( #34576, #10268, #18888, #12609, #29359, #20857, #34753, #24306, #13325, #7553, #26831, #32048, #18531, #26478, #1987, #21572, #13155, #12964, #29181, #29536, #1631, #15811, #1811, #15462, #15635, #26657, #23585, #5051, #2186, #23950, #32569, #34946, #31859, #10445, #4530, #35298, #12785, #10075, #7191, #24130, #35122, #21405, #23765, #2356, #32402, #15996, #27010, #10615, #7903, #18170, #16169, #2531, #32751, #14189, #11321, #27188, #10972, #24830, #8079, #16877, #5399, #13497, #19060, #27360, #16346, #16702, #514, #13844, #5912, #11146, #10797, #13674, #32931, #19418, #328, #5573, #22291, #24654, #14369, #30416, #8253, #3051, #19228, #21937, #25003, #16535, #30234, #27544, #8603, #21756, #22113, #24478, #25191, #2880, #2707, #155, #33109, #8433, #30059, #5743, #14011, #27713, #33287, #19575, #30579, #27881, #11493, #3226, #22463, #33453, #8776, #19743, #30755, #35466, #3579, #30935, #9324, #8956, #12207, #4123, #34356, #20281, #28413, #23181, #23358, #19921, #15063, #12026, #14526, #31291, #17768, #6440, #3410, #31113, #22997, #33623, #34177, #1055, #9501, #11661, #34000, #6090, #6615, #9682, #17586, #1403, #25543, #26073, #28594, #3945, #28770, #17410, #3754, #855, #14890, #12380, #20637, #11837 ),
 ( #25902, #1230, #20459, #31471, #6267, #14709, #17056, #22818, #6797, #9143, #28069, #14358, #25368, #679, #33818, #17232, #22631, #28239, #20105, #25723, #26611, #10222, #1946, #4660, #12921, #2137, #23719, #13284, #4296, #15590, #24263, #17946, #34711, #26247, #4482, #29658, #18661, #23906, #32181, #26432, #34899, #31816, #7337, #26974, #18489, #18313, #34533, #21188, #35249, #7508, #7152, #20813, #20998, #32001, #31636, #35079, #29488, #1762, #2315, #29312, #1587, #15768, #9849, #5000, #18126, #15421, #6973, #10035, #4827, #26787, #29130, #7677, #12744, #13114, #24095, #10403, #21361, #23538, #28947, #15236, #12566, #15956, #32354, #10571, #16301, #30190, #3184, #115, #16837, #30020, #19534, #24791, #33067, #33244, #21897, #32891, #19022, #19367, #8564, #30540, #5356, #468, #10931, #32523, #27143, #21716, #27842, #7855, #11273, #14141, #2483, #22246, #8213, #13803, #18846, #25141, #5870, #24964, #21524, #24433, #29846, #5187, #35420, #16126, #13453, #10750, #32713, #3013, #19191, #27316, #287, #8040, #2661, #5527, #35602, #13624, #24615, #16485, #27503, #2842, #11106, #22074, #8384, #30372, #5701, #16661, #13973, #27672, #11793, #9450, #6565, #811, #26027, #8913, #638, #14313, #22953, #22772 ),
 ( #11451, #3895, #30715, #28547, #25494, #15023, #14851, #28195, #6225, #22417, #3536, #17009, #17541, #19877, #17187, #25319, #31068, #33773, #33579, #9102, #33409, #9278, #20409, #19699, #20062, #4081, #25860, #3709, #8731, #25675, #6396, #1186, #28730, #11615, #31421, #17364, #30890, #1009, #23130, #28366, #6047, #14662, #11985, #3366, #12158, #33951, #34127, #28019, #20233, #22588, #31245, #6751, #17727, #14484, #28901, #1356, #23309, #17905, #35036, #32134, #12332, #31772, #9989, #4251, #2087, #26197, #34309, #15188, #12518, #1535, #1904, #21316, #34668, #26746, #31951, #31597, #34490, #18078, #4614, #21140, #26382, #7464, #9809, #20772, #15548, #29079, #23858, #4428, #7105, #10172, #1716, #15371, #12700, #29441, #6932, #7287, #9638, #10356, #23676, #23495, #20950, #18261, #29266, #26566, #12879, #34847, #18444, #4786, #15729, #13066, #24051, #32310, #7635, #18622, #29620, #4958, #15914, #20599, #26931, #24392, #16083, #30148, #29804, #33027, #24924, #21856, #5485, #32850, #35566, #8169, #8340, #18980, #9010, #35207, #10891, #19974, #13241, #29978, #21487, #35378, #247, #13935, #19150, #27461, #21674, #16440, #27100, #2617, #22201, #13766, #13581, #5143, #2807, #30982, #24751, #2439, #13410, #16256 ),
 ( #6314, #19321, #10527, #30334, #5316, #2273, #5666, #7997, #32676, #24216, #27275, #32479, #22034, #10704, #24575, #77, #16625, #7812, #18804, #27638, #11064, #2976, #11232, #33675, #20691, #34044, #12073, #17283, #9371, #22869, #12433, #25775, #23046, #31160, #1270, #6667, #3808, #31340, #31867, #15111, #15291, #25592, #3996, #9902, #31689, #9553, #20865, #31524, #14938, #34413, #34585, #6489, #26303, #23230, #1102, #6848, #28995, #17644, #14580, #28648, #34223, #9192, #9730, #12256, #7021, #33866, #20520, #28287, #17820, #3631, #28819, #12618, #20330, #1639, #4169, #26120, #4345, #25947, #1453, #14766, #23416, #23593, #913, #17997, #11893, #20153, #17464, #28462, #7393, #2538, #29191, #32580, #35476, #23775, #7914, #18541, #35132, #4538, #10807, #16177, #10624, #21766, #10085, #15470, #13505, #21051, #7198, #18896, #18179, #12795, #24313, #29544, #26666, #21581, #29893, #1998, #32234, #21241, #12973, #34955, #24487, #18365, #29367, #24138, #10276, #34761, #5237, #26842, #26488, #35306, #27199, #7560, #1819, #2364, #4877, #32056, #4712, #15644, #23960, #18713, #15821, #2195, #13163, #10453, #21414, #32410, #7729, #29715, #5059, #16004, #27019, #13335, #30425, #22472, #27723, #27369, #30242, #13854 ) ),
 .UNSPECIFIED., .T., .F., .F. ) 
 B_SPLINE_SURFACE_WITH_KNOTS ( ( 4, 3, 4 ),
 ( 4, 2, 2, 2, 2, 2, 2, 2, 2, 2, 2, 2, 2, 2, 2, 2, 2, 2, 2, 2, 2, 2, 2, 2, 2, 2, 2, 2, 2, 2, 2, 2, 2, 2, 2, 2, 2, 2, 2, 2, 2, 2, 2, 2, 2, 2, 2, 2, 2, 2, 2, 2, 2, 2, 2, 2, 2, 2, 2, 2, 2, 2, 2, 2, 2, 2, 2, 2, 2, 2, 2, 2, 2, 2, 2, 2, 2, 2, 4 ),
 ( 0.000000000000000000, 0.5000000000000000000, 1.000000000000000000 ),
 ( 0.000000000000000000, 0.005381740036788157898, 0.008072610055182236413, 0.009418045064379276105, 0.01009076256897779508, 0.01076348007357631580, 0.01185104180586291078, 0.01293860353814950404, 0.01511372700272269054, 0.01946397393186906355, 0.02816446779016181304, 0.04556545550674730855, 0.08036743093991829956, 0.1151694063730892975, 0.1325703940896748034, 0.1412708879479675494, 0.1456211348771139225, 0.1477962583416871090, 0.1488838200739737161, 0.1499713818062602955, 0.1507624401091536004, 0.1515534984120469053, 0.1531356150178334874, 0.1562998482294066793, 0.1626283146525530909, 0.1752852474988458864, 0.2005991131914315051, 0.2512268445766027147, 0.3018545759617738966, 0.3271684416543594875, 0.3398253745006523108, 0.3461538409237986946, 0.3493180741353718588, 0.3509001907411584686, 0.3524823073469450785, 0.3548354025267266287, 0.3571884977065081790, 0.3618946880660712795, 0.3713070687851974805, 0.3901318302234498825, 0.4277813530999547420, 0.4654308759764596015, 0.4842556374147120035, 0.4936680181338382045, 0.4983742084934013050, 0.5007273036731828553, 0.5030803988529644055, 0.5053274392295320494, 0.5075744796060996933, 0.5120685603592350921, 0.5210567218655057786, 0.5390330448780472627, 0.5749856909031301200, 0.6109383369282129772, 0.6289146599407544613, 0.6379028214470251479, 0.6423969022001605467, 0.6446439425767281906, 0.6468909829532958344, 0.6492440781330773847, 0.6515971733128589349, 0.6563033636724220354, 0.6657157443915482364, 0.6845405058298006384, 0.7221900287063054424, 0.7598395515828102464, 0.7786643130210626484, 0.7880766937401888494, 0.7927828840997519499, 0.7951359792795336112, 0.7974890744593151615, 0.7990711910651018268, 0.8006533076708883812, 0.8038175408824614898, 0.8101460073056079292, 0.8228029401519008079, 0.8481168058444863433, 0.8987445372296576362, 1.000000000000000000 ),
 .UNSPECIFIED. ) 
 GEOMETRIC_REPRESENTATION_ITEM ( )  RATIONAL_B_SPLINE_SURFACE ( (
 ( 1.000000000000000000, 1.000000000000000000, 1.000000000000000000, 1.000000000000000000, 1.000000000000000000, 1.000000000000000000, 1.000000000000000000, 1.000000000000000000, 1.000000000000000000, 1.000000000000000000, 1.000000000000000000, 1.000000000000000000, 1.000000000000000000, 1.000000000000000000, 1.000000000000000000, 1.000000000000000000, 1.000000000000000000, 1.000000000000000000, 1.000000000000000000, 1.000000000000000000, 1.000000000000000000, 1.000000000000000000, 1.000000000000000000, 1.000000000000000000, 1.000000000000000000, 1.000000000000000000, 1.000000000000000000, 1.000000000000000000, 1.000000000000000000, 1.000000000000000000, 1.000000000000000000, 1.000000000000000000, 1.000000000000000000, 1.000000000000000000, 1.000000000000000000, 1.000000000000000000, 1.000000000000000000, 1.000000000000000000, 1.000000000000000000, 1.000000000000000000, 1.000000000000000000, 1.000000000000000000, 1.000000000000000000, 1.000000000000000000, 1.000000000000000000, 1.000000000000000000, 1.000000000000000000, 1.000000000000000000, 1.000000000000000000, 1.000000000000000000, 1.000000000000000000, 1.000000000000000000, 1.000000000000000000, 1.000000000000000000, 1.000000000000000000, 1.000000000000000000, 1.000000000000000000, 1.000000000000000000, 1.000000000000000000, 1.000000000000000000, 1.000000000000000000, 1.000000000000000000, 1.000000000000000000, 1.000000000000000000, 1.000000000000000000, 1.000000000000000000, 1.000000000000000000, 1.000000000000000000, 1.000000000000000000, 1.000000000000000000, 1.000000000000000000, 1.000000000000000000, 1.000000000000000000, 1.000000000000000000, 1.000000000000000000, 1.000000000000000000, 1.000000000000000000, 1.000000000000000000, 1.000000000000000000, 1.000000000000000000, 1.000000000000000000, 1.000000000000000000, 1.000000000000000000, 1.000000000000000000, 1.000000000000000000, 1.000000000000000000, 1.000000000000000000, 1.000000000000000000, 1.000000000000000000, 1.000000000000000000, 1.000000000000000000, 1.000000000000000000, 1.000000000000000000, 1.000000000000000000, 1.000000000000000000, 1.000000000000000000, 1.000000000000000000, 1.000000000000000000, 1.000000000000000000, 1.000000000000000000, 1.000000000000000000, 1.000000000000000000, 1.000000000000000000, 1.000000000000000000, 1.000000000000000000, 1.000000000000000000, 1.000000000000000000, 1.000000000000000000, 1.000000000000000000, 1.000000000000000000, 1.000000000000000000, 1.000000000000000000, 1.000000000000000000, 1.000000000000000000, 1.000000000000000000, 1.000000000000000000, 1.000000000000000000, 1.000000000000000000, 1.000000000000000000, 1.000000000000000000, 1.000000000000000000, 1.000000000000000000, 1.000000000000000000, 1.000000000000000000, 1.000000000000000000, 1.000000000000000000, 1.000000000000000000, 1.000000000000000000, 1.000000000000000000, 1.000000000000000000, 1.000000000000000000, 1.000000000000000000, 1.000000000000000000, 1.000000000000000000, 1.000000000000000000, 1.000000000000000000, 1.000000000000000000, 1.000000000000000000, 1.000000000000000000, 1.000000000000000000, 1.000000000000000000, 1.000000000000000000, 1.000000000000000000, 1.000000000000000000, 1.000000000000000000, 1.000000000000000000, 1.000000000000000000, 1.000000000000000000, 1.000000000000000000, 1.000000000000000000, 1.000000000000000000, 1.000000000000000000, 1.000000000000000000, 1.000000000000000000, 1.000000000000000000, 1.000000000000000000, 1.000000000000000000, 1.000000000000000000),
 ( 0.3333333333333333703, 0.3333333333333333703, 0.3333333333333333703, 0.3333333333333333703, 0.3333333333333333703, 0.3333333333333333703, 0.3333333333333333703, 0.3333333333333333703, 0.3333333333333333703, 0.3333333333333333703, 0.3333333333333333703, 0.3333333333333333703, 0.3333333333333333703, 0.3333333333333333703, 0.3333333333333333703, 0.3333333333333333703, 0.3333333333333333703, 0.3333333333333333703, 0.3333333333333333703, 0.3333333333333333703, 0.3333333333333333703, 0.3333333333333333703, 0.3333333333333333703, 0.3333333333333333703, 0.3333333333333333703, 0.3333333333333333703, 0.3333333333333333703, 0.3333333333333333703, 0.3333333333333333703, 0.3333333333333333703, 0.3333333333333333703, 0.3333333333333333703, 0.3333333333333333703, 0.3333333333333333703, 0.3333333333333333703, 0.3333333333333333703, 0.3333333333333333703, 0.3333333333333333703, 0.3333333333333333703, 0.3333333333333333703, 0.3333333333333333703, 0.3333333333333333703, 0.3333333333333333703, 0.3333333333333333703, 0.3333333333333333703, 0.3333333333333333703, 0.3333333333333333703, 0.3333333333333333703, 0.3333333333333333703, 0.3333333333333333703, 0.3333333333333333703, 0.3333333333333333703, 0.3333333333333333703, 0.3333333333333333703, 0.3333333333333333703, 0.3333333333333333703, 0.3333333333333333703, 0.3333333333333333703, 0.3333333333333333703, 0.3333333333333333703, 0.3333333333333333703, 0.3333333333333333703, 0.3333333333333333703, 0.3333333333333333703, 0.3333333333333333703, 0.3333333333333333703, 0.3333333333333333703, 0.3333333333333333703, 0.3333333333333333703, 0.3333333333333333703, 0.3333333333333333703, 0.3333333333333333703, 0.3333333333333333703, 0.3333333333333333703, 0.3333333333333333703, 0.3333333333333333703, 0.3333333333333333703, 0.3333333333333333703, 0.3333333333333333703, 0.3333333333333333703, 0.3333333333333333703, 0.3333333333333333703, 0.3333333333333333703, 0.3333333333333333703, 0.3333333333333333703, 0.3333333333333333703, 0.3333333333333333703, 0.3333333333333333703, 0.3333333333333333703, 0.3333333333333333703, 0.3333333333333333703, 0.3333333333333333703, 0.3333333333333333703, 0.3333333333333333703, 0.3333333333333333703, 0.3333333333333333703, 0.3333333333333333703, 0.3333333333333333703, 0.3333333333333333703, 0.3333333333333333703, 0.3333333333333333703, 0.3333333333333333703, 0.3333333333333333703, 0.3333333333333333703, 0.3333333333333333703, 0.3333333333333333703, 0.3333333333333333703, 0.3333333333333333703, 0.3333333333333333703, 0.3333333333333333703, 0.3333333333333333703, 0.3333333333333333703, 0.3333333333333333703, 0.3333333333333333703, 0.3333333333333333703, 0.3333333333333333703, 0.3333333333333333703, 0.3333333333333333703, 0.3333333333333333703, 0.3333333333333333703, 0.3333333333333333703, 0.3333333333333333703, 0.3333333333333333703, 0.3333333333333333703, 0.3333333333333333703, 0.3333333333333333703, 0.3333333333333333703, 0.3333333333333333703, 0.3333333333333333703, 0.3333333333333333703, 0.3333333333333333703, 0.3333333333333333703, 0.3333333333333333703, 0.3333333333333333703, 0.3333333333333333703, 0.3333333333333333703, 0.3333333333333333703, 0.3333333333333333703, 0.3333333333333333703, 0.3333333333333333703, 0.3333333333333333703, 0.3333333333333333703, 0.3333333333333333703, 0.3333333333333333703, 0.3333333333333333703, 0.3333333333333333703, 0.3333333333333333703, 0.3333333333333333703, 0.3333333333333333703, 0.3333333333333333703, 0.3333333333333333703, 0.3333333333333333703, 0.3333333333333333703, 0.3333333333333333703, 0.3333333333333333703, 0.3333333333333333703, 0.3333333333333333703, 0.3333333333333333703),
 ( 0.3333333333333333703, 0.3333333333333333703, 0.3333333333333333703, 0.3333333333333333703, 0.3333333333333333703, 0.3333333333333333703, 0.3333333333333333703, 0.3333333333333333703, 0.3333333333333333703, 0.3333333333333333703, 0.3333333333333333703, 0.3333333333333333703, 0.3333333333333333703, 0.3333333333333333703, 0.3333333333333333703, 0.3333333333333333703, 0.3333333333333333703, 0.3333333333333333703, 0.3333333333333333703, 0.3333333333333333703, 0.3333333333333333703, 0.3333333333333333703, 0.3333333333333333703, 0.3333333333333333703, 0.3333333333333333703, 0.3333333333333333703, 0.3333333333333333703, 0.3333333333333333703, 0.3333333333333333703, 0.3333333333333333703, 0.3333333333333333703, 0.3333333333333333703, 0.3333333333333333703, 0.3333333333333333703, 0.3333333333333333703, 0.3333333333333333703, 0.3333333333333333703, 0.3333333333333333703, 0.3333333333333333703, 0.3333333333333333703, 0.3333333333333333703, 0.3333333333333333703, 0.3333333333333333703, 0.3333333333333333703, 0.3333333333333333703, 0.3333333333333333703, 0.3333333333333333703, 0.3333333333333333703, 0.3333333333333333703, 0.3333333333333333703, 0.3333333333333333703, 0.3333333333333333703, 0.3333333333333333703, 0.3333333333333333703, 0.3333333333333333703, 0.3333333333333333703, 0.3333333333333333703, 0.3333333333333333703, 0.3333333333333333703, 0.3333333333333333703, 0.3333333333333333703, 0.3333333333333333703, 0.3333333333333333703, 0.3333333333333333703, 0.3333333333333333703, 0.3333333333333333703, 0.3333333333333333703, 0.3333333333333333703, 0.3333333333333333703, 0.3333333333333333703, 0.3333333333333333703, 0.3333333333333333703, 0.3333333333333333703, 0.3333333333333333703, 0.3333333333333333703, 0.3333333333333333703, 0.3333333333333333703, 0.3333333333333333703, 0.3333333333333333703, 0.3333333333333333703, 0.3333333333333333703, 0.3333333333333333703, 0.3333333333333333703, 0.3333333333333333703, 0.3333333333333333703, 0.3333333333333333703, 0.3333333333333333703, 0.3333333333333333703, 0.3333333333333333703, 0.3333333333333333703, 0.3333333333333333703, 0.3333333333333333703, 0.3333333333333333703, 0.3333333333333333703, 0.3333333333333333703, 0.3333333333333333703, 0.3333333333333333703, 0.3333333333333333703, 0.3333333333333333703, 0.3333333333333333703, 0.3333333333333333703, 0.3333333333333333703, 0.3333333333333333703, 0.3333333333333333703, 0.3333333333333333703, 0.3333333333333333703, 0.3333333333333333703, 0.3333333333333333703, 0.3333333333333333703, 0.3333333333333333703, 0.3333333333333333703, 0.3333333333333333703, 0.3333333333333333703, 0.3333333333333333703, 0.3333333333333333703, 0.3333333333333333703, 0.3333333333333333703, 0.3333333333333333703, 0.3333333333333333703, 0.3333333333333333703, 0.3333333333333333703, 0.3333333333333333703, 0.3333333333333333703, 0.3333333333333333703, 0.3333333333333333703, 0.3333333333333333703, 0.3333333333333333703, 0.3333333333333333703, 0.3333333333333333703, 0.3333333333333333703, 0.3333333333333333703, 0.3333333333333333703, 0.3333333333333333703, 0.3333333333333333703, 0.3333333333333333703, 0.3333333333333333703, 0.3333333333333333703, 0.3333333333333333703, 0.3333333333333333703, 0.3333333333333333703, 0.3333333333333333703, 0.3333333333333333703, 0.3333333333333333703, 0.3333333333333333703, 0.3333333333333333703, 0.3333333333333333703, 0.3333333333333333703, 0.3333333333333333703, 0.3333333333333333703, 0.3333333333333333703, 0.3333333333333333703, 0.3333333333333333703, 0.3333333333333333703, 0.3333333333333333703, 0.3333333333333333703, 0.3333333333333333703, 0.3333333333333333703, 0.3333333333333333703),
 ( 1.000000000000000000, 1.000000000000000000, 1.000000000000000000, 1.000000000000000000, 1.000000000000000000, 1.000000000000000000, 1.000000000000000000, 1.000000000000000000, 1.000000000000000000, 1.000000000000000000, 1.000000000000000000, 1.000000000000000000, 1.000000000000000000, 1.000000000000000000, 1.000000000000000000, 1.000000000000000000, 1.000000000000000000, 1.000000000000000000, 1.000000000000000000, 1.000000000000000000, 1.000000000000000000, 1.000000000000000000, 1.000000000000000000, 1.000000000000000000, 1.000000000000000000, 1.000000000000000000, 1.000000000000000000, 1.000000000000000000, 1.000000000000000000, 1.000000000000000000, 1.000000000000000000, 1.000000000000000000, 1.000000000000000000, 1.000000000000000000, 1.000000000000000000, 1.000000000000000000, 1.000000000000000000, 1.000000000000000000, 1.000000000000000000, 1.000000000000000000, 1.000000000000000000, 1.000000000000000000, 1.000000000000000000, 1.000000000000000000, 1.000000000000000000, 1.000000000000000000, 1.000000000000000000, 1.000000000000000000, 1.000000000000000000, 1.000000000000000000, 1.000000000000000000, 1.000000000000000000, 1.000000000000000000, 1.000000000000000000, 1.000000000000000000, 1.000000000000000000, 1.000000000000000000, 1.000000000000000000, 1.000000000000000000, 1.000000000000000000, 1.000000000000000000, 1.000000000000000000, 1.000000000000000000, 1.000000000000000000, 1.000000000000000000, 1.000000000000000000, 1.000000000000000000, 1.000000000000000000, 1.000000000000000000, 1.000000000000000000, 1.000000000000000000, 1.000000000000000000, 1.000000000000000000, 1.000000000000000000, 1.000000000000000000, 1.000000000000000000, 1.000000000000000000, 1.000000000000000000, 1.000000000000000000, 1.000000000000000000, 1.000000000000000000, 1.000000000000000000, 1.000000000000000000, 1.000000000000000000, 1.000000000000000000, 1.000000000000000000, 1.000000000000000000, 1.000000000000000000, 1.000000000000000000, 1.000000000000000000, 1.000000000000000000, 1.000000000000000000, 1.000000000000000000, 1.000000000000000000, 1.000000000000000000, 1.000000000000000000, 1.000000000000000000, 1.000000000000000000, 1.000000000000000000, 1.000000000000000000, 1.000000000000000000, 1.000000000000000000, 1.000000000000000000, 1.000000000000000000, 1.000000000000000000, 1.000000000000000000, 1.000000000000000000, 1.000000000000000000, 1.000000000000000000, 1.000000000000000000, 1.000000000000000000, 1.000000000000000000, 1.000000000000000000, 1.000000000000000000, 1.000000000000000000, 1.000000000000000000, 1.000000000000000000, 1.000000000000000000, 1.000000000000000000, 1.000000000000000000, 1.000000000000000000, 1.000000000000000000, 1.000000000000000000, 1.000000000000000000, 1.000000000000000000, 1.000000000000000000, 1.000000000000000000, 1.000000000000000000, 1.000000000000000000, 1.000000000000000000, 1.000000000000000000, 1.000000000000000000, 1.000000000000000000, 1.000000000000000000, 1.000000000000000000, 1.000000000000000000, 1.000000000000000000, 1.000000000000000000, 1.000000000000000000, 1.000000000000000000, 1.000000000000000000, 1.000000000000000000, 1.000000000000000000, 1.000000000000000000, 1.000000000000000000, 1.000000000000000000, 1.000000000000000000, 1.000000000000000000, 1.000000000000000000, 1.000000000000000000, 1.000000000000000000, 1.000000000000000000, 1.000000000000000000, 1.000000000000000000, 1.000000000000000000, 1.000000000000000000, 1.000000000000000000, 1.000000000000000000),
 ( 0.3333333333333333703, 0.3333333333333333703, 0.3333333333333333703, 0.3333333333333333703, 0.3333333333333333703, 0.3333333333333333703, 0.3333333333333333703, 0.3333333333333333703, 0.3333333333333333703, 0.3333333333333333703, 0.3333333333333333703, 0.3333333333333333703, 0.3333333333333333703, 0.3333333333333333703, 0.3333333333333333703, 0.3333333333333333703, 0.3333333333333333703, 0.3333333333333333703, 0.3333333333333333703, 0.3333333333333333703, 0.3333333333333333703, 0.3333333333333333703, 0.3333333333333333703, 0.3333333333333333703, 0.3333333333333333703, 0.3333333333333333703, 0.3333333333333333703, 0.3333333333333333703, 0.3333333333333333703, 0.3333333333333333703, 0.3333333333333333703, 0.3333333333333333703, 0.3333333333333333703, 0.3333333333333333703, 0.3333333333333333703, 0.3333333333333333703, 0.3333333333333333703, 0.3333333333333333703, 0.3333333333333333703, 0.3333333333333333703, 0.3333333333333333703, 0.3333333333333333703, 0.3333333333333333703, 0.3333333333333333703, 0.3333333333333333703, 0.3333333333333333703, 0.3333333333333333703, 0.3333333333333333703, 0.3333333333333333703, 0.3333333333333333703, 0.3333333333333333703, 0.3333333333333333703, 0.3333333333333333703, 0.3333333333333333703, 0.3333333333333333703, 0.3333333333333333703, 0.3333333333333333703, 0.3333333333333333703, 0.3333333333333333703, 0.3333333333333333703, 0.3333333333333333703, 0.3333333333333333703, 0.3333333333333333703, 0.3333333333333333703, 0.3333333333333333703, 0.3333333333333333703, 0.3333333333333333703, 0.3333333333333333703, 0.3333333333333333703, 0.3333333333333333703, 0.3333333333333333703, 0.3333333333333333703, 0.3333333333333333703, 0.3333333333333333703, 0.3333333333333333703, 0.3333333333333333703, 0.3333333333333333703, 0.3333333333333333703, 0.3333333333333333703, 0.3333333333333333703, 0.3333333333333333703, 0.3333333333333333703, 0.3333333333333333703, 0.3333333333333333703, 0.3333333333333333703, 0.3333333333333333703, 0.3333333333333333703, 0.3333333333333333703, 0.3333333333333333703, 0.3333333333333333703, 0.3333333333333333703, 0.3333333333333333703, 0.3333333333333333703, 0.3333333333333333703, 0.3333333333333333703, 0.3333333333333333703, 0.3333333333333333703, 0.3333333333333333703, 0.3333333333333333703, 0.3333333333333333703, 0.3333333333333333703, 0.3333333333333333703, 0.3333333333333333703, 0.3333333333333333703, 0.3333333333333333703, 0.3333333333333333703, 0.3333333333333333703, 0.3333333333333333703, 0.3333333333333333703, 0.3333333333333333703, 0.3333333333333333703, 0.3333333333333333703, 0.3333333333333333703, 0.3333333333333333703, 0.3333333333333333703, 0.3333333333333333703, 0.3333333333333333703, 0.3333333333333333703, 0.3333333333333333703, 0.3333333333333333703, 0.3333333333333333703, 0.3333333333333333703, 0.3333333333333333703, 0.3333333333333333703, 0.3333333333333333703, 0.3333333333333333703, 0.3333333333333333703, 0.3333333333333333703, 0.3333333333333333703, 0.3333333333333333703, 0.3333333333333333703, 0.3333333333333333703, 0.3333333333333333703, 0.3333333333333333703, 0.3333333333333333703, 0.3333333333333333703, 0.3333333333333333703, 0.3333333333333333703, 0.3333333333333333703, 0.3333333333333333703, 0.3333333333333333703, 0.3333333333333333703, 0.3333333333333333703, 0.3333333333333333703, 0.3333333333333333703, 0.3333333333333333703, 0.3333333333333333703, 0.3333333333333333703, 0.3333333333333333703, 0.3333333333333333703, 0.3333333333333333703, 0.3333333333333333703, 0.3333333333333333703, 0.3333333333333333703, 0.3333333333333333703, 0.3333333333333333703, 0.3333333333333333703, 0.3333333333333333703),
 ( 0.3333333333333333703, 0.3333333333333333703, 0.3333333333333333703, 0.3333333333333333703, 0.3333333333333333703, 0.3333333333333333703, 0.3333333333333333703, 0.3333333333333333703, 0.3333333333333333703, 0.3333333333333333703, 0.3333333333333333703, 0.3333333333333333703, 0.3333333333333333703, 0.3333333333333333703, 0.3333333333333333703, 0.3333333333333333703, 0.3333333333333333703, 0.3333333333333333703, 0.3333333333333333703, 0.3333333333333333703, 0.3333333333333333703, 0.3333333333333333703, 0.3333333333333333703, 0.3333333333333333703, 0.3333333333333333703, 0.3333333333333333703, 0.3333333333333333703, 0.3333333333333333703, 0.3333333333333333703, 0.3333333333333333703, 0.3333333333333333703, 0.3333333333333333703, 0.3333333333333333703, 0.3333333333333333703, 0.3333333333333333703, 0.3333333333333333703, 0.3333333333333333703, 0.3333333333333333703, 0.3333333333333333703, 0.3333333333333333703, 0.3333333333333333703, 0.3333333333333333703, 0.3333333333333333703, 0.3333333333333333703, 0.3333333333333333703, 0.3333333333333333703, 0.3333333333333333703, 0.3333333333333333703, 0.3333333333333333703, 0.3333333333333333703, 0.3333333333333333703, 0.3333333333333333703, 0.3333333333333333703, 0.3333333333333333703, 0.3333333333333333703, 0.3333333333333333703, 0.3333333333333333703, 0.3333333333333333703, 0.3333333333333333703, 0.3333333333333333703, 0.3333333333333333703, 0.3333333333333333703, 0.3333333333333333703, 0.3333333333333333703, 0.3333333333333333703, 0.3333333333333333703, 0.3333333333333333703, 0.3333333333333333703, 0.3333333333333333703, 0.3333333333333333703, 0.3333333333333333703, 0.3333333333333333703, 0.3333333333333333703, 0.3333333333333333703, 0.3333333333333333703, 0.3333333333333333703, 0.3333333333333333703, 0.3333333333333333703, 0.3333333333333333703, 0.3333333333333333703, 0.3333333333333333703, 0.3333333333333333703, 0.3333333333333333703, 0.3333333333333333703, 0.3333333333333333703, 0.3333333333333333703, 0.3333333333333333703, 0.3333333333333333703, 0.3333333333333333703, 0.3333333333333333703, 0.3333333333333333703, 0.3333333333333333703, 0.3333333333333333703, 0.3333333333333333703, 0.3333333333333333703, 0.3333333333333333703, 0.3333333333333333703, 0.3333333333333333703, 0.3333333333333333703, 0.3333333333333333703, 0.3333333333333333703, 0.3333333333333333703, 0.3333333333333333703, 0.3333333333333333703, 0.3333333333333333703, 0.3333333333333333703, 0.3333333333333333703, 0.3333333333333333703, 0.3333333333333333703, 0.3333333333333333703, 0.3333333333333333703, 0.3333333333333333703, 0.3333333333333333703, 0.3333333333333333703, 0.3333333333333333703, 0.3333333333333333703, 0.3333333333333333703, 0.3333333333333333703, 0.3333333333333333703, 0.3333333333333333703, 0.3333333333333333703, 0.3333333333333333703, 0.3333333333333333703, 0.3333333333333333703, 0.3333333333333333703, 0.3333333333333333703, 0.3333333333333333703, 0.3333333333333333703, 0.3333333333333333703, 0.3333333333333333703, 0.3333333333333333703, 0.3333333333333333703, 0.3333333333333333703, 0.3333333333333333703, 0.3333333333333333703, 0.3333333333333333703, 0.3333333333333333703, 0.3333333333333333703, 0.3333333333333333703, 0.3333333333333333703, 0.3333333333333333703, 0.3333333333333333703, 0.3333333333333333703, 0.3333333333333333703, 0.3333333333333333703, 0.3333333333333333703, 0.3333333333333333703, 0.3333333333333333703, 0.3333333333333333703, 0.3333333333333333703, 0.3333333333333333703, 0.3333333333333333703, 0.3333333333333333703, 0.3333333333333333703, 0.3333333333333333703, 0.3333333333333333703, 0.3333333333333333703, 0.3333333333333333703),
 ( 1.000000000000000000, 1.000000000000000000, 1.000000000000000000, 1.000000000000000000, 1.000000000000000000, 1.000000000000000000, 1.000000000000000000, 1.000000000000000000, 1.000000000000000000, 1.000000000000000000, 1.000000000000000000, 1.000000000000000000, 1.000000000000000000, 1.000000000000000000, 1.000000000000000000, 1.000000000000000000, 1.000000000000000000, 1.000000000000000000, 1.000000000000000000, 1.000000000000000000, 1.000000000000000000, 1.000000000000000000, 1.000000000000000000, 1.000000000000000000, 1.000000000000000000, 1.000000000000000000, 1.000000000000000000, 1.000000000000000000, 1.000000000000000000, 1.000000000000000000, 1.000000000000000000, 1.000000000000000000, 1.000000000000000000, 1.000000000000000000, 1.000000000000000000, 1.000000000000000000, 1.000000000000000000, 1.000000000000000000, 1.000000000000000000, 1.000000000000000000, 1.000000000000000000, 1.000000000000000000, 1.000000000000000000, 1.000000000000000000, 1.000000000000000000, 1.000000000000000000, 1.000000000000000000, 1.000000000000000000, 1.000000000000000000, 1.000000000000000000, 1.000000000000000000, 1.000000000000000000, 1.000000000000000000, 1.000000000000000000, 1.000000000000000000, 1.000000000000000000, 1.000000000000000000, 1.000000000000000000, 1.000000000000000000, 1.000000000000000000, 1.000000000000000000, 1.000000000000000000, 1.000000000000000000, 1.000000000000000000, 1.000000000000000000, 1.000000000000000000, 1.000000000000000000, 1.000000000000000000, 1.000000000000000000, 1.000000000000000000, 1.000000000000000000, 1.000000000000000000, 1.000000000000000000, 1.000000000000000000, 1.000000000000000000, 1.000000000000000000, 1.000000000000000000, 1.000000000000000000, 1.000000000000000000, 1.000000000000000000, 1.000000000000000000, 1.000000000000000000, 1.000000000000000000, 1.000000000000000000, 1.000000000000000000, 1.000000000000000000, 1.000000000000000000, 1.000000000000000000, 1.000000000000000000, 1.000000000000000000, 1.000000000000000000, 1.000000000000000000, 1.000000000000000000, 1.000000000000000000, 1.000000000000000000, 1.000000000000000000, 1.000000000000000000, 1.000000000000000000, 1.000000000000000000, 1.000000000000000000, 1.000000000000000000, 1.000000000000000000, 1.000000000000000000, 1.000000000000000000, 1.000000000000000000, 1.000000000000000000, 1.000000000000000000, 1.000000000000000000, 1.000000000000000000, 1.000000000000000000, 1.000000000000000000, 1.000000000000000000, 1.000000000000000000, 1.000000000000000000, 1.000000000000000000, 1.000000000000000000, 1.000000000000000000, 1.000000000000000000, 1.000000000000000000, 1.000000000000000000, 1.000000000000000000, 1.000000000000000000, 1.000000000000000000, 1.000000000000000000, 1.000000000000000000, 1.000000000000000000, 1.000000000000000000, 1.000000000000000000, 1.000000000000000000, 1.000000000000000000, 1.000000000000000000, 1.000000000000000000, 1.000000000000000000, 1.000000000000000000, 1.000000000000000000, 1.000000000000000000, 1.000000000000000000, 1.000000000000000000, 1.000000000000000000, 1.000000000000000000, 1.000000000000000000, 1.000000000000000000, 1.000000000000000000, 1.000000000000000000, 1.000000000000000000, 1.000000000000000000, 1.000000000000000000, 1.000000000000000000, 1.000000000000000000, 1.000000000000000000, 1.000000000000000000, 1.000000000000000000, 1.000000000000000000, 1.000000000000000000, 1.000000000000000000, 1.000000000000000000, 1.000000000000000000, 1.000000000000000000) ) ) 
 REPRESENTATION_ITEM ( '' )  SURFACE ( )  );
#2961 = LINE ( 'NONE', #586, #6281 ) ;
#2962 = CARTESIAN_POINT ( 'NONE',  ( -35.50000000000000000, -113.9929510916434339, 10.50625754673586876 ) ) ;
#2963 = CARTESIAN_POINT ( 'NONE',  ( 46.00000000000000000, 9.797174393178845379E-16, 78.00000000000001421 ) ) ;
#2964 = CARTESIAN_POINT ( 'NONE',  ( -46.00000000000000000, 0.000000000000000000, 8.000000000000000000 ) ) ;
#2965 = TOROIDAL_SURFACE ( 'NONE', #4122, 7.800000000000023803, 0.2000000000000003164 ) ;
#2966 = COLOUR_RGB ( '', 0.31764706, 0.68627451, 0.89019608) ;
#2967 = AXIS2_PLACEMENT_3D ( 'NONE', #12771, #21216, #15618 ) ;
#2968 = CARTESIAN_POINT ( 'NONE',  ( -34.50000000000000000, -112.9611193698460738, 2.883091707513499635 ) ) ;
#2969 = ADVANCED_FACE ( 'NONE', ( #34644 ), #29055, .T. ) ;
#2970 = CARTESIAN_POINT ( 'NONE',  ( -39.00000000000000000, -115.9929510916434481, 12.56351784598954779 ) ) ;
#2971 = FACE_OUTER_BOUND ( 'NONE', #8027, .T. ) ;
#2972 = EDGE_CURVE ( 'NONE', #32704, #32451, #15526, .T. ) ;
#2973 = CARTESIAN_POINT ( 'NONE',  ( -36.49999999999999289, -11.52052244843579309, 115.1848168619253698 ) ) ;
#2974 = PRODUCT_DEFINITION_SHAPE ( 'NONE', 'NONE',  #35643 ) ;
#2975 = ORIENTED_EDGE ( 'NONE', *, *, #1380, .T. ) ;
#2976 = CARTESIAN_POINT ( 'NONE',  ( -35.50000000000000711, -114.3464919575557843, 9.568884482464163455 ) ) ;
#2977 = DIRECTION ( 'NONE',  ( -1.000000000000000000, -1.817026393327835042E-30, 1.734723475976807094E-16 ) ) ;
#2978 = FILL_AREA_STYLE_COLOUR ( '', #129 ) ;
#2979 = DIRECTION ( 'NONE',  ( 0.000000000000000000, 0.000000000000000000, 1.000000000000000000 ) ) ;
#2980 = ORIENTED_EDGE ( 'NONE', *, *, #9162, .T. ) ;
#2981 = DIRECTION ( 'NONE',  ( 1.000000000000000000, 1.836970198721029934E-16, 0.000000000000000000 ) ) ;
#2982 = LINE ( 'NONE', #27982, #7786 ) ;
#2983 = LINE ( 'NONE', #32683, #25157 ) ;
#2984 = CARTESIAN_POINT ( 'NONE',  ( 0.1717365941144993746, -6.008326913195982222, 0.000000000000000000 ) ) ;
#2985 = EDGE_CURVE ( 'NONE', #24079, #15022, #11695, .T. ) ;
#2986 = EDGE_CURVE ( 'NONE', #23201, #9658, #1674, .T. ) ;
#2987 = FACE_OUTER_BOUND ( 'NONE', #6987, .T. ) ;
#2988 = CARTESIAN_POINT ( 'NONE',  ( -44.00199999999999534, 14.29999999999999893, 3.000000000000002665 ) ) ;
#2989 = EDGE_LOOP ( 'NONE', ( #17604, #28300, #12736, #33040 ) ) ;
#2990 = DIRECTION ( 'NONE',  ( 0.000000000000000000, 0.000000000000000000, 1.000000000000000000 ) ) ;
#2991 = DIRECTION ( 'NONE',  ( -1.000000000000000000, 0.000000000000000000, 0.000000000000000000 ) ) ;
#2992 = DIRECTION ( 'NONE',  ( 0.000000000000000000, 0.000000000000000000, -1.000000000000000000 ) ) ;
#2993 = ORIENTED_EDGE ( 'NONE', *, *, #857, .T. ) ;
#2994 = CARTESIAN_POINT ( 'NONE',  ( -36.94073759706868287, -115.0000000000000000, 7.371475545821551734 ) ) ;
#2995 = ORIENTED_EDGE ( 'NONE', *, *, #14778, .F. ) ;
#2996 = CIRCLE ( 'NONE', #22511, 19.99999999999998579 ) ;
#2997 = AXIS2_PLACEMENT_3D ( 'NONE', #14692, #34519, #34159 ) ;
#2998 = ORIENTED_EDGE ( 'NONE', *, *, #27190, .T. ) ;
#2999 = EDGE_LOOP ( 'NONE', ( #33499, #12810, #10509, #20341 ) ) ;
#3000 = CARTESIAN_POINT ( 'NONE',  ( 4.000000000000003553, -0.6505223195679143977, -51.99593080916758936 ) ) ;
#3001 = APPLICATION_CONTEXT ( 'automotive_design' ) ;
#3002 = DIRECTION ( 'NONE',  ( 0.000000000000000000, 0.000000000000000000, 1.000000000000000000 ) ) ;
#3003 = VECTOR ( 'NONE', #14853, 1000.000000000000114 ) ;
#3004 = CARTESIAN_POINT ( 'NONE',  ( -35.50000000000000711, -114.6604609523327838, 9.751889438017201428 ) ) ;
#3005 = LINE ( 'NONE', #19693, #30450 ) ;
#3006 = DIRECTION ( 'NONE',  ( 0.000000000000000000, 0.000000000000000000, 1.000000000000000000 ) ) ;
#3007 = DIRECTION ( 'NONE',  ( -1.000000000000000000, 5.339440136655842133E-16, -1.047965281155515476E-16 ) ) ;
#3008 = DIRECTION ( 'NONE',  ( -1.000000000000000000, -0.000000000000000000, 0.000000000000000000 ) ) ;
#3009 = EDGE_CURVE ( 'NONE', #6246, #26745, #775, .T. ) ;
#3010 = CARTESIAN_POINT ( 'NONE',  ( 8.000000000000007105, 13.61301047812919052, -3.268936481846215880 ) ) ;
#3011 = AXIS2_PLACEMENT_3D ( 'NONE', #7848, #24423, #35412 ) ;
#3012 = STYLED_ITEM ( 'NONE', ( #182 ), #2239 ) ;
#3013 = CARTESIAN_POINT ( 'NONE',  ( -38.25557080230232998, -115.9929510916434481, 13.92914543265419525 ) ) ;
#3015 = DIRECTION ( 'NONE',  ( -1.000000000000000000, 1.110223024625156540E-16, 0.000000000000000000 ) ) ;
#3014 = AXIS2_PLACEMENT_3D ( 'NONE', #459, #28008, #25304 ) ;
#3016 = CYLINDRICAL_SURFACE ( 'NONE', #35475, 12.55910585664918422 ) ;
#3017 = CARTESIAN_POINT ( 'NONE',  ( 0.000000000000000000, -14.80634052301617309, -8.177498406287382338 ) ) ;
#3018 = DIRECTION ( 'NONE',  ( 1.000000000000000000, -1.110223024625156540E-16, 0.000000000000000000 ) ) ;
#3019 = PLANE ( 'NONE',  #23978 ) ;
#3020 = CYLINDRICAL_SURFACE ( 'NONE', #14368, 8.000000000000001776 ) ;
#3021 = VERTEX_POINT ( 'NONE', #9766 ) ;
#3022 = CARTESIAN_POINT ( 'NONE',  ( -36.94073759706868287, -115.9999999999999858, 7.371475545821551734 ) ) ;
#3023 = FACE_OUTER_BOUND ( 'NONE', #30000, .T. ) ;
#3024 = DIRECTION ( 'NONE',  ( 0.000000000000000000, 0.000000000000000000, -1.000000000000000000 ) ) ;
#3025 = DIRECTION ( 'NONE',  ( 1.110223024625156540E-16, 1.000000000000000000, 0.000000000000000000 ) ) ;
#3026 = ORIENTED_EDGE ( 'NONE', *, *, #15289, .F. ) ;
#3027 = CIRCLE ( 'NONE', #7599, 7.000000000000035527 ) ;
#3028 = VERTEX_POINT ( 'NONE', #17497 ) ;
#3029 = CARTESIAN_POINT ( 'NONE',  ( 8.000000000000000000, 0.000000000000000000, 0.000000000000000000 ) ) ;
#3030 = DIRECTION ( 'NONE',  ( -1.000000000000000000, 0.000000000000000000, 0.000000000000000000 ) ) ;
#3031 = ORIENTED_EDGE ( 'NONE', *, *, #3176, .T. ) ;
#3032 = ORIENTED_EDGE ( 'NONE', *, *, #17647, .T. ) ;
#3033 = LINE ( 'NONE', #19395, #219 ) ;
#3034 = DIRECTION ( 'NONE',  ( -1.000000000000000000, 0.000000000000000000, 0.000000000000000000 ) ) ;
#3035 = AXIS2_PLACEMENT_3D ( 'NONE', #15538, #32300, #7620 ) ;
#3036 = DIRECTION ( 'NONE',  ( -1.000000000000000000, 0.000000000000000000, 0.000000000000000000 ) ) ;
#3037 = VERTEX_POINT ( 'NONE', #17856 ) ;
#3038 = ORIENTED_EDGE ( 'NONE', *, *, #18067, .F. ) ;
#3039 = CARTESIAN_POINT ( 'NONE',  ( 2.000000000000001776, 7.800000000000029132, 3.469446951953614189E-15 ) ) ;
#3040 = LINE ( 'NONE', #668, #33918 ) ;
#3041 = ORIENTED_EDGE ( 'NONE', *, *, #27315, .F. ) ;
#3042 = CARTESIAN_POINT ( 'NONE',  ( 46.00000000000000000, 0.000000000000000000, 0.000000000000000000 ) ) ;
#3043 = AXIS2_PLACEMENT_3D ( 'NONE', #26710, #10316, #29585 ) ;
#3044 = CARTESIAN_POINT ( 'NONE',  ( -34.50000000000000000, -112.0460568841087223, -0.8839717462762063382 ) ) ;
#3045 = VECTOR ( 'NONE', #27840, 1000.000000000000000 ) ;
#3046 = EDGE_CURVE ( 'NONE', #30129, #2544, #14561, .T. ) ;
#3047 = CARTESIAN_POINT ( 'NONE',  ( -35.87745010033553683, -114.9929510916434339, 14.11371147303761298 ) ) ;
#3048 = AXIS2_PLACEMENT_3D ( 'NONE', #11758, #3330, #33731 ) ;
#3049 = CARTESIAN_POINT ( 'NONE',  ( -38.00000000000000711, -114.9929510916434339, 12.59102132592608925 ) ) ;
#3050 = DIRECTION ( 'NONE',  ( -1.000000000000000000, -0.000000000000000000, 0.000000000000000000 ) ) ;
#3051 = CARTESIAN_POINT ( 'NONE',  ( -35.07817881376918479, -114.9929510916434339, 13.81802396319203297 ) ) ;
#3052 = CARTESIAN_POINT ( 'NONE',  ( 0.000000000000000000, -44.25018368420762016, 27.31155879685168131 ) ) ;
#3053 = ORIENTED_EDGE ( 'NONE', *, *, #8030, .T. ) ;
#3054 = CARTESIAN_POINT ( 'NONE',  ( 8.000000000000000000, -6.359167119270333401, -18.96209359615098577 ) ) ;
#3055 = DIRECTION ( 'NONE',  ( -1.000000000000000000, 0.000000000000000000, 0.000000000000000000 ) ) ;
#3056 = DIRECTION ( 'NONE',  ( 0.000000000000000000, 0.000000000000000000, 1.000000000000000000 ) ) ;
#3057 = LINE ( 'NONE', #518, #22680 ) ;
#3058 = AXIS2_PLACEMENT_3D ( 'NONE', #21859, #4960, #29980 ) ;
#3059 = ORIENTED_EDGE ( 'NONE', *, *, #17897, .F. ) ;
#3060 = AXIS2_PLACEMENT_3D ( 'NONE', #18702, #24477, #4702 ) ;
#3061 = DIRECTION ( 'NONE',  ( 8.708451184622495809E-17, -6.938893903907203726E-17, -1.000000000000000000 ) ) ;
#3062 = ORIENTED_EDGE ( 'NONE', *, *, #8553, .T. ) ;
#3063 = EDGE_CURVE ( 'NONE', #28711, #5428, #718, .T. ) ;
#3064 = AXIS2_PLACEMENT_3D ( 'NONE', #22052, #14116, #16986 ) ;
#3065 = CARTESIAN_POINT ( 'NONE',  ( -34.83677480945819838, -111.9205845034225462, 7.316024454178450043 ) ) ;
#3066 = LINE ( 'NONE', #10984, #34199 ) ;
#3067 = CARTESIAN_POINT ( 'NONE',  ( -35.50000000000000711, -112.0140978167138712, -0.3122823525984337878 ) ) ;
#3068 = ORIENTED_EDGE ( 'NONE', *, *, #6816, .T. ) ;
#3069 = ORIENTED_EDGE ( 'NONE', *, *, #32265, .T. ) ;
#3070 = LINE ( 'NONE', #25557, #11972 ) ;
#3071 = CARTESIAN_POINT ( 'NONE',  ( 0.000000000000000000, -2.710505431213761085E-17, -45.10000000000000142 ) ) ;
#3072 = ORIENTED_EDGE ( 'NONE', *, *, #16909, .F. ) ;
#3073 = CIRCLE ( 'NONE', #23781, 3.799999999999999822 ) ;
#3074 = AXIS2_PLACEMENT_3D ( 'NONE', #18258, #29261, #14847 ) ;
#3075 = DIRECTION ( 'NONE',  ( -1.000000000000000000, -0.000000000000000000, -0.000000000000000000 ) ) ;
#3076 = CARTESIAN_POINT ( 'NONE',  ( -37.49999999999999289, -11.52052244843579309, 115.1848168619253698 ) ) ;
#3078 = ORIENTED_EDGE ( 'NONE', *, *, #22725, .T. ) ;
#3077 = COLOUR_RGB ( '', 0.31764706, 0.68627451, 0.89019608) ;
#3079 = ORIENTED_EDGE ( 'NONE', *, *, #5513, .T. ) ;
#3080 = CARTESIAN_POINT ( 'NONE',  ( 0.000000000000000000, 17.47118961583601404, -0.9861715913088251462 ) ) ;
#3081 = ADVANCED_FACE ( 'NONE', ( #12656 ), #34449, .T. ) ;
#3082 = LINE ( 'NONE', #11689, #19011 ) ;
#3083 = ORIENTED_EDGE ( 'NONE', *, *, #14355, .T. ) ;
#3084 = VERTEX_POINT ( 'NONE', #1137 ) ;
#3085 = CARTESIAN_POINT ( 'NONE',  ( -35.50000000000000000, -112.8920926830253677, 2.874852253704053062 ) ) ;
#3086 = AXIS2_PLACEMENT_3D ( 'NONE', #9014, #22341, #11712 ) ;
#3087 = CARTESIAN_POINT ( 'NONE',  ( 7.999999999999992895, 5.667686777401707232, 46.64153600743606631 ) ) ;
#3088 = ORIENTED_EDGE ( 'NONE', *, *, #10237, .F. ) ;
#3089 = CARTESIAN_POINT ( 'NONE',  ( -35.50000000000000711, -114.9929510916434339, 12.60752341388803544 ) ) ;
#3090 = ADVANCED_FACE ( 'NONE', ( #3845 ), #1879, .T. ) ;
#3091 = CARTESIAN_POINT ( 'NONE',  ( -34.50120407906360498, -113.9929510916434339, 12.67985367974112343 ) ) ;
#3092 = ADVANCED_FACE ( 'NONE', ( #31373 ), #30043, .T. ) ;
#3093 = CARTESIAN_POINT ( 'NONE',  ( -34.49999999999998579, -37.28532556477434667, 76.74125644078563369 ) ) ;
#3094 = EDGE_CURVE ( 'NONE', #19486, #16196, #9900, .T. ) ;
#3095 = CARTESIAN_POINT ( 'NONE',  ( -34.50000000000000000, -113.9929510916434339, 10.52826033068511435 ) ) ;
#3096 = CARTESIAN_POINT ( 'NONE',  ( 0.000000000000000000, -36.34385289850609979, 29.77717097092063980 ) ) ;
#3097 = CARTESIAN_POINT ( 'NONE',  ( -35.50000000000000711, -114.9922651054798308, 10.46846006712531008 ) ) ;
#3098 = DIRECTION ( 'NONE',  ( 1.000000000000000000, 0.000000000000000000, 0.000000000000000000 ) ) ;
#3099 = AXIS2_PLACEMENT_3D ( 'NONE', #15061, #18124, #2135 ) ;
#3100 = CIRCLE ( 'NONE', #11135, 7.199999999999993960 ) ;
#3101 = LINE ( 'NONE', #25050, #12956 ) ;
#3102 = EDGE_LOOP ( 'NONE', ( #5630, #4974, #16989, #17044 ) ) ;
#3103 = VERTEX_POINT ( 'NONE', #29030 ) ;
#3104 = EDGE_CURVE ( 'NONE', #28091, #14794, #34078, .T. ) ;
#3105 = CARTESIAN_POINT ( 'NONE',  ( 50.00005079999998969, 10.58300524425836109, -3.000000000000002665 ) ) ;
#3106 = DIRECTION ( 'NONE',  ( 1.000000000000000000, -0.000000000000000000, -0.000000000000000000 ) ) ;
#3107 = EDGE_CURVE ( 'NONE', #10099, #28443, #12794, .T. ) ;
#3108 = EDGE_LOOP ( 'NONE', ( #13392, #17439, #19443, #29588 ) ) ;
#3109 = DIRECTION ( 'NONE',  ( 0.000000000000000000, 0.5877852522924739143, -0.8090169943749468962 ) ) ;
#3110 = ORIENTED_EDGE ( 'NONE', *, *, #18733, .T. ) ;
#3111 = CIRCLE ( 'NONE', #19738, 4.000000000000000000 ) ;
#3112 = AXIS2_PLACEMENT_3D ( 'NONE', #28363, #1007, #33578 ) ;
#3113 = CARTESIAN_POINT ( 'NONE',  ( -35.50000000000000000, -113.0140978167138712, -0.4685323525984296800 ) ) ;
#3114 = CARTESIAN_POINT ( 'NONE',  ( 4.000000000000003553, -15.92965478239629817, 15.17386234660378008 ) ) ;
#3115 = CARTESIAN_POINT ( 'NONE',  ( -37.76916472181487450, -111.9754527089670404, 4.034774454178449155 ) ) ;
#3116 = CARTESIAN_POINT ( 'NONE',  ( 0.000000000000000000, -19.44205635905512608, -43.33776004284631256 ) ) ;
#3117 = ORIENTED_EDGE ( 'NONE', *, *, #23985, .F. ) ;
#3118 = CARTESIAN_POINT ( 'NONE',  ( -35.50000000000000711, -112.0250551866464548, 1.025914454044489332 ) ) ;
#3119 = VERTEX_POINT ( 'NONE', #6703 ) ;
#3120 = ORIENTED_EDGE ( 'NONE', *, *, #29084, .F. ) ;
#3121 = CARTESIAN_POINT ( 'NONE',  ( -37.76916472181487450, -111.9754527089670404, 7.034774454178450931 ) ) ;
#3122 = EDGE_CURVE ( 'NONE', #18111, #31582, #15324, .T. ) ;
#3123 = SHAPE_REPRESENTATION_RELATIONSHIP ( 'NONE' , 'NONE' ,  #31430, #19774 ) ;
#3124 = CARTESIAN_POINT ( 'NONE',  ( 0.000000000000000000, 35.11945359308111847, 38.34871548466026070 ) ) ;
#3125 = ORIENTED_EDGE ( 'NONE', *, *, #31259, .T. ) ;
#3126 = ORIENTED_EDGE ( 'NONE', *, *, #33275, .F. ) ;
#3127 = CARTESIAN_POINT ( 'NONE',  ( -34.50000000000000000, -112.4434344552011282, 1.705278471174987986 ) ) ;
#3128 = LINE ( 'NONE', #14606, #28088 ) ;
#3129 = PRODUCT_DEFINITION ( 'UNKNOWN', '', #8615, #761 ) ;
#3130 = CARTESIAN_POINT ( 'NONE',  ( 8.000000000000000000, -18.48663108841356717, 4.615718728111985136 ) ) ;
#3131 = EDGE_CURVE ( 'NONE', #13387, #5141, #19671, .T. ) ;
#3132 = CARTESIAN_POINT ( 'NONE',  ( -35.50000000000000000, -113.9929510916434339, 10.72628538622835670 ) ) ;
#3133 = VECTOR ( 'NONE', #26486, 1000.000000000000000 ) ;
#3134 = CARTESIAN_POINT ( 'NONE',  ( -39.49999999999999289, -9.059673409587547965, 113.4689433211305811 ) ) ;
#3135 = ADVANCED_FACE ( 'NONE', ( #28683 ), #4570, .T. ) ;
#3136 = DIRECTION ( 'NONE',  ( -1.000000000000000000, 8.604228440844963188E-16, 0.000000000000000000 ) ) ;
#3137 = EDGE_CURVE ( 'NONE', #34977, #23819, #3596, .T. ) ;
#3138 = CARTESIAN_POINT ( 'NONE',  ( -34.50000000000000000, -116.0140978167138712, -0.4685323525984310677 ) ) ;
#3139 = CARTESIAN_POINT ( 'NONE',  ( -38.69949915733018742, -115.9929510916434481, 13.54034599209165890 ) ) ;
#3140 = DIRECTION ( 'NONE',  ( -1.000000000000000000, 0.000000000000000000, 0.000000000000000000 ) ) ;
#3141 = DIRECTION ( 'NONE',  ( -1.000000000000000000, 0.000000000000000000, 0.000000000000000000 ) ) ;
#3142 = ORIENTED_EDGE ( 'NONE', *, *, #28661, .T. ) ;
#3143 = DIRECTION ( 'NONE',  ( -1.000000000000000000, -0.000000000000000000, -0.000000000000000000 ) ) ;
#3144 = DIRECTION ( 'NONE',  ( 0.000000000000000000, 1.000000000000000000, 0.000000000000000000 ) ) ;
#3145 = CYLINDRICAL_SURFACE ( 'NONE', #12822, 22.00000000000000000 ) ;
#3146 = EDGE_CURVE ( 'NONE', #23782, #28075, #12829, .T. ) ;
#3147 = VECTOR ( 'NONE', #25455, 1000.000000000000000 ) ;
#3148 = ORIENTED_EDGE ( 'NONE', *, *, #13055, .F. ) ;
#3149 = CARTESIAN_POINT ( 'NONE',  ( 4.000000000000003553, 9.637487275701115408, 10.15474465512054181 ) ) ;
#3150 = CARTESIAN_POINT ( 'NONE',  ( -29.99999999999999645, -27.99999999999999289, 113.9999999999999858 ) ) ;
#3151 = FACE_OUTER_BOUND ( 'NONE', #30786, .T. ) ;
#3152 = DIRECTION ( 'NONE',  ( 1.541976423090495140E-16, -1.000000000000000000, 0.000000000000000000 ) ) ;
#3153 = PLANE ( 'NONE',  #7233 ) ;
#3154 = CARTESIAN_POINT ( 'NONE',  ( 26.99999999999999289, 20.00000000000000711, 2.449293598294706513E-15 ) ) ;
#3155 = ORIENTED_EDGE ( 'NONE', *, *, #32670, .T. ) ;
#3156 = AXIS2_PLACEMENT_3D ( 'NONE', #20079, #22969, #1029 ) ;
#3157 = DIRECTION ( 'NONE',  ( 0.000000000000000000, 0.000000000000000000, 1.000000000000000000 ) ) ;
#3158 = VECTOR ( 'NONE', #26077, 1000.000000000000000 ) ;
#3159 = DIRECTION ( 'NONE',  ( -1.000000000000000000, -0.000000000000000000, -0.000000000000000000 ) ) ;
#3160 = CARTESIAN_POINT ( 'NONE',  ( 7.999999999999992895, -8.053585752062238257, 46.81126742072021329 ) ) ;
#3161 = ORIENTED_EDGE ( 'NONE', *, *, #26875, .F. ) ;
#3162 = CARTESIAN_POINT ( 'NONE',  ( -38.02454729103295961, -113.6450488405582462, 4.840225545821551734 ) ) ;
#3163 = ORIENTED_EDGE ( 'NONE', *, *, #21065, .T. ) ;
#3164 = EDGE_CURVE ( 'NONE', #23592, #17129, #34256, .T. ) ;
#3165 = AXIS2_PLACEMENT_3D ( 'NONE', #18183, #21055, #4543 ) ;
#3166 =( LENGTH_UNIT ( ) NAMED_UNIT ( * ) SI_UNIT ( .MILLI., .METRE. ) );
#3167 = EDGE_LOOP ( 'NONE', ( #19715, #27036, #1388, #15787 ) ) ;
#3168 = VERTEX_POINT ( 'NONE', #31558 ) ;
#3169 = CARTESIAN_POINT ( 'NONE',  ( 8.000000000000007105, -9.604183132802424083, 5.908880290975512928 ) ) ;
#3170 = EDGE_CURVE ( 'NONE', #26059, #1241, #21974, .T. ) ;
#3171 = CARTESIAN_POINT ( 'NONE',  ( -35.50000000000000711, -115.3362660311619692, -1.573728109101206085 ) ) ;
#3172 = CARTESIAN_POINT ( 'NONE',  ( 8.000000000000007105, 13.61301047812928111, 3.268936481846215880 ) ) ;
#3173 = AXIS2_PLACEMENT_3D ( 'NONE', #26345, #13198, #35339 ) ;
#3174 = CARTESIAN_POINT ( 'NONE',  ( -35.50000000000000711, -114.1302255537607095, 9.515717283514957714 ) ) ;
#3175 = CYLINDRICAL_SURFACE ( 'NONE', #25301, 0.6000000000000029754 ) ;
#3176 = EDGE_CURVE ( 'NONE', #5736, #19206, #13010, .T. ) ;
#3177 = DIRECTION ( 'NONE',  ( 0.000000000000000000, 0.000000000000000000, 1.000000000000000000 ) ) ;
#3178 = EDGE_CURVE ( 'NONE', #11728, #31611, #15857, .T. ) ;
#3179 = CARTESIAN_POINT ( 'NONE',  ( -34.50000000000000000, -114.1861579685891712, 9.524983039397698192 ) ) ;
#3180 = DIRECTION ( 'NONE',  ( 1.000000000000000000, 0.000000000000000000, 0.000000000000000000 ) ) ;
#3181 = AXIS2_PLACEMENT_3D ( 'NONE', #2884, #32755, #11149 ) ;
#3182 = VECTOR ( 'NONE', #30896, 1000.000000000000000 ) ;
#3183 = DIRECTION ( 'NONE',  ( -0.000000000000000000, 0.000000000000000000, -1.000000000000000000 ) ) ;
#3184 = CARTESIAN_POINT ( 'NONE',  ( -35.80421860361284558, -115.9929510916434481, 14.10650203519841916 ) ) ;
#3185 = CARTESIAN_POINT ( 'NONE',  ( -35.50000000000000711, -112.0140978167138712, -0.5622823525984296245 ) ) ;
#3186 = CIRCLE ( 'NONE', #10057, 0.5000000000000004441 ) ;
#3187 = CARTESIAN_POINT ( 'NONE',  ( -34.49999999999998579, -25.98076211353322051, 84.99999999999992895 ) ) ;
#3188 = CARTESIAN_POINT ( 'NONE',  ( -44.00000000000000000, 3.999999999999998224, 4.898587196589410857E-16 ) ) ;
#3189 = CARTESIAN_POINT ( 'NONE',  ( 5.639656061357297467, -10.48075544252193048, -1.200000000000006617 ) ) ;
#3190 = AXIS2_PLACEMENT_3D ( 'NONE', #35359, #29783, #26911 ) ;
#3191 = DIRECTION ( 'NONE',  ( 0.000000000000000000, 0.000000000000000000, -1.000000000000000000 ) ) ;
#3192 = VERTEX_POINT ( 'NONE', #2035 ) ;
#3193 = CARTESIAN_POINT ( 'NONE',  ( -35.62769128460905677, -112.5438815906447729, 9.808975545821551734 ) ) ;
#3194 = DIRECTION ( 'NONE',  ( -1.000000000000000000, 0.000000000000000000, 0.000000000000000000 ) ) ;
#3195 = DIRECTION ( 'NONE',  ( 0.000000000000000000, -6.987080667128811962E-15, 1.000000000000000000 ) ) ;
#3196 = PLANE ( 'NONE',  #422 ) ;
#3197 = ORIENTED_EDGE ( 'NONE', *, *, #14695, .T. ) ;
#3198 = VECTOR ( 'NONE', #1993, 999.9999999999998863 ) ;
#3199 = ORIENTED_EDGE ( 'NONE', *, *, #28205, .T. ) ;
#3200 = APPLICATION_CONTEXT ( 'automotive_design' ) ;
#3201 = DIRECTION ( 'NONE',  ( -1.000000000000000000, -0.000000000000000000, -0.000000000000000000 ) ) ;
#3202 = FACE_OUTER_BOUND ( 'NONE', #11847, .T. ) ;
#3203 = VERTEX_POINT ( 'NONE', #10117 ) ;
#3204 = ORIENTED_EDGE ( 'NONE', *, *, #13737, .T. ) ;
#3205 = ADVANCED_FACE ( 'NONE', ( #21269 ), #5436, .T. ) ;
#3206 = ADVANCED_FACE ( 'NONE', ( #10659 ), #18926, .T. ) ;
#3207 = DIRECTION ( 'NONE',  ( -1.000000000000000000, 0.000000000000000000, 0.000000000000000000 ) ) ;
#3208 = AXIS2_PLACEMENT_3D ( 'NONE', #85, #33034, #11072 ) ;
#3209 = DIRECTION ( 'NONE',  ( -1.000000000000000000, 0.000000000000000000, 0.000000000000000000 ) ) ;
#3210 = CARTESIAN_POINT ( 'NONE',  ( -42.49999999999999289, -25.98076211353321696, 84.99999999999995737 ) ) ;
#3211 = AXIS2_PLACEMENT_3D ( 'NONE', #31257, #6579, #17553 ) ;
#3212 = FACE_OUTER_BOUND ( 'NONE', #3730, .T. ) ;
#3213 = ORIENTED_EDGE ( 'NONE', *, *, #18521, .F. ) ;
#3214 = ORIENTED_EDGE ( 'NONE', *, *, #10364, .T. ) ;
#3215 = AXIS2_PLACEMENT_3D ( 'NONE', #31002, #5818, #33526 ) ;
#3216 = LINE ( 'NONE', #6601, #21447 ) ;
#3217 = CARTESIAN_POINT ( 'NONE',  ( 7.999999999999992895, 44.75336757549778355, 14.30704879393622520 ) ) ;
#3218 = ORIENTED_EDGE ( 'NONE', *, *, #22731, .T. ) ;
#3219 = CARTESIAN_POINT ( 'NONE',  ( 0.000000000000000000, -2.710505431213761085E-17, -54.99999999999999289 ) ) ;
#3220 = AXIS2_PLACEMENT_3D ( 'NONE', #10228, #29315, #21192 ) ;
#3221 = DIRECTION ( 'NONE',  ( 1.000000000000000000, -4.607758420995284547E-15, -1.196244974681468202E-15 ) ) ;
#3222 = CARTESIAN_POINT ( 'NONE',  ( 65.00000000000001421, -30.47068043442695284, 88.33026027086506815 ) ) ;
#3223 = CARTESIAN_POINT ( 'NONE',  ( -34.50000000000000000, -115.9927366631908825, 10.47601115720670073 ) ) ;
#3224 = DIRECTION ( 'NONE',  ( 0.000000000000000000, 0.000000000000000000, 1.000000000000000000 ) ) ;
#3225 = DIRECTION ( 'NONE',  ( 0.000000000000000000, 0.000000000000000000, 1.000000000000000000 ) ) ;
#3226 = CARTESIAN_POINT ( 'NONE',  ( -37.18750000000006395, -114.9929510916434339, 14.11852480586264846 ) ) ;
#3227 = LINE ( 'NONE', #14012, #19913 ) ;
#3228 = DIRECTION ( 'NONE',  ( -1.000000000000000000, -0.000000000000000000, -0.000000000000000000 ) ) ;
#3229 = CARTESIAN_POINT ( 'NONE',  ( 65.00000000000001421, -32.20716221109618260, 78.48218274074299927 ) ) ;
#3230 = DIRECTION ( 'NONE',  ( 1.174092375852890260E-15, -4.222049128630259891E-16, -1.000000000000000000 ) ) ;
#3231 = CARTESIAN_POINT ( 'NONE',  ( 0.000000000000000000, 0.000000000000000000, 0.000000000000000000 ) ) ;
#3232 = AXIS2_PLACEMENT_3D ( 'NONE', #781, #25461, #19843 ) ;
#3233 = ORIENTED_EDGE ( 'NONE', *, *, #18323, .T. ) ;
#3234 = DIRECTION ( 'NONE',  ( -1.000000000000000000, 0.000000000000000000, 0.000000000000000000 ) ) ;
#3235 = ORIENTED_EDGE ( 'NONE', *, *, #28132, .T. ) ;
#3236 = CARTESIAN_POINT ( 'NONE',  ( -40.02454729103296671, -115.1833782841879525, 5.159774454178449155 ) ) ;
#3237 = CARTESIAN_POINT ( 'NONE',  ( 0.000000000000000000, 0.000000000000000000, 0.000000000000000000 ) ) ;
#3238 = VECTOR ( 'NONE', #21287, 1000.000000000000000 ) ;
#3239 = CARTESIAN_POINT ( 'NONE',  ( -35.50000000000000711, -112.6919296022648638, -1.573728109100751116 ) ) ;
#3240 = ORIENTED_EDGE ( 'NONE', *, *, #31686, .T. ) ;
#3241 = ORIENTED_EDGE ( 'NONE', *, *, #35015, .T. ) ;
#3242 = AXIS2_PLACEMENT_3D ( 'NONE', #11628, #16673, #22601 ) ;
#3243 = FACE_OUTER_BOUND ( 'NONE', #27570, .T. ) ;
#3244 = DIRECTION ( 'NONE',  ( -1.000000000000000000, -0.000000000000000000, -0.000000000000000000 ) ) ;
#3245 = ORIENTED_EDGE ( 'NONE', *, *, #28445, .T. ) ;
#3246 = CIRCLE ( 'NONE', #9587, 7.199999999999994849 ) ;
#3247 =( REPRESENTATION_RELATIONSHIP ('NONE','NONE', #26607, #31430 ) REPRESENTATION_RELATIONSHIP_WITH_TRANSFORMATION ( #784 )SHAPE_REPRESENTATION_RELATIONSHIP( ) );
#3248 = DIRECTION ( 'NONE',  ( -1.000000000000000000, 0.000000000000000000, 0.000000000000000000 ) ) ;
#3249 = ADVANCED_FACE ( 'NONE', ( #2225 ), #13537, .T. ) ;
#3250 = FACE_OUTER_BOUND ( 'NONE', #5593, .T. ) ;
#3251 = ORIENTED_EDGE ( 'NONE', *, *, #9751, .T. ) ;
#3252 = ORIENTED_EDGE ( 'NONE', *, *, #32189, .T. ) ;
#3253 = DIRECTION ( 'NONE',  ( 0.000000000000000000, 0.000000000000000000, 1.000000000000000000 ) ) ;
#3254 = PLANE ( 'NONE',  #8668 ) ;
#3255 = CIRCLE ( 'NONE', #25691, 20.00000000000001066 ) ;
#3256 = ORIENTED_EDGE ( 'NONE', *, *, #18348, .F. ) ;
#3257 = ORIENTED_EDGE ( 'NONE', *, *, #26825, .F. ) ;
#3258 = CARTESIAN_POINT ( 'NONE',  ( -34.50000000000000000, -116.9119893297194324, -1.269118781492768688 ) ) ;
#3259 = CIRCLE ( 'NONE', #359, 4.800000000000000711 ) ;
#3260 = EDGE_CURVE ( 'NONE', #32804, #20080, #14481, .T. ) ;
#3261 = ORIENTED_EDGE ( 'NONE', *, *, #16911, .T. ) ;
#3262 = CARTESIAN_POINT ( 'NONE',  ( -35.91854304697313438, -114.9929510916434339, 13.11211614918345703 ) ) ;
#3263 = CIRCLE ( 'NONE', #7842, 4.000000000000000000 ) ;
#3264 = CIRCLE ( 'NONE', #15311, 17.49900000000001654 ) ;
#3265 = CIRCLE ( 'NONE', #17034, 22.00000000000000000 ) ;
#3266 = CARTESIAN_POINT ( 'NONE',  ( -34.50000000000000000, -113.9929510916434339, 12.57451923796416260 ) ) ;
#3267 = AXIS2_PLACEMENT_3D ( 'NONE', #20064, #28369, #6398 ) ;
#3268 = DIRECTION ( 'NONE',  ( -0.000000000000000000, 0.000000000000000000, -1.000000000000000000 ) ) ;
#3269 = DIRECTION ( 'NONE',  ( 0.000000000000000000, 0.2538061376417697357, 0.9672551082808334977 ) ) ;
#3270 = CARTESIAN_POINT ( 'NONE',  ( -34.50000000000000000, -113.9929510916434339, 12.44250253426871033 ) ) ;
#3271 = DIRECTION ( 'NONE',  ( -1.000000000000000000, 0.000000000000000000, 0.000000000000000000 ) ) ;
#3272 =( GEOMETRIC_REPRESENTATION_CONTEXT ( 3 ) GLOBAL_UNCERTAINTY_ASSIGNED_CONTEXT ( ( #25453 ) ) GLOBAL_UNIT_ASSIGNED_CONTEXT ( ( #11202, #2780, #8505 ) ) REPRESENTATION_CONTEXT ( 'NONE', 'WORKASPACE' ) );
#3273 = CARTESIAN_POINT ( 'NONE',  ( -35.50000000000000711, -114.9925223117477202, 10.47601618151863079 ) ) ;
#3274 = DIRECTION ( 'NONE',  ( -1.000000000000000000, 0.000000000000000000, 0.000000000000000000 ) ) ;
#3275 = LINE ( 'NONE', #555, #6619 ) ;
#3276 = ORIENTED_EDGE ( 'NONE', *, *, #9282, .T. ) ;
#3277 = ORIENTED_EDGE ( 'NONE', *, *, #8445, .T. ) ;
#3278 = DIRECTION ( 'NONE',  ( 0.000000000000000000, 0.000000000000000000, 1.000000000000000000 ) ) ;
#3279 = CARTESIAN_POINT ( 'NONE',  ( -10.00000000000000178, 0.000000000000000000, 0.000000000000000000 ) ) ;
#3280 = CIRCLE ( 'NONE', #23387, 47.49900000000001654 ) ;
#3281 = VECTOR ( 'NONE', #13675, 1000.000000000000000 ) ;
#3282 = VERTEX_POINT ( 'NONE', #30098 ) ;
#3283 = CYLINDRICAL_SURFACE ( 'NONE', #10160, 7.199999999999994849 ) ;
#3284 = ORIENTED_EDGE ( 'NONE', *, *, #22447, .T. ) ;
#3285 = VECTOR ( 'NONE', #13983, 1000.000000000000000 ) ;
#3286 = CARTESIAN_POINT ( 'NONE',  ( -35.50000000000000000, -113.0974311500471714, -0.6247823525984269599 ) ) ;
#3287 = CARTESIAN_POINT ( 'NONE',  ( 8.000000000000000000, -12.49559743815785140, 9.169462670380546854 ) ) ;
#3288 = CARTESIAN_POINT ( 'NONE',  ( -35.02454729103298803, -114.8876895276775087, 1.597274454178448710 ) ) ;
#3289 = VERTEX_POINT ( 'NONE', #18576 ) ;
#3290 = LINE ( 'NONE', #22523, #14750 ) ;
#3291 = ORIENTED_EDGE ( 'NONE', *, *, #27599, .F. ) ;
#3292 = AXIS2_PLACEMENT_3D ( 'NONE', #1875, #35005, #18769 ) ;
#3293 = DIRECTION ( 'NONE',  ( -1.000000000000000000, 0.000000000000000000, 0.000000000000000000 ) ) ;
#3294 = EDGE_CURVE ( 'NONE', #20209, #3876, #9339, .T. ) ;
#3295 = CARTESIAN_POINT ( 'NONE',  ( -35.50000000000000000, -117.0140978167138854, 0.8752176474015623819 ) ) ;
#3296 = ORIENTED_EDGE ( 'NONE', *, *, #12144, .T. ) ;
#3297 = ORIENTED_EDGE ( 'NONE', *, *, #17207, .T. ) ;
#3298 = EDGE_CURVE ( 'NONE', #33119, #14640, #18746, .T. ) ;
#3299 = AXIS2_PLACEMENT_3D ( 'NONE', #28734, #34852, #23679 ) ;
#3300 = VECTOR ( 'NONE', #8931, 1000.000000000000000 ) ;
#3301 = CARTESIAN_POINT ( 'NONE',  ( -38.45611840935523418, -115.3723087153909432, 6.566024454178448266 ) ) ;
#3302 =( LENGTH_UNIT ( ) NAMED_UNIT ( * ) SI_UNIT ( .MILLI., .METRE. ) );
#3303 = DIRECTION ( 'NONE',  ( -1.000000000000000000, 0.000000000000000000, 0.000000000000000000 ) ) ;
#3304 = ORIENTED_EDGE ( 'NONE', *, *, #18350, .F. ) ;
#3305 = ORIENTED_EDGE ( 'NONE', *, *, #19236, .T. ) ;
#3306 = CARTESIAN_POINT ( 'NONE',  ( -34.50000000000000000, -113.1256619669233885, 1.895633585076891947 ) ) ;
#3307 = CARTESIAN_POINT ( 'NONE',  ( 0.000000000000000000, 0.000000000000000000, 0.000000000000000000 ) ) ;
#3308 = EDGE_CURVE ( 'NONE', #13350, #4520, #28897, .T. ) ;
#3309 = VERTEX_POINT ( 'NONE', #13194 ) ;
#3310 = LINE ( 'NONE', #8861, #35043 ) ;
#3311 = AXIS2_PLACEMENT_3D ( 'NONE', #78, #11065, #22035 ) ;
#3312 = VECTOR ( 'NONE', #3271, 1000.000000000000000 ) ;
#3313 = CARTESIAN_POINT ( 'NONE',  ( -35.50000000000000000, -113.9929510916436470, 10.50625754673586876 ) ) ;
#3314 = CARTESIAN_POINT ( 'NONE',  ( 0.000000000000000000, 5.679790370316226245, -7.613867765417517752 ) ) ;
#3315 = CARTESIAN_POINT ( 'NONE',  ( 3.872983346207429900, -1.000000000000003553, 55.00000000000000000 ) ) ;
#3316 = CARTESIAN_POINT ( 'NONE',  ( -34.50000000000000000, -116.0141056290913610, -0.5935324770972248976 ) ) ;
#3317 = AXIS2_PLACEMENT_3D ( 'NONE', #10394, #21351, #21710 ) ;
#3318 = CIRCLE ( 'NONE', #23430, 4.000000000000000000 ) ;
#3319 = CARTESIAN_POINT ( 'NONE',  ( -35.50000000000000000, -114.3793648455349654, 8.543708532059524074 ) ) ;
#3320 = DIRECTION ( 'NONE',  ( -1.000000000000000000, 0.000000000000000000, 0.000000000000000000 ) ) ;
#3321 = CIRCLE ( 'NONE', #29206, 20.00000000000000711 ) ;
#3322 = DIRECTION ( 'NONE',  ( -1.000000000000000000, 0.000000000000000000, 0.000000000000000000 ) ) ;
#3323 = AXIS2_PLACEMENT_3D ( 'NONE', #8576, #33082, #6238 ) ;
#3324 = ORIENTED_EDGE ( 'NONE', *, *, #1369, .T. ) ;
#3325 = LINE ( 'NONE', #19501, #6756 ) ;
#3326 = CARTESIAN_POINT ( 'NONE',  ( 8.000000000000007105, 11.27190672109280811, 4.484851126495202678 ) ) ;
#3327 = CARTESIAN_POINT ( 'NONE',  ( -0.2000000000000612399, -6.997142273814382030, -0.7999999999999951594 ) ) ;
#3328 = ADVANCED_FACE ( 'NONE', ( #24167 ), #16388, .T. ) ;
#3329 = ORIENTED_EDGE ( 'NONE', *, *, #22946, .F. ) ;
#3330 = DIRECTION ( 'NONE',  ( 0.000000000000000000, 0.000000000000000000, -1.000000000000000000 ) ) ;
#3331 = CARTESIAN_POINT ( 'NONE',  ( 0.000000000000000000, -16.59870953437682672, 3.253005020243791456 ) ) ;
#3332 = CARTESIAN_POINT ( 'NONE',  ( -50.00000000000000000, 19.99999999999998934, 120.0000000000000000 ) ) ;
#3333 = DIRECTION ( 'NONE',  ( 1.174092375852890457E-15, -4.222049128630259891E-16, -1.000000000000000000 ) ) ;
#3334 = CONTEXT_DEPENDENT_SHAPE_REPRESENTATION ( #15622, #20403 ) ;
#3335 = LINE ( 'NONE', #609, #340 ) ;
#3336 = FACE_OUTER_BOUND ( 'NONE', #30465, .T. ) ;
#3337 = CIRCLE ( 'NONE', #13108, 6.984000000000015085 ) ;
#3338 = VERTEX_POINT ( 'NONE', #21799 ) ;
#3339 = CARTESIAN_POINT ( 'NONE',  ( 0.000000000000000000, 0.000000000000000000, 60.90000000000001279 ) ) ;
#3340 = VECTOR ( 'NONE', #4704, 1000.000000000000000 ) ;
#3341 = EDGE_CURVE ( 'NONE', #12939, #35590, #8755, .T. ) ;
#3342 = DIRECTION ( 'NONE',  ( -1.000000000000000000, 0.000000000000000000, 0.000000000000000000 ) ) ;
#3343 = CARTESIAN_POINT ( 'NONE',  ( -42.49999999999999289, -17.72201855431888973, 73.69543654875883476 ) ) ;
#3344 = VERTEX_POINT ( 'NONE', #2756 ) ;
#3345 = ADVANCED_FACE ( 'NONE', ( #34795 ), #7764, .T. ) ;
#3346 = CARTESIAN_POINT ( 'NONE',  ( -37.05926240293131713, -113.0000000000000000, 5.121475545821551734 ) ) ;
#3347 = ADVANCED_FACE ( 'NONE', ( #5093, #24345 ), #18397, .F. ) ;
#3348 = ORIENTED_EDGE ( 'NONE', *, *, #35246, .T. ) ;
#3349 = AXIS2_PLACEMENT_3D ( 'NONE', #22314, #5422, #8627 ) ;
#3350 =( NAMED_UNIT ( * ) SI_UNIT ( $, .STERADIAN. ) SOLID_ANGLE_UNIT ( ) );
#3351 = ORIENTED_EDGE ( 'NONE', *, *, #23483, .T. ) ;
#3352 = ORIENTED_EDGE ( 'NONE', *, *, #26701, .T. ) ;
#3353 = AXIS2_PLACEMENT_3D ( 'NONE', #24854, #11170, #14214 ) ;
#3354 = DIRECTION ( 'NONE',  ( 0.000000000000000000, 0.000000000000000000, 1.000000000000000000 ) ) ;
#3355 = ADVANCED_FACE ( 'NONE', ( #16034 ), #2395, .T. ) ;
#3356 = VECTOR ( 'NONE', #5930, 999.9999999999998863 ) ;
#3357 = CARTESIAN_POINT ( 'NONE',  ( -35.50000000000000711, -116.0060826362711595, -0.7553032835231661135 ) ) ;
#3358 = ADVANCED_FACE ( 'NONE', ( #33663 ), #8480, .F. ) ;
#3359 = DIRECTION ( 'NONE',  ( 0.000000000000000000, 0.000000000000000000, 1.000000000000000000 ) ) ;
#3360 = CARTESIAN_POINT ( 'NONE',  ( -35.50000000000000711, -114.8847986568751907, 10.03799953695244618 ) ) ;
#3361 = CARTESIAN_POINT ( 'NONE',  ( 7.999999999999992895, 44.61570720899074161, 14.73072383765644489 ) ) ;
#3362 = CARTESIAN_POINT ( 'NONE',  ( 0.000000000000000000, 0.000000000000000000, 0.000000000000000000 ) ) ;
#3363 = CARTESIAN_POINT ( 'NONE',  ( -34.50000000000000000, -114.9929510916434339, 11.91443571948719971 ) ) ;
#3364 = LINE ( 'NONE', #22586, #35253 ) ;
#3365 = LINE ( 'NONE', #5525, #12294 ) ;
#3366 = CARTESIAN_POINT ( 'NONE',  ( -35.50000000000000000, -115.9929510916434481, 10.52826033068511435 ) ) ;
#3367 = CARTESIAN_POINT ( 'NONE',  ( -35.50000000000000711, -112.0651520602111191, -0.9469505670458575608 ) ) ;
#3368 = DIRECTION ( 'NONE',  ( 0.000000000000000000, 0.000000000000000000, 1.000000000000000000 ) ) ;
#3369 = ADVANCED_FACE ( 'NONE', ( #3622 ), #27753, .F. ) ;
#3370 = FACE_OUTER_BOUND ( 'NONE', #1796, .T. ) ;
#3371 = CIRCLE ( 'NONE', #5680, 2.799122904894268071 ) ;
#3372 = DIRECTION ( 'NONE',  ( 0.000000000000000000, 0.000000000000000000, 1.000000000000000000 ) ) ;
#3373 = CARTESIAN_POINT ( 'NONE',  ( 1.110223024625156540E-13, -1.000000000000042633, -52.50000000000000000 ) ) ;
#3374 = EDGE_CURVE ( 'NONE', #23819, #19728, #2923, .T. ) ;
#3375 = CARTESIAN_POINT ( 'NONE',  ( -42.49999999999999289, -34.27980021920977549, 73.62564434701768334 ) ) ;
#3376 = DIRECTION ( 'NONE',  ( -1.000000000000000000, -0.000000000000000000, -0.000000000000000000 ) ) ;
#3377 = VERTEX_POINT ( 'NONE', #33151 ) ;
#3378 = EDGE_CURVE ( 'NONE', #17419, #26106, #24867, .T. ) ;
#3379 = CARTESIAN_POINT ( 'NONE',  ( -37.66520193420439711, -114.7490116281687023, 3.058975545821551734 ) ) ;
#3380 =( GEOMETRIC_REPRESENTATION_CONTEXT ( 3 ) GLOBAL_UNCERTAINTY_ASSIGNED_CONTEXT ( ( #13929 ) ) GLOBAL_UNIT_ASSIGNED_CONTEXT ( ( #15783, #35436, #7692 ) ) REPRESENTATION_CONTEXT ( 'NONE', 'WORKASPACE' ) );
#3381 = CARTESIAN_POINT ( 'NONE',  ( 0.000000000000000000, 5.400000000000000355, -0.9999999999999985567 ) ) ;
#3382 = CARTESIAN_POINT ( 'NONE',  ( 4.000000000000000000, 4.627536653468036720E-16, 45.10000000000000142 ) ) ;
#3383 = DIRECTION ( 'NONE',  ( -1.000000000000000000, -1.836970198721029934E-16, -0.000000000000000000 ) ) ;
#3384 = VERTEX_POINT ( 'NONE', #24 ) ;
#3385 = ORIENTED_EDGE ( 'NONE', *, *, #20497, .F. ) ;
#3386 = DIRECTION ( 'NONE',  ( -1.000000000000000000, 0.000000000000000000, 0.000000000000000000 ) ) ;
#3387 = CARTESIAN_POINT ( 'NONE',  ( 8.000000000000000000, 18.62763138773855687, 2.494040418455418351 ) ) ;
#3388 = ORIENTED_EDGE ( 'NONE', *, *, #16220, .T. ) ;
#3389 = EDGE_CURVE ( 'NONE', #2565, #13276, #17096, .T. ) ;
#3390 = ORIENTED_EDGE ( 'NONE', *, *, #9869, .F. ) ;
#3391 = EDGE_CURVE ( 'NONE', #9669, #4180, #13942, .T. ) ;
#3392 = CARTESIAN_POINT ( 'NONE',  ( 0.000000000000000000, 0.000000000000000000, -39.50000000000000711 ) ) ;
#3393 = PLANE ( 'NONE',  #18283 ) ;
#3394 = APPLICATION_PROTOCOL_DEFINITION ( 'draft international standard', 'automotive_design', 1998, #19717 ) ;
#3395 = EDGE_CURVE ( 'NONE', #28380, #3813, #30458, .T. ) ;
#3396 = CARTESIAN_POINT ( 'NONE',  ( 0.000000000000000000, 10.00000000000000888, -25.00000000000000000 ) ) ;
#3397 = EDGE_LOOP ( 'NONE', ( #19722, #11550, #20094, #1381 ) ) ;
#3398 = ORIENTED_EDGE ( 'NONE', *, *, #11251, .T. ) ;
#3399 = CIRCLE ( 'NONE', #17732, 0.5000000000000004441 ) ;
#3400 = CYLINDRICAL_SURFACE ( 'NONE', #16840, 4.000000000000000000 ) ;
#3401 = DIRECTION ( 'NONE',  ( 1.000000000000000000, 1.734723475976807094E-16, -0.000000000000000000 ) ) ;
#3402 = ORIENTED_EDGE ( 'NONE', *, *, #431, .T. ) ;
#3403 = DIRECTION ( 'NONE',  ( 0.02857142857143298714, -0.9995917534020514195, -4.555780455966493806E-16 ) ) ;
#3404 = CARTESIAN_POINT ( 'NONE',  ( -34.50000000000000000, -113.0974311500471714, -0.6247823525984269599 ) ) ;
#3405 = CARTESIAN_POINT ( 'NONE',  ( 0.000000000000000000, 0.000000000000000000, 0.000000000000000000 ) ) ;
#3406 = CARTESIAN_POINT ( 'NONE',  ( 8.000000000000000000, 0.000000000000000000, 0.000000000000000000 ) ) ;
#3407 = CARTESIAN_POINT ( 'NONE',  ( -34.50000000000000000, -115.9710363517788068, 10.20486393345008835 ) ) ;
#3408 = FACE_BOUND ( 'NONE', #9795, .T. ) ;
#3409 = CARTESIAN_POINT ( 'NONE',  ( 7.999999999999992895, 0.000000000000000000, 0.000000000000000000 ) ) ;
#3410 = CARTESIAN_POINT ( 'NONE',  ( -38.95206139890800046, -114.9929510916434339, 13.00730889637963728 ) ) ;
#3411 = DIRECTION ( 'NONE',  ( -1.000000000000000000, 0.000000000000000000, 0.000000000000000000 ) ) ;
#3412 = EDGE_CURVE ( 'NONE', #8708, #21509, #24870, .T. ) ;
#3413 = CARTESIAN_POINT ( 'NONE',  ( 8.000000000000000000, -2.912696353505969338, 21.80633394113446499 ) ) ;
#3414 = DIRECTION ( 'NONE',  ( -1.000000000000000000, 0.000000000000000000, 0.000000000000000000 ) ) ;
#3415 = FACE_OUTER_BOUND ( 'NONE', #21315, .T. ) ;
#3416 = EDGE_CURVE ( 'NONE', #33336, #30332, #7608, .T. ) ;
#3417 = ORIENTED_EDGE ( 'NONE', *, *, #12189, .T. ) ;
#3418 = CARTESIAN_POINT ( 'NONE',  ( 0.000000000000000000, 0.000000000000000000, 0.000000000000000000 ) ) ;
#3419 = ORIENTED_EDGE ( 'NONE', *, *, #22946, .T. ) ;
#3420 = VECTOR ( 'NONE', #8550, 1000.000000000000000 ) ;
#3421 = CARTESIAN_POINT ( 'NONE',  ( -35.81662171581204746, -117.0245472910329738, 4.784774454178448266 ) ) ;
#3422 = CARTESIAN_POINT ( 'NONE',  ( 7.999999999999992895, -19.44205635905572649, 43.33776004284603545 ) ) ;
#3423 = CARTESIAN_POINT ( 'NONE',  ( -35.50000000000000711, -112.0140978167138712, -0.1247823525984259746 ) ) ;
#3424 = VERTEX_POINT ( 'NONE', #3093 ) ;
#3425 = AXIS2_PLACEMENT_3D ( 'NONE', #34075, #25976, #23806 ) ;
#3426 = ORIENTED_EDGE ( 'NONE', *, *, #17908, .F. ) ;
#3427 = DIRECTION ( 'NONE',  ( 0.000000000000000000, 0.5000000000000011102, -0.8660254037844379305 ) ) ;
#3428 = DIRECTION ( 'NONE',  ( 0.000000000000000000, 0.000000000000000000, 1.000000000000000000 ) ) ;
#3429 = EDGE_CURVE ( 'NONE', #21242, #33174, #16803, .T. ) ;
#3430 = ORIENTED_EDGE ( 'NONE', *, *, #23446, .T. ) ;
#3431 = AXIS2_PLACEMENT_3D ( 'NONE', #3458, #30804, #5797 ) ;
#3432 = DIRECTION ( 'NONE',  ( -1.000000000000000000, 0.000000000000000000, 0.000000000000000000 ) ) ;
#3433 = ORIENTED_EDGE ( 'NONE', *, *, #12611, .F. ) ;
#3434 = ORIENTED_EDGE ( 'NONE', *, *, #31199, .T. ) ;
#3435 = FACE_OUTER_BOUND ( 'NONE', #10788, .T. ) ;
#3436 = SHAPE_REPRESENTATION_RELATIONSHIP ( 'NONE' , 'NONE' ,  #2005, #2239 ) ;
#3437 = CARTESIAN_POINT ( 'NONE',  ( 0.000000000000000000, -2.710505431213761085E-17, 55.00000000000000000 ) ) ;
#3438 = EDGE_LOOP ( 'NONE', ( #15500, #5981, #28662, #25374 ) ) ;
#3439 = ORIENTED_EDGE ( 'NONE', *, *, #24763, .F. ) ;
#3440 = CARTESIAN_POINT ( 'NONE',  ( -35.50000000000000000, -111.0140821919084715, 0.8283428459075261596 ) ) ;
#3441 = AXIS2_PLACEMENT_3D ( 'NONE', #32344, #21349, #13444 ) ;
#3442 = DIRECTION ( 'NONE',  ( 0.000000000000000000, -0.9048270524660145808, -0.4257792915650830956 ) ) ;
#3443 = ORIENTED_EDGE ( 'NONE', *, *, #9526, .T. ) ;
#3444 = CARTESIAN_POINT ( 'NONE',  ( -36.07812499999994316, -114.9929510916434339, 13.11852480586264669 ) ) ;
#3445 = CARTESIAN_POINT ( 'NONE',  ( -39.00000000000000000, -113.9929510916434339, 10.50625754673587053 ) ) ;
#3446 = DIRECTION ( 'NONE',  ( 1.000000000000000000, -0.000000000000000000, -0.000000000000000000 ) ) ;
#3447 = DIRECTION ( 'NONE',  ( 1.174092375852890260E-15, -4.222049128630259891E-16, -1.000000000000000000 ) ) ;
#3448 = CARTESIAN_POINT ( 'NONE',  ( -34.50000000000000000, -113.9929510916434339, 10.51725893871049067 ) ) ;
#3450 = DIRECTION ( 'NONE',  ( -1.734723475976807094E-16, -1.000000000000000000, 1.067522139062650474E-15 ) ) ;
#3449 = CIRCLE ( 'NONE', #1719, 0.9999999999999974465 ) ;
#3451 = CARTESIAN_POINT ( 'NONE',  ( -37.51635661748575501, -114.9929510916434339, 13.11827392651459157 ) ) ;
#3452 = DIRECTION ( 'NONE',  ( -0.000000000000000000, 0.000000000000000000, -1.000000000000000000 ) ) ;
#3453 = CARTESIAN_POINT ( 'NONE',  ( 0.000000000000000000, -46.21320724403641833, -10.97699764142004497 ) ) ;
#3454 = CYLINDRICAL_SURFACE ( 'NONE', #10008, 10.49999999999999645 ) ;
#3455 = EDGE_CURVE ( 'NONE', #34251, #34512, #5894, .T. ) ;
#3456 = ORIENTED_EDGE ( 'NONE', *, *, #20900, .T. ) ;
#3457 = ORIENTED_EDGE ( 'NONE', *, *, #27350, .F. ) ;
#3458 = CARTESIAN_POINT ( 'NONE',  ( 0.000000000000000000, 0.000000000000000000, -31.10000000000000142 ) ) ;
#3459 = DIRECTION ( 'NONE',  ( 0.000000000000000000, 0.000000000000000000, 1.000000000000000000 ) ) ;
#3460 = VERTEX_POINT ( 'NONE', #367 ) ;
#3461 = CARTESIAN_POINT ( 'NONE',  ( 0.000000000000000000, -19.77827456857333743, -2.969824084036672751 ) ) ;
#3462 = VERTEX_POINT ( 'NONE', #30278 ) ;
#3463 = CARTESIAN_POINT ( 'NONE',  ( -35.50000000000000000, -113.0140978167143260, -0.6247823525984285142 ) ) ;
#3464 = LINE ( 'NONE', #5804, #27125 ) ;
#3465 = CARTESIAN_POINT ( 'NONE',  ( -34.97545270896703329, -113.2308352781851539, 5.909774454178449155 ) ) ;
#3466 = ORIENTED_EDGE ( 'NONE', *, *, #21355, .F. ) ;
#3467 = CARTESIAN_POINT ( 'NONE',  ( 8.000000000000007105, -9.433698091065020108, -1.111908866155191022 ) ) ;
#3468 = VERTEX_POINT ( 'NONE', #720 ) ;
#3469 = AXIS2_PLACEMENT_3D ( 'NONE', #2651, #24608, #10024 ) ;
#3470 = DIRECTION ( 'NONE',  ( 0.000000000000000000, 1.000000000000000000, 3.614007241618346010E-15 ) ) ;
#3471 = CARTESIAN_POINT ( 'NONE',  ( -35.50000000000000000, -116.9884631899972476, -0.9506101647064282290 ) ) ;
#3472 = ORIENTED_EDGE ( 'NONE', *, *, #8151, .T. ) ;
#3473 = ORIENTED_EDGE ( 'NONE', *, *, #18559, .T. ) ;
#3474 = CARTESIAN_POINT ( 'NONE',  ( -34.97545270896703329, -113.2308352781851539, 5.909774454178449155 ) ) ;
#3475 = CIRCLE ( 'NONE', #18979, 8.000000000000000000 ) ;
#3476 = CIRCLE ( 'NONE', #26479, 19.99999999999998579 ) ;
#3477 = SURFACE_STYLE_USAGE ( .BOTH. , #17127 ) ;
#3478 = CARTESIAN_POINT ( 'NONE',  ( 38.00000000000000000, 14.30000000000001492, 3.000000000000002665 ) ) ;
#3479 = ORIENTED_EDGE ( 'NONE', *, *, #27615, .F. ) ;
#3480 = VERTEX_POINT ( 'NONE', #24696 ) ;
#3481 = CARTESIAN_POINT ( 'NONE',  ( -34.50000000000000000, -112.7765286249690035, 1.847058736912741583 ) ) ;
#3482 = DIRECTION ( 'NONE',  ( -1.226634733346697831E-16, 0.7071067811865466846, 0.7071067811865483499 ) ) ;
#3483 = PRODUCT_DEFINITION_SHAPE ( 'NONE', 'NONE',  #35617 ) ;
#3484 = ORIENTED_EDGE ( 'NONE', *, *, #10018, .F. ) ;
#3485 = ORIENTED_EDGE ( 'NONE', *, *, #23597, .F. ) ;
#3486 = CARTESIAN_POINT ( 'NONE',  ( -34.49999999999998579, -1.338792908815551458E-14, 114.0000000000000000 ) ) ;
#3487 = CARTESIAN_POINT ( 'NONE',  ( -36.12500000000014211, -113.9929510916434339, 13.11852480586264846 ) ) ;
#3488 = DIRECTION ( 'NONE',  ( -1.000000000000000000, 0.000000000000000000, 0.000000000000000000 ) ) ;
#3489 = CARTESIAN_POINT ( 'NONE',  ( 65.00000000000001421, -25.98076211353320986, 80.99999999999992895 ) ) ;
#3490 = CARTESIAN_POINT ( 'NONE',  ( -34.50000000000000000, -116.0140978167138712, -0.5622823525984409487 ) ) ;
#3491 = CARTESIAN_POINT ( 'NONE',  ( -39.00000000000000000, -115.9929510916434481, 10.85830208992306822 ) ) ;
#3492 = CARTESIAN_POINT ( 'NONE',  ( 3.872983346207517386, -1.000000000000028644, -40.00000000000000711 ) ) ;
#3493 = CIRCLE ( 'NONE', #6353, 20.00000000000000355 ) ;
#3494 = DIRECTION ( 'NONE',  ( -0.000000000000000000, 0.000000000000000000, 1.000000000000000000 ) ) ;
#3495 = EDGE_CURVE ( 'NONE', #23884, #3935, #16828, .T. ) ;
#3496 = EDGE_CURVE ( 'NONE', #16062, #16883, #15098, .T. ) ;
#3497 = CIRCLE ( 'NONE', #26476, 20.00000000000000711 ) ;
#3498 = CARTESIAN_POINT ( 'NONE',  ( 0.000000000000000000, 0.000000000000000000, 0.000000000000000000 ) ) ;
#3499 = CARTESIAN_POINT ( 'NONE',  ( 0.000000000000000000, -8.931325931664478190, -16.53603053422218494 ) ) ;
#3500 = CARTESIAN_POINT ( 'NONE',  ( 3.872983346207416133, 1.000000000000001110, -29.99999999999999289 ) ) ;
#3501 = ORIENTED_EDGE ( 'NONE', *, *, #30231, .T. ) ;
#3502 = CARTESIAN_POINT ( 'NONE',  ( 5.400000000000015454, -1.000000000000002220, 30.00000000000000000 ) ) ;
#3503 = DIRECTION ( 'NONE',  ( -1.000000000000000000, 0.000000000000000000, 0.000000000000000000 ) ) ;
#3504 = FACE_BOUND ( 'NONE', #23755, .T. ) ;
#3505 = CARTESIAN_POINT ( 'NONE',  ( 7.999999999999992895, 34.03046037009256963, 33.13733193845818903 ) ) ;
#3506 = ADVANCED_FACE ( 'NONE', ( #19616 ), #25227, .F. ) ;
#3507 = DIRECTION ( 'NONE',  ( -1.000000000000000000, 0.000000000000000000, 0.000000000000000000 ) ) ;
#3508 = FACE_OUTER_BOUND ( 'NONE', #17433, .T. ) ;
#3509 = ORIENTED_EDGE ( 'NONE', *, *, #30780, .F. ) ;
#3510 =( NAMED_UNIT ( * ) PLANE_ANGLE_UNIT ( ) SI_UNIT ( $, .RADIAN. ) );
#3511 = DIRECTION ( 'NONE',  ( 0.000000000000000000, 0.000000000000000000, 1.000000000000000000 ) ) ;
#3512 = DIRECTION ( 'NONE',  ( 0.000000000000000000, 0.6427876096865349220, 0.7660444431189816772 ) ) ;
#3513 = EDGE_LOOP ( 'NONE', ( #35507, #10361 ) ) ;
#3514 = VECTOR ( 'NONE', #32219, 1000.000000000000000 ) ;
#3515 = CARTESIAN_POINT ( 'NONE',  ( -36.33479806579560289, -113.2509883718313262, 6.808975545821551734 ) ) ;
#3516 = ORIENTED_EDGE ( 'NONE', *, *, #4525, .F. ) ;
#3517 = ITEM_DEFINED_TRANSFORMATION ( 'NONE', 'NONE', #25935,  #21307 ) ;
#3518 = ORIENTED_EDGE ( 'NONE', *, *, #24631, .F. ) ;
#3519 = ORIENTED_EDGE ( 'NONE', *, *, #10818, .F. ) ;
#3520 = DIRECTION ( 'NONE',  ( 0.000000000000000000, 0.000000000000000000, 1.000000000000000000 ) ) ;
#3521 = AXIS2_PLACEMENT_3D ( 'NONE', #24715, #43, #13207 ) ;
#3522 = PRESENTATION_LAYER_ASSIGNMENT (  '', '', ( #24779 ) ) ;
#3523 = AXIS2_PLACEMENT_3D ( 'NONE', #4514, #4146, #12406 ) ;
#3524 = CARTESIAN_POINT ( 'NONE',  ( -35.50000000000000711, -114.1807644833817648, -1.624782352598427959 ) ) ;
#3525 = EDGE_CURVE ( 'NONE', #26450, #35140, #7631, .T. ) ;
#3526 = DIRECTION ( 'NONE',  ( -1.000000000000000000, 0.000000000000000000, 0.000000000000000000 ) ) ;
#3527 = CARTESIAN_POINT ( 'NONE',  ( -35.50000000000000711, -114.9925223117477202, 10.47601618151863079 ) ) ;
#3528 = FACE_OUTER_BOUND ( 'NONE', #11822, .T. ) ;
#3529 = DIRECTION ( 'NONE',  ( -1.000000000000000000, 0.000000000000000000, 0.000000000000000000 ) ) ;
#3530 = CARTESIAN_POINT ( 'NONE',  ( -34.50000000000000000, -114.9929517792218689, 10.50900788599415314 ) ) ;
#3531 = LINE ( 'NONE', #16833, #27771 ) ;
#3532 = EDGE_CURVE ( 'NONE', #26843, #30129, #196, .T. ) ;
#3533 = EDGE_CURVE ( 'NONE', #4435, #4367, #11536, .T. ) ;
#3534 = DIRECTION ( 'NONE',  ( 0.000000000000000000, 0.000000000000000000, 1.000000000000000000 ) ) ;
#3535 = EDGE_CURVE ( 'NONE', #23109, #26849, #20321, .T. ) ;
#3536 = CARTESIAN_POINT ( 'NONE',  ( -35.50000000000000000, -114.2265172349312508, 8.519938377296172760 ) ) ;
#3537 = FACE_OUTER_BOUND ( 'NONE', #11543, .T. ) ;
#3538 =( LENGTH_UNIT ( ) NAMED_UNIT ( * ) SI_UNIT ( .MILLI., .METRE. ) );
#3539 = LINE ( 'NONE', #20238, #2128 ) ;
#3540 = CARTESIAN_POINT ( 'NONE',  ( 8.000000000000000000, 14.80634052301623171, 8.177498406287277533 ) ) ;
#3541 = DIRECTION ( 'NONE',  ( 0.000000000000000000, 0.000000000000000000, 1.000000000000000000 ) ) ;
#3542 = LINE ( 'NONE', #14490, #19352 ) ;
#3543 = DIRECTION ( 'NONE',  ( 0.000000000000000000, 0.000000000000000000, -1.000000000000000000 ) ) ;
#3544 = ORIENTED_EDGE ( 'NONE', *, *, #26796, .T. ) ;
#3545 = EDGE_CURVE ( 'NONE', #29395, #5751, #22003, .T. ) ;
#3546 = AXIS2_PLACEMENT_3D ( 'NONE', #17473, #14776, #14245 ) ;
#3547 = CARTESIAN_POINT ( 'NONE',  ( -35.99999999999999289, -114.0592624029313242, 1.503524454178448710 ) ) ;
#3548 = CARTESIAN_POINT ( 'NONE',  ( 7.999999999999992895, -46.21320724403657465, 10.97699764141937884 ) ) ;
#3549 = CARTESIAN_POINT ( 'NONE',  ( 5.400000000000085620, -1.000000000000049516, -32.00000000000000000 ) ) ;
#3550 = EDGE_CURVE ( 'NONE', #1924, #18506, #17453, .T. ) ;
#3551 = ORIENTED_EDGE ( 'NONE', *, *, #3545, .T. ) ;
#3552 = EDGE_LOOP ( 'NONE', ( #35355, #12838, #3978, #32315 ) ) ;
#3553 = DIRECTION ( 'NONE',  ( -1.000000000000000000, 0.000000000000000000, 0.000000000000000000 ) ) ;
#3554 = DIRECTION ( 'NONE',  ( 0.000000000000000000, 0.000000000000000000, 1.000000000000000000 ) ) ;
#3555 = VERTEX_POINT ( 'NONE', #12061 ) ;
#3556 = CARTESIAN_POINT ( 'NONE',  ( -34.02454729103298092, -115.3019030900506294, 7.597274454178449155 ) ) ;
#3557 = ORIENTED_EDGE ( 'NONE', *, *, #19002, .F. ) ;
#3558 = CARTESIAN_POINT ( 'NONE',  ( -3.799999999999999822, 4.653657836759942730E-16, -40.89999999999999858 ) ) ;
#3559 = DIRECTION ( 'NONE',  ( 1.000000000000000000, 1.734723475976807094E-16, 0.000000000000000000 ) ) ;
#3560 = APPLICATION_PROTOCOL_DEFINITION ( 'draft international standard', 'automotive_design', 1998, #5043 ) ;
#3561 = EDGE_CURVE ( 'NONE', #11684, #32704, #13965, .T. ) ;
#3562 = CARTESIAN_POINT ( 'NONE',  ( -1.000000000000014655, -4.808326913196006913, -0.7999999999999951594 ) ) ;
#3563 = ORIENTED_EDGE ( 'NONE', *, *, #18312, .F. ) ;
#3564 = ORIENTED_EDGE ( 'NONE', *, *, #19723, .F. ) ;
#3565 = PRODUCT_RELATED_PRODUCT_CATEGORY ( 'part', '', ( #20719 ) ) ;
#3566 = CARTESIAN_POINT ( 'NONE',  ( 3.799999999999999822, -2.710505431213761085E-17, -30.00000000000000711 ) ) ;
#3567 = AXIS2_PLACEMENT_3D ( 'NONE', #4199, #29393, #4737 ) ;
#3568 = ORIENTED_EDGE ( 'NONE', *, *, #27997, .T. ) ;
#3569 = AXIS2_PLACEMENT_3D ( 'NONE', #16328, #24815, #2869 ) ;
#3570 = CARTESIAN_POINT ( 'NONE',  ( 0.000000000000000000, 0.000000000000000000, 0.000000000000000000 ) ) ;
#3571 = CARTESIAN_POINT ( 'NONE',  ( -34.50000000000000000, -114.8474311500471572, -0.6247823525984269599 ) ) ;
#3572 = LINE ( 'NONE', #19915, #20758 ) ;
#3573 = DIRECTION ( 'NONE',  ( 1.000000000000000000, -5.339440136655842133E-16, -1.047965281155519420E-16 ) ) ;
#3574 = CARTESIAN_POINT ( 'NONE',  ( -34.50000000000000000, -115.9056129652226872, 9.909279992139808257 ) ) ;
#3575 = EDGE_CURVE ( 'NONE', #26508, #27200, #28452, .T. ) ;
#3576 = CYLINDRICAL_SURFACE ( 'NONE', #24372, 52.00000000000000711 ) ;
#3577 = CARTESIAN_POINT ( 'NONE',  ( 0.000000000000000000, 19.74581912682909390, -48.10512059033372623 ) ) ;
#3578 = EDGE_CURVE ( 'NONE', #22879, #18391, #1320, .T. ) ;
#3579 = CARTESIAN_POINT ( 'NONE',  ( -37.46874999999996447, -114.9929510916434339, 14.11852480586264846 ) ) ;
#3580 = DIRECTION ( 'NONE',  ( 0.000000000000000000, 0.000000000000000000, -1.000000000000000000 ) ) ;
#3581 = CARTESIAN_POINT ( 'NONE',  ( 0.000000000000000000, 2.123073309835184830, 47.45152853935336168 ) ) ;
#3582 = STYLED_ITEM ( 'NONE', ( #813 ), #22482 ) ;
#3583 = DIRECTION ( 'NONE',  ( 0.000000000000000000, 0.000000000000000000, 1.000000000000000000 ) ) ;
#3584 = DIRECTION ( 'NONE',  ( 0.000000000000000000, 1.000000000000000000, 0.000000000000000000 ) ) ;
#3585 = ORIENTED_EDGE ( 'NONE', *, *, #10165, .F. ) ;
#3586 = CARTESIAN_POINT ( 'NONE',  ( 0.000000000000000000, 6.359167119270718871, -18.96209359615085788 ) ) ;
#3587 = ORIENTED_EDGE ( 'NONE', *, *, #34796, .F. ) ;
#3588 = AXIS2_PLACEMENT_3D ( 'NONE', #7853, #3008, #24428 ) ;
#3589 = CARTESIAN_POINT ( 'NONE',  ( -38.18337828418796676, -117.0245472910329738, 7.465225545821552622 ) ) ;
#3590 = DIRECTION ( 'NONE',  ( 1.000000000000000000, 0.000000000000000000, 0.000000000000000000 ) ) ;
#3591 = CARTESIAN_POINT ( 'NONE',  ( -35.50000000000000711, -115.2732872103912030, -1.592823285204062911 ) ) ;
#3592 = EDGE_CURVE ( 'NONE', #6257, #21944, #34213, .T. ) ;
#3593 = ORIENTED_EDGE ( 'NONE', *, *, #21723, .T. ) ;
#3594 = ORIENTED_EDGE ( 'NONE', *, *, #28049, .F. ) ;
#3595 = DIRECTION ( 'NONE',  ( 1.000000000000000000, -0.000000000000000000, -0.000000000000000000 ) ) ;
#3596 = CIRCLE ( 'NONE', #11073, 47.49900000000001654 ) ;
#3597 = CARTESIAN_POINT ( 'NONE',  ( -34.49999999999998579, -26.68172400785662290, 89.21410161513767889 ) ) ;
#3598 = EDGE_LOOP ( 'NONE', ( #31397, #23988, #13480, #29011 ) ) ;
#3599 = ORIENTED_EDGE ( 'NONE', *, *, #31643, .T. ) ;
#3600 = AXIS2_PLACEMENT_3D ( 'NONE', #10557, #18296, #13274 ) ;
#3601 = CARTESIAN_POINT ( 'NONE',  ( 0.000000000000000000, -45.78515115856034612, -12.64416602183715455 ) ) ;
#3602 = ORIENTED_EDGE ( 'NONE', *, *, #29308, .T. ) ;
#3603 = ORIENTED_EDGE ( 'NONE', *, *, #24762, .T. ) ;
#3604 = CARTESIAN_POINT ( 'NONE',  ( -39.02454729103295961, -113.2308352781851397, 3.340225545821551734 ) ) ;
#3605 = DIRECTION ( 'NONE',  ( 4.739069934226962966E-18, 0.9934137525465440710, -0.1145823557594880665 ) ) ;
#3606 = EDGE_CURVE ( 'NONE', #20267, #34652, #31328, .T. ) ;
#3607 = CARTESIAN_POINT ( 'NONE',  ( 0.000000000000000000, 39.64889472655781333, -33.64468972902464827 ) ) ;
#3608 = ORIENTED_EDGE ( 'NONE', *, *, #35235, .T. ) ;
#3609 = EDGE_LOOP ( 'NONE', ( #6893, #13089, #3660, #8012 ) ) ;
#3610 = COLOUR_RGB ( '', 0.72549020, 0.75294118, 0.79215686) ;
#3611 = CARTESIAN_POINT ( 'NONE',  ( -35.50000000000000000, -116.6134300264884445, -1.853877267570539944 ) ) ;
#3612 = ADVANCED_FACE ( 'NONE', ( #11882 ), #12247, .T. ) ;
#3613 = ADVANCED_FACE ( 'NONE', ( #9361 ), #28986, .T. ) ;
#3614 = CARTESIAN_POINT ( 'NONE',  ( 7.999999999999992895, 43.55304910509406824, 28.41006711800001128 ) ) ;
#3615 = VERTEX_POINT ( 'NONE', #23037 ) ;
#3616 = CARTESIAN_POINT ( 'NONE',  ( -36.06250000000002132, -114.9929510916434339, 13.11852480586264669 ) ) ;
#3617 = CIRCLE ( 'NONE', #33517, 8.000000000000008882 ) ;
#3618 = CARTESIAN_POINT ( 'NONE',  ( -39.00000000000000000, -113.9929510916434339, 12.39849696637031151 ) ) ;
#3619 = AXIS2_PLACEMENT_3D ( 'NONE', #31515, #15279, #17807 ) ;
#3620 = LINE ( 'NONE', #22670, #21125 ) ;
#3621 = EDGE_CURVE ( 'NONE', #4878, #28758, #31678, .T. ) ;
#3622 = FACE_OUTER_BOUND ( 'NONE', #27621, .T. ) ;
#3623 = EDGE_CURVE ( 'NONE', #2106, #1101, #17984, .T. ) ;
#3624 = CARTESIAN_POINT ( 'NONE',  ( -36.15625000000007816, -113.9929510916434339, 14.11852480586265024 ) ) ;
#3625 = CYLINDRICAL_SURFACE ( 'NONE', #30922, 10.50000000000000178 ) ;
#3626 = CARTESIAN_POINT ( 'NONE',  ( -35.50000000000000711, -114.9929510916434339, 12.59102132592610523 ) ) ;
#3627 = ORIENTED_EDGE ( 'NONE', *, *, #21126, .T. ) ;
#3628 = DIRECTION ( 'NONE',  ( -1.000000000000000000, 0.000000000000000000, 0.000000000000000000 ) ) ;
#3629 = DIRECTION ( 'NONE',  ( 1.000000000000000000, 0.000000000000000000, 0.000000000000000000 ) ) ;
#3630 = VERTEX_POINT ( 'NONE', #4334 ) ;
#3631 = CARTESIAN_POINT ( 'NONE',  ( -35.50000102263782509, -114.9929510916434339, 12.62466071271731316 ) ) ;
#3632 = EDGE_LOOP ( 'NONE', ( #32776, #34412, #11398, #18008 ) ) ;
#3633 = DIRECTION ( 'NONE',  ( -1.000000000000000000, 0.000000000000000000, 0.000000000000000000 ) ) ;
#3634 = CARTESIAN_POINT ( 'NONE',  ( 7.999999999999992895, -9.744342220503712682, 46.48873837489796301 ) ) ;
#3635 = ORIENTED_EDGE ( 'NONE', *, *, #26640, .F. ) ;
#3636 = AXIS2_PLACEMENT_3D ( 'NONE', #10128, #21094, #7428 ) ;
#3637 = CARTESIAN_POINT ( 'NONE',  ( -50.00000000000000000, 0.000000000000000000, -5.000000000000011546 ) ) ;
#3638 = ORIENTED_EDGE ( 'NONE', *, *, #5358, .T. ) ;
#3639 = AXIS2_PLACEMENT_3D ( 'NONE', #10281, #27025, #32239 ) ;
#3640 = CARTESIAN_POINT ( 'NONE',  ( -35.50000000000000000, -115.0140978167138712, -0.3122823525984416149 ) ) ;
#3641 = DIRECTION ( 'NONE',  ( -0.000000000000000000, 0.000000000000000000, -1.000000000000000000 ) ) ;
#3642 = CARTESIAN_POINT ( 'NONE',  ( -36.94073759706868287, -112.0000000000000142, 2.628524454178448710 ) ) ;
#3643 = ORIENTED_EDGE ( 'NONE', *, *, #15823, .T. ) ;
#3644 = CARTESIAN_POINT ( 'NONE',  ( -38.99999999999999289, -113.9407375970686900, 3.753524454178449155 ) ) ;
#3645 = DIRECTION ( 'NONE',  ( -1.174092375852890260E-15, 4.222049128630259891E-16, 1.000000000000000000 ) ) ;
#3646 = VECTOR ( 'NONE', #26534, 1000.000000000000000 ) ;
#3647 = CARTESIAN_POINT ( 'NONE',  ( -35.50000000000000000, -114.6807644833805000, -2.624782352598442614 ) ) ;
#3648 = AXIS2_PLACEMENT_3D ( 'NONE', #11320, #16700, #8432 ) ;
#3649 = ORIENTED_EDGE ( 'NONE', *, *, #4897, .F. ) ;
#3650 = ORIENTED_EDGE ( 'NONE', *, *, #29562, .T. ) ;
#3651 = CARTESIAN_POINT ( 'NONE',  ( -3.799999999999999822, 4.382607293638566128E-16, 45.99999999999998579 ) ) ;
#3652 = FILL_AREA_STYLE_COLOUR ( '', #21906 ) ;
#3653 = EDGE_CURVE ( 'NONE', #9489, #6860, #8784, .T. ) ;
#3654 = FACE_OUTER_BOUND ( 'NONE', #2736, .T. ) ;
#3655 = ORIENTED_EDGE ( 'NONE', *, *, #29996, .T. ) ;
#3656 = ORIENTED_EDGE ( 'NONE', *, *, #5080, .T. ) ;
#3657 = CARTESIAN_POINT ( 'NONE',  ( -34.50000000000000000, -112.0140900043366088, -0.5935324770972457697 ) ) ;
#3658 = FACE_OUTER_BOUND ( 'NONE', #14381, .T. ) ;
#3659 = EDGE_CURVE ( 'NONE', #32739, #28967, #8206, .T. ) ;
#3660 = ORIENTED_EDGE ( 'NONE', *, *, #8778, .T. ) ;
#3661 = ORIENTED_EDGE ( 'NONE', *, *, #6649, .T. ) ;
#3662 = CARTESIAN_POINT ( 'NONE',  ( 38.00000000000000000, 6.980486755139912911E-15, 0.000000000000000000 ) ) ;
#3663 = AXIS2_PLACEMENT_3D ( 'NONE', #8420, #144, #20088 ) ;
#3664 = CARTESIAN_POINT ( 'NONE',  ( -37.46874999999995737, -113.9929510916434339, 13.11852480586264846 ) ) ;
#3665 = FACE_OUTER_BOUND ( 'NONE', #25437, .T. ) ;
#3666 = CARTESIAN_POINT ( 'NONE',  ( 0.000000000000000000, 39.55064067543098361, -25.36340625197317067 ) ) ;
#3667 = CARTESIAN_POINT ( 'NONE',  ( -35.99181955245763476, -113.9929510916434339, 13.11847460610632510 ) ) ;
#3668 = CARTESIAN_POINT ( 'NONE',  ( -35.50000000000000000, -115.9929510916434481, 10.61627146648203990 ) ) ;
#3669 = CARTESIAN_POINT ( 'NONE',  ( 0.000000000000000000, 0.000000000000000000, -53.39999999999999858 ) ) ;
#3670 = APPLICATION_CONTEXT ( 'automotive_design' ) ;
#3672 = AXIS2_PLACEMENT_3D ( 'NONE', #8094, #27206, #7922 ) ;
#3671 = DIRECTION ( 'NONE',  ( 0.000000000000000000, 0.000000000000000000, 1.000000000000000000 ) ) ;
#3673 = CIRCLE ( 'NONE', #19720, 20.00000000000000355 ) ;
#3674 = DIRECTION ( 'NONE',  ( 0.000000000000000000, 0.000000000000000000, -1.000000000000000000 ) ) ;
#3675 = DIRECTION ( 'NONE',  ( -1.000000000000000000, -1.836970198721029934E-16, -0.000000000000000000 ) ) ;
#3676 = CARTESIAN_POINT ( 'NONE',  ( 3.799999999999999822, 0.000000000000000000, -53.39999999999999858 ) ) ;
#3677 = VERTEX_POINT ( 'NONE', #9890 ) ;
#3678 = CARTESIAN_POINT ( 'NONE',  ( 4.000000000000003553, -5.871425383721907920, 51.66745943012281117 ) ) ;
#3679 = DIRECTION ( 'NONE',  ( 0.000000000000000000, -8.881784197001252323E-16, -1.000000000000000000 ) ) ;
#3680 = DIRECTION ( 'NONE',  ( -1.734723475976807094E-16, 1.000000000000000000, 0.000000000000000000 ) ) ;
#3681 = DIRECTION ( 'NONE',  ( -1.000000000000000000, 0.000000000000000000, 0.000000000000000000 ) ) ;
#3682 = CARTESIAN_POINT ( 'NONE',  ( 0.000000000000000000, 0.000000000000000000, 60.00000000000000000 ) ) ;
#3683 = CARTESIAN_POINT ( 'NONE',  ( 70.00000000000001421, 0.000000000000000000, 0.000000000000000000 ) ) ;
#3684 = CIRCLE ( 'NONE', #16864, 0.5000000000000004441 ) ;
#3685 = VERTEX_POINT ( 'NONE', #28810 ) ;
#3686 = DIRECTION ( 'NONE',  ( -1.000000000000000000, 0.000000000000000000, 0.000000000000000000 ) ) ;
#3687 = DIRECTION ( 'NONE',  ( 0.000000000000000000, 0.000000000000000000, -1.000000000000000000 ) ) ;
#3688 = DIRECTION ( 'NONE',  ( -1.000000000000000000, -0.000000000000000000, 0.000000000000000000 ) ) ;
#3689 = ORIENTED_EDGE ( 'NONE', *, *, #33057, .F. ) ;
#3690 = ORIENTED_EDGE ( 'NONE', *, *, #4198, .T. ) ;
#3691 = CARTESIAN_POINT ( 'NONE',  ( -37.99999999999998579, -114.0592624029313242, 7.746475545821553510 ) ) ;
#3692 = ORIENTED_EDGE ( 'NONE', *, *, #7492, .T. ) ;
#3693 = ORIENTED_EDGE ( 'NONE', *, *, #31526, .F. ) ;
#3694 = VERTEX_POINT ( 'NONE', #26294 ) ;
#3695 = DIRECTION ( 'NONE',  ( 1.000000000000000000, 0.000000000000000000, -0.000000000000000000 ) ) ;
#3696 = CIRCLE ( 'NONE', #29001, 20.00000000000000711 ) ;
#3697 = EDGE_CURVE ( 'NONE', #4637, #10821, #30092, .T. ) ;
#3698 = VECTOR ( 'NONE', #15369, 1000.000000000000000 ) ;
#3699 = CARTESIAN_POINT ( 'NONE',  ( 50.00005079999998969, 3.872983346207531596, 1.000000000000000888 ) ) ;
#3700 = FACE_OUTER_BOUND ( 'NONE', #2999, .T. ) ;
#3701 = CARTESIAN_POINT ( 'NONE',  ( -35.50000000000000711, -114.9929510916434339, 10.72628538622835670 ) ) ;
#3702 = CARTESIAN_POINT ( 'NONE',  ( -4.000000000000000000, 0.000000000000000000, -40.40000000000000568 ) ) ;
#3703 = EDGE_CURVE ( 'NONE', #23592, #26583, #31800, .T. ) ;
#3704 = CARTESIAN_POINT ( 'NONE',  ( -50.00000000000000000, 0.000000000000000000, 70.00000000000000000 ) ) ;
#3705 = CARTESIAN_POINT ( 'NONE',  ( -34.50000000000000000, -114.2305202833893816, 9.534416457224700991 ) ) ;
#3706 = DIRECTION ( 'NONE',  ( 0.000000000000000000, 0.000000000000000000, 1.000000000000000000 ) ) ;
#3707 = LINE ( 'NONE', #12156, #33569 ) ;
#3708 = ORIENTED_EDGE ( 'NONE', *, *, #20910, .T. ) ;
#3709 = CARTESIAN_POINT ( 'NONE',  ( -35.50000000000000000, -115.9056129652226872, 9.909279992139808257 ) ) ;
#3710 = CARTESIAN_POINT ( 'NONE',  ( -35.50000000000000711, -112.4434344552011282, 1.705278471174987986 ) ) ;
#3711 = DIRECTION ( 'NONE',  ( -1.000000000000000000, -1.734723475976807094E-16, -0.000000000000000000 ) ) ;
#3712 = DIRECTION ( 'NONE',  ( 0.000000000000000000, -0.8660254037844326014, -0.5000000000000102141 ) ) ;
#3713 = DIRECTION ( 'NONE',  ( 1.000000000000000000, -0.000000000000000000, 0.000000000000000000 ) ) ;
#3714 = DIRECTION ( 'NONE',  ( -1.000000000000000000, -0.000000000000000000, -0.000000000000000000 ) ) ;
#3715 = CIRCLE ( 'NONE', #5469, 0.5000000000000004441 ) ;
#3716 = VECTOR ( 'NONE', #9190, 1000.000000000000000 ) ;
#3717 = DIRECTION ( 'NONE',  ( 0.000000000000000000, 0.000000000000000000, 1.000000000000000000 ) ) ;
#3718 = FACE_OUTER_BOUND ( 'NONE', #10049, .T. ) ;
#3719 = ORIENTED_EDGE ( 'NONE', *, *, #8829, .T. ) ;
#3720 = CARTESIAN_POINT ( 'NONE',  ( -37.05926240293133134, -115.0000000000000000, 1.878524454178448710 ) ) ;
#3721 = CARTESIAN_POINT ( 'NONE',  ( 7.999999999999992895, 32.32520163883582853, 34.09746168776048592 ) ) ;
#3722 = CARTESIAN_POINT ( 'NONE',  ( 4.121423858225409909, -12.61643262889541894, -1.200000000000006617 ) ) ;
#3723 = AXIS2_PLACEMENT_3D ( 'NONE', #20648, #31650, #28079 ) ;
#3724 = ORIENTED_EDGE ( 'NONE', *, *, #24002, .T. ) ;
#3725 = VERTEX_POINT ( 'NONE', #33854 ) ;
#3726 = CARTESIAN_POINT ( 'NONE',  ( 8.000000000000000000, 14.71414642875970635, -9.471478019454975694 ) ) ;
#3727 = CARTESIAN_POINT ( 'NONE',  ( 0.000000000000000000, 5.400000000000029665, -1.000000000000000888 ) ) ;
#3728 = ORIENTED_EDGE ( 'NONE', *, *, #2296, .F. ) ;
#3729 = CARTESIAN_POINT ( 'NONE',  ( -34.00000000000000000, -114.0592624029313242, 9.003524454178446490 ) ) ;
#3730 = EDGE_LOOP ( 'NONE', ( #22010, #30073, #1288, #5060 ) ) ;
#3731 = ADVANCED_FACE ( 'NONE', ( #9180 ), #20144, .T. ) ;
#3732 = FACE_OUTER_BOUND ( 'NONE', #22735, .T. ) ;
#3733 = EDGE_CURVE ( 'NONE', #10764, #30393, #2184, .T. ) ;
#3734 = CARTESIAN_POINT ( 'NONE',  ( -21.15833593587365513, -29.98076211353323828, 83.49999999999990052 ) ) ;
#3735 = APPLICATION_PROTOCOL_DEFINITION ( 'draft international standard', 'automotive_design', 1998, #9172 ) ;
#3736 = CARTESIAN_POINT ( 'NONE',  ( 8.000000000000000000, 18.48663108841359559, 4.615718728112120139 ) ) ;
#3737 = ORIENTED_EDGE ( 'NONE', *, *, #27615, .T. ) ;
#3738 = EDGE_LOOP ( 'NONE', ( #28761, #23199, #32340, #21052 ) ) ;
#3739 = AXIS2_PLACEMENT_3D ( 'NONE', #20237, #31247, #17544 ) ;
#3740 = FACE_OUTER_BOUND ( 'NONE', #13159, .T. ) ;
#3741 = CARTESIAN_POINT ( 'NONE',  ( 8.000000000000000000, -6.336799421339930127, 16.31134495048480915 ) ) ;
#3742 = EDGE_CURVE ( 'NONE', #28748, #5903, #10614, .T. ) ;
#3743 = EDGE_LOOP ( 'NONE', ( #1903, #25067 ) ) ;
#3744 = DIRECTION ( 'NONE',  ( -1.000000000000000000, 0.000000000000000000, 0.000000000000000000 ) ) ;
#3745 = ADVANCED_FACE ( 'NONE', ( #4529 ), #21571, .F. ) ;
#3746 = CIRCLE ( 'NONE', #17524, 5.000000000000004441 ) ;
#3747 = CARTESIAN_POINT ( 'NONE',  ( -34.50000000000000000, -112.9415908020655195, 1.873661708251232572 ) ) ;
#3748 = DIRECTION ( 'NONE',  ( 0.000000000000000000, -0.8090169943749405679, -0.5877852522924826850 ) ) ;
#3749 = DIRECTION ( 'NONE',  ( 0.000000000000000000, 0.000000000000000000, 1.000000000000000000 ) ) ;
#3750 = CIRCLE ( 'NONE', #30774, 4.000000000000000000 ) ;
#3751 = CARTESIAN_POINT ( 'NONE',  ( -34.50000000000000000, -115.9792481177720731, 10.26484292309424795 ) ) ;
#3752 = CARTESIAN_POINT ( 'NONE',  ( 7.999999999999992895, -12.30077720129132679, 50.52416135122078344 ) ) ;
#3753 = CARTESIAN_POINT ( 'NONE',  ( 0.000000000000000000, 0.000000000000000000, -44.50000000000000000 ) ) ;
#3754 = CARTESIAN_POINT ( 'NONE',  ( -39.00000000000000711, -114.9929510916434339, 12.17846912687782179 ) ) ;
#3755 = DIRECTION ( 'NONE',  ( -1.000000000000000000, -1.734723475976807094E-16, -0.000000000000000000 ) ) ;
#3756 = DIRECTION ( 'NONE',  ( 0.000000000000000000, 0.000000000000000000, -1.000000000000000000 ) ) ;
#3757 = AXIS2_PLACEMENT_3D ( 'NONE', #8825, #204, #16919 ) ;
#3758 = CARTESIAN_POINT ( 'NONE',  ( 8.000000000000000000, 0.000000000000000000, 0.000000000000000000 ) ) ;
#3759 = FACE_OUTER_BOUND ( 'NONE', #5965, .T. ) ;
#3760 = ORIENTED_EDGE ( 'NONE', *, *, #24701, .T. ) ;
#3761 = DIRECTION ( 'NONE',  ( -1.000000000000000000, -1.836970198721029934E-16, -0.000000000000000000 ) ) ;
#3762 = ORIENTED_EDGE ( 'NONE', *, *, #12646, .F. ) ;
#3763 = CARTESIAN_POINT ( 'NONE',  ( -39.99999999999999289, -114.0592624029313242, 4.746475545821549957 ) ) ;
#3764 = DIRECTION ( 'NONE',  ( 1.000000000000000000, -0.000000000000000000, 0.000000000000000000 ) ) ;
#3765 = EDGE_CURVE ( 'NONE', #13043, #27252, #27782, .T. ) ;
#3766 = CARTESIAN_POINT ( 'NONE',  ( -35.50000000000000711, -112.0141059978162019, -0.6575071456984691309 ) ) ;
#3767 = ORIENTED_EDGE ( 'NONE', *, *, #3550, .T. ) ;
#3768 = ORIENTED_EDGE ( 'NONE', *, *, #23274, .F. ) ;
#3769 = CLOSED_SHELL ( 'NONE', ( #18687, #5338, #22527, #33299, #32877, #34808, #14774, #29471, #2450, #190, #15138, #32497, #4472, #4930, #4111, #33091, #6476, #7953, #7065, #31290, #10902, #2064, #24425, #21358, #22284, #3966 ) ) ;
#3771 = CARTESIAN_POINT ( 'NONE',  ( 3.872983346207517386, -1.000000000000028644, 65.00000000000000000 ) ) ;
#3770 = PRODUCT_DEFINITION_SHAPE ( 'NONE', 'NONE',  #35625 ) ;
#3772 = CIRCLE ( 'NONE', #11790, 4.000000000000000000 ) ;
#3773 = DIRECTION ( 'NONE',  ( -1.000000000000000000, 0.000000000000000000, 0.000000000000000000 ) ) ;
#3774 = ORIENTED_EDGE ( 'NONE', *, *, #4198, .F. ) ;
#3775 = ORIENTED_EDGE ( 'NONE', *, *, #23135, .F. ) ;
#3776 = VECTOR ( 'NONE', #16093, 1000.000000000000000 ) ;
#3777 = CIRCLE ( 'NONE', #1483, 3.799999999999999822 ) ;
#3778 = EDGE_CURVE ( 'NONE', #10834, #18507, #7072, .T. ) ;
#3779 = DIRECTION ( 'NONE',  ( 0.000000000000000000, 0.000000000000000000, -1.000000000000000000 ) ) ;
#3780 = EDGE_LOOP ( 'NONE', ( #15499, #57, #17915, #25124 ) ) ;
#3781 = EDGE_CURVE ( 'NONE', #32945, #28711, #749, .T. ) ;
#3782 = CARTESIAN_POINT ( 'NONE',  ( -37.05926240293131713, -112.0000000000000142, 5.121475545821551734 ) ) ;
#3783 = EDGE_CURVE ( 'NONE', #15733, #27081, #7382, .T. ) ;
#3784 = DIRECTION ( 'NONE',  ( -1.000000000000000000, -1.502314598737170371E-16, 8.673617379883843187E-17 ) ) ;
#3786 = ORIENTED_EDGE ( 'NONE', *, *, #2897, .T. ) ;
#3785 = AXIS2_PLACEMENT_3D ( 'NONE', #19970, #14762, #31156 ) ;
#3787 = ORIENTED_EDGE ( 'NONE', *, *, #14974, .T. ) ;
#3788 = CARTESIAN_POINT ( 'NONE',  ( -35.50000000000000000, -116.9980674558286040, -0.8858242144478970514 ) ) ;
#3789 = EDGE_CURVE ( 'NONE', #19841, #8832, #24896, .T. ) ;
#3790 = CARTESIAN_POINT ( 'NONE',  ( 3.872983346207517386, -1.000000000000028644, 45.00000000000000711 ) ) ;
#3791 = ORIENTED_EDGE ( 'NONE', *, *, #23520, .F. ) ;
#3792 = CARTESIAN_POINT ( 'NONE',  ( -37.52044295795950291, -114.9929510916434339, 13.11812344617477244 ) ) ;
#3793 = EDGE_CURVE ( 'NONE', #14835, #24556, #25486, .T. ) ;
#3794 = CARTESIAN_POINT ( 'NONE',  ( -37.46093750000000711, -113.9929510916434339, 14.11852480586265024 ) ) ;
#3795 = CIRCLE ( 'NONE', #27367, 11.00000000000000000 ) ;
#3796 = CARTESIAN_POINT ( 'NONE',  ( 112.0000000000000000, 81.48267994499606459, 37.65054357219658243 ) ) ;
#3797 = CARTESIAN_POINT ( 'NONE',  ( -29.99999999999999645, -27.99999999999999289, 113.9999999999999858 ) ) ;
#3798 = CARTESIAN_POINT ( 'NONE',  ( -37.62254989966453422, -113.9929510916434339, 14.11371147303758278 ) ) ;
#3799 = DIRECTION ( 'NONE',  ( -1.000000000000000000, 0.000000000000000000, 0.000000000000000000 ) ) ;
#3800 = AXIS2_PLACEMENT_3D ( 'NONE', #19314, #11409, #11751 ) ;
#3801 = CARTESIAN_POINT ( 'NONE',  ( -35.99386409314529800, -114.9929510916434339, 13.11852378322482515 ) ) ;
#3802 = CARTESIAN_POINT ( 'NONE',  ( 2.321707774797385326, -4.824281976788927118, -0.7999999999999951594 ) ) ;
#3803 = ORIENTED_EDGE ( 'NONE', *, *, #4651, .T. ) ;
#3804 = AXIS2_PLACEMENT_3D ( 'NONE', #1823, #23779, #5412 ) ;
#3805 = FACE_OUTER_BOUND ( 'NONE', #2506, .T. ) ;
#3806 = CARTESIAN_POINT ( 'NONE',  ( -3.983177536951265640, -13.66651769228263724, -1.200000000000006617 ) ) ;
#3807 = ORIENTED_EDGE ( 'NONE', *, *, #14980, .T. ) ;
#3808 = CARTESIAN_POINT ( 'NONE',  ( -35.50000000000000711, -114.9928438774171582, 10.49113435197128652 ) ) ;
#3809 = ORIENTED_EDGE ( 'NONE', *, *, #6680, .F. ) ;
#3810 = DIRECTION ( 'NONE',  ( -1.000000000000000000, -0.000000000000000000, 0.000000000000000000 ) ) ;
#3811 = AXIS2_PLACEMENT_3D ( 'NONE', #13598, #24592, #35584 ) ;
#3812 = EDGE_CURVE ( 'NONE', #3615, #10084, #34695, .T. ) ;
#3813 = VERTEX_POINT ( 'NONE', #29882 ) ;
#3814 = DIRECTION ( 'NONE',  ( -1.000000000000000000, 0.000000000000000000, 0.000000000000000000 ) ) ;
#3815 = ORIENTED_EDGE ( 'NONE', *, *, #827, .F. ) ;
#3816 = CARTESIAN_POINT ( 'NONE',  ( -35.50000000000000000, -113.8474311500459777, -0.6247823525984269599 ) ) ;
#3817 = FACE_OUTER_BOUND ( 'NONE', #18834, .T. ) ;
#3818 = ADVANCED_FACE ( 'NONE', ( #32047 ), #18887, .T. ) ;
#3819 = CARTESIAN_POINT ( 'NONE',  ( -38.37230871539094323, -112.5438815906447729, 5.441024454178449155 ) ) ;
#3820 = VERTEX_POINT ( 'NONE', #18530 ) ;
#3821 = CARTESIAN_POINT ( 'NONE',  ( -36.23083527818512550, -116.0245472910329880, 1.784774454178448932 ) ) ;
#3822 = LINE ( 'NONE', #31353, #1001 ) ;
#3823 = CIRCLE ( 'NONE', #14715, 4.000000000000000000 ) ;
#3824 = CARTESIAN_POINT ( 'NONE',  ( -35.50000000000000711, -113.6807644833805995, -1.624782352598427959 ) ) ;
#3825 = EDGE_LOOP ( 'NONE', ( #652, #9347, #9995, #31273 ) ) ;
#3826 = ORIENTED_EDGE ( 'NONE', *, *, #33672, .T. ) ;
#3827 = EDGE_CURVE ( 'NONE', #32451, #22834, #32371, .T. ) ;
#3828 = DIRECTION ( 'NONE',  ( 1.000000000000000000, 1.734723475976807094E-16, -0.000000000000000000 ) ) ;
#3829 = EDGE_CURVE ( 'NONE', #2870, #4202, #18567, .T. ) ;
#3830 = AXIS2_PLACEMENT_3D ( 'NONE', #7768, #13015, #35515 ) ;
#3831 = CIRCLE ( 'NONE', #29114, 20.00000000000001066 ) ;
#3832 = SURFACE_SIDE_STYLE ('',( #7220 ) ) ;
#3833 = DIRECTION ( 'NONE',  ( -1.000000000000000000, 0.000000000000000000, -0.000000000000000000 ) ) ;
#3834 = ORIENTED_EDGE ( 'NONE', *, *, #26246, .F. ) ;
#3835 = ORIENTED_EDGE ( 'NONE', *, *, #12388, .T. ) ;
#3836 = CARTESIAN_POINT ( 'NONE',  ( -34.50000000000000000, -112.6919296022648638, -1.573728109100751116 ) ) ;
#3837 = CARTESIAN_POINT ( 'NONE',  ( 8.000000000000000000, 16.92083251265334098, -4.460989585140788805 ) ) ;
#3838 = ORIENTED_EDGE ( 'NONE', *, *, #25536, .T. ) ;
#3839 = ORIENTED_EDGE ( 'NONE', *, *, #5999, .F. ) ;
#3840 = AXIS2_PLACEMENT_3D ( 'NONE', #18949, #10329, #35538 ) ;
#3841 = DIRECTION ( 'NONE',  ( 0.000000000000000000, -1.000000000000000000, 0.000000000000000000 ) ) ;
#3842 = CIRCLE ( 'NONE', #18751, 20.00000000000000711 ) ;
#3843 = CARTESIAN_POINT ( 'NONE',  ( -37.50818044754229419, -113.9929510916434339, 13.11847460610629845 ) ) ;
#3844 = CARTESIAN_POINT ( 'NONE',  ( -34.50000000000000000, -113.6318576702834804, 1.956056246348823580 ) ) ;
#3845 = FACE_OUTER_BOUND ( 'NONE', #12614, .T. ) ;
#3846 = CARTESIAN_POINT ( 'NONE',  ( -35.50000000000000000, -113.9929510916434339, 10.85830208992344303 ) ) ;
#3847 = CARTESIAN_POINT ( 'NONE',  ( -35.50000000000000000, -115.9929524668003182, 10.51038305125561401 ) ) ;
#3848 = VECTOR ( 'NONE', #15769, 1000.000000000000000 ) ;
#3849 = UNCERTAINTY_MEASURE_WITH_UNIT (LENGTH_MEASURE( 1.000000000000000082E-05 ), #12860, 'distance_accuracy_value', 'NONE');
#3850 = CARTESIAN_POINT ( 'NONE',  ( 0.000000000000000000, -2.710505431213761085E-17, 45.10000000000000142 ) ) ;
#3851 = DIRECTION ( 'NONE',  ( 1.000000000000000000, -0.000000000000000000, 0.000000000000000000 ) ) ;
#3852 = AXIS2_PLACEMENT_3D ( 'NONE', #24445, #10762, #21729 ) ;
#3853 = CARTESIAN_POINT ( 'NONE',  ( -34.50000000000001421, -24.48076211353301801, 67.99999999999991473 ) ) ;
#3854 = DIRECTION ( 'NONE',  ( 0.000000000000000000, 0.9980267284282717810, -0.06279051952930990443 ) ) ;
#3855 = LINE ( 'NONE', #26160, #10555 ) ;
#3856 = AXIS2_PLACEMENT_3D ( 'NONE', #23588, #4164, #23041 ) ;
#3857 = EDGE_CURVE ( 'NONE', #15308, #17487, #9359, .T. ) ;
#3858 = ORIENTED_EDGE ( 'NONE', *, *, #26022, .F. ) ;
#3859 = VECTOR ( 'NONE', #13553, 1000.000000000000000 ) ;
#3860 = CARTESIAN_POINT ( 'NONE',  ( 70.00000000000001421, -30.47068043442695284, 93.33026027086508236 ) ) ;
#3861 = DIRECTION ( 'NONE',  ( -1.000000000000000000, -1.836970198721029934E-16, 0.000000000000000000 ) ) ;
#3862 = EDGE_CURVE ( 'NONE', #34739, #35010, #15810, .T. ) ;
#3863 = CARTESIAN_POINT ( 'NONE',  ( 8.000000000000000000, 2.494040418455352182, 18.62763138773848937 ) ) ;
#3864 = DIRECTION ( 'NONE',  ( -1.000000000000000000, -0.000000000000000000, -0.000000000000000000 ) ) ;
#3865 = CIRCLE ( 'NONE', #4425, 20.00000000000000355 ) ;
#3866 = VECTOR ( 'NONE', #21425, 1000.000000000000000 ) ;
#3867 = CARTESIAN_POINT ( 'NONE',  ( 4.000000000000000000, 12.46108038583334299, -15.64357617738982142 ) ) ;
#3868 = DIRECTION ( 'NONE',  ( 0.000000000000000000, 0.000000000000000000, 1.000000000000000000 ) ) ;
#3869 = ORIENTED_EDGE ( 'NONE', *, *, #12177, .T. ) ;
#3870 = CARTESIAN_POINT ( 'NONE',  ( 0.000000000000000000, -11.06713717293248855, 13.55483219355725844 ) ) ;
#3871 = CARTESIAN_POINT ( 'NONE',  ( -34.50000000000000000, -117.0140978167138854, -0.3747823525984421145 ) ) ;
#3872 = LINE ( 'NONE', #20383, #34097 ) ;
#3873 = VERTEX_POINT ( 'NONE', #10796 ) ;
#3874 = EDGE_LOOP ( 'NONE', ( #8444, #34699, #31317, #17340 ) ) ;
#3875 = CARTESIAN_POINT ( 'NONE',  ( -37.66520193420439000, -113.2509883718312977, 2.441024454178448710 ) ) ;
#3876 = VERTEX_POINT ( 'NONE', #21755 ) ;
#3877 = VERTEX_POINT ( 'NONE', #8076 ) ;
#3878 = ORIENTED_EDGE ( 'NONE', *, *, #2056, .F. ) ;
#3879 = CARTESIAN_POINT ( 'NONE',  ( -35.50000000000000000, -115.0140978167138428, -0.6247823525979866455 ) ) ;
#3880 = CIRCLE ( 'NONE', #7307, 6.000000000000005329 ) ;
#3881 = CARTESIAN_POINT ( 'NONE',  ( -35.50000000000000711, -116.0140978167138712, -0.4685323525984310677 ) ) ;
#3882 = AXIS2_PLACEMENT_3D ( 'NONE', #29379, #16190, #26505 ) ;
#3883 = CARTESIAN_POINT ( 'NONE',  ( 0.000000000000000000, 0.000000000000000000, 0.000000000000000000 ) ) ;
#3884 = AXIS2_PLACEMENT_3D ( 'NONE', #35496, #35323, #34973 ) ;
#3885 = CARTESIAN_POINT ( 'NONE',  ( -35.51597953369718397, -114.9929510916434339, 12.74811950270164473 ) ) ;
#3886 = CARTESIAN_POINT ( 'NONE',  ( -9.999999999999994671, 0.000000000000000000, 0.000000000000000000 ) ) ;
#3887 = AXIS2_PLACEMENT_3D ( 'NONE', #13127, #32366, #10236 ) ;
#3888 = AXIS2_PLACEMENT_3D ( 'NONE', #21872, #29638, #24069 ) ;
#3889 = DIRECTION ( 'NONE',  ( 0.000000000000000000, 0.000000000000000000, 1.000000000000000000 ) ) ;
#3890 = AXIS2_PLACEMENT_3D ( 'NONE', #22393, #7737, #31916 ) ;
#3891 = CARTESIAN_POINT ( 'NONE',  ( -34.50000000000000000, -114.9929510916434339, 11.73841344789270202 ) ) ;
#3892 = CYLINDRICAL_SURFACE ( 'NONE', #27210, 22.00000000000000000 ) ;
#3893 = PLANE ( 'NONE',  #22062 ) ;
#3894 = ORIENTED_EDGE ( 'NONE', *, *, #4681, .F. ) ;
#3895 = CARTESIAN_POINT ( 'NONE',  ( -35.50000000000000000, -114.1371041221139109, 8.509266650872710613 ) ) ;
#3896 = CARTESIAN_POINT ( 'NONE',  ( -35.50000000000000711, -112.0141053790792114, 0.9054673897245171243 ) ) ;
#3897 = FILL_AREA_STYLE ('',( #28549 ) ) ;
#3898 = DIRECTION ( 'NONE',  ( 0.000000000000000000, 0.000000000000000000, 1.000000000000000000 ) ) ;
#3899 = FACE_OUTER_BOUND ( 'NONE', #27076, .T. ) ;
#3900 = CIRCLE ( 'NONE', #3311, 4.000000000000000000 ) ;
#3901 = CARTESIAN_POINT ( 'NONE',  ( -50.00000000000000000, 10.00000000000000888, 120.0000000000000000 ) ) ;
#3902 = DIRECTION ( 'NONE',  ( -1.000000000000000000, 0.000000000000000000, 0.000000000000000000 ) ) ;
#3903 = EDGE_CURVE ( 'NONE', #30827, #35186, #19059, .T. ) ;
#3904 = AXIS2_PLACEMENT_3D ( 'NONE', #29304, #23350, #2133 ) ;
#3905 = CARTESIAN_POINT ( 'NONE',  ( -3.799999999999999822, 4.382607293638566128E-16, -45.00000000000000000 ) ) ;
#3906 = CARTESIAN_POINT ( 'NONE',  ( -46.00000000000000000, 0.000000000000000000, 0.000000000000000000 ) ) ;
#3907 = ORIENTED_EDGE ( 'NONE', *, *, #29480, .F. ) ;
#3908 = VECTOR ( 'NONE', #33852, 1000.000000000000000 ) ;
#3909 = CARTESIAN_POINT ( 'NONE',  ( -36.52652403469559061, -114.9754527089670262, 8.777725545821549957 ) ) ;
#3910 = VECTOR ( 'NONE', #4653, 999.9999999999998863 ) ;
#3911 = DIRECTION ( 'NONE',  ( 0.000000000000000000, -0.4999999999999989453, -0.8660254037844392627 ) ) ;
#3912 = VECTOR ( 'NONE', #31497, 1000.000000000000000 ) ;
#3913 = DIRECTION ( 'NONE',  ( 0.000000000000000000, -1.000000000000000000, 0.000000000000000000 ) ) ;
#3914 = ORIENTED_EDGE ( 'NONE', *, *, #24499, .T. ) ;
#3915 = ORIENTED_EDGE ( 'NONE', *, *, #34549, .F. ) ;
#3916 = AXIS2_PLACEMENT_3D ( 'NONE', #21919, #30216, #27526 ) ;
#3917 = LINE ( 'NONE', #1555, #26870 ) ;
#3918 = CARTESIAN_POINT ( 'NONE',  ( 7.999999999999992895, 11.46872990052381880, 45.56340405422447049 ) ) ;
#3919 = ORIENTED_EDGE ( 'NONE', *, *, #2451, .T. ) ;
#3920 = CARTESIAN_POINT ( 'NONE',  ( -39.07941549657749647, -116.1632251905417803, 9.058975545821549957 ) ) ;
#3921 = EDGE_CURVE ( 'NONE', #31804, #24979, #4867, .T. ) ;
#3922 = EDGE_LOOP ( 'NONE', ( #7495, #30740, #14943, #6320 ) ) ;
#3923 = CIRCLE ( 'NONE', #21170, 1.000000000000000444 ) ;
#3924 = CARTESIAN_POINT ( 'NONE',  ( 7.999999999999992895, 51.93417535146742381, 2.615612846549361770 ) ) ;
#3925 = CARTESIAN_POINT ( 'NONE',  ( 0.000000000000000000, 0.000000000000000000, 0.000000000000000000 ) ) ;
#3926 = DIRECTION ( 'NONE',  ( 0.000000000000000000, 0.5877852522924742473, -0.8090169943749466741 ) ) ;
#3927 = SHAPE_DEFINITION_REPRESENTATION ( #30770, #31430 ) ;
#3928 = DIRECTION ( 'NONE',  ( -0.000000000000000000, 0.000000000000000000, -1.000000000000000000 ) ) ;
#3929 = AXIS2_PLACEMENT_3D ( 'NONE', #18404, #4214, #29406 ) ;
#3930 = ORIENTED_EDGE ( 'NONE', *, *, #18025, .T. ) ;
#3931 = ORIENTED_EDGE ( 'NONE', *, *, #8792, .F. ) ;
#3932 = CARTESIAN_POINT ( 'NONE',  ( 70.00001200000002655, -29.17942948312593998, 82.54181312010028648 ) ) ;
#3933 = DIRECTION ( 'NONE',  ( 0.000000000000000000, 0.000000000000000000, -1.000000000000000000 ) ) ;
#3934 = AXIS2_PLACEMENT_3D ( 'NONE', #1260, #31326, #28984 ) ;
#3935 = VERTEX_POINT ( 'NONE', #10073 ) ;
#3936 = DIRECTION ( 'NONE',  ( 1.783119874454246424E-31, 1.187911941725854497E-31, -1.000000000000000000 ) ) ;
#3937 = CARTESIAN_POINT ( 'NONE',  ( -34.50000000000000000, -114.3474311500471572, -0.6247823525984269599 ) ) ;
#3938 = DIRECTION ( 'NONE',  ( 0.000000000000000000, 0.000000000000000000, 1.000000000000000000 ) ) ;
#3939 = FACE_OUTER_BOUND ( 'NONE', #23878, .T. ) ;
#3940 = AXIS2_PLACEMENT_3D ( 'NONE', #13568, #29787, #60 ) ;
#3941 =( REPRESENTATION_RELATIONSHIP ('NONE','NONE', #26607, #2005 ) REPRESENTATION_RELATIONSHIP_WITH_TRANSFORMATION ( #4395 )SHAPE_REPRESENTATION_RELATIONSHIP( ) );
#3942 = CARTESIAN_POINT ( 'NONE',  ( -34.50000000000000000, -115.1342778146718473, 8.846135899190283425 ) ) ;
#3943 = CYLINDRICAL_SURFACE ( 'NONE', #10566, 4.800000000000000711 ) ;
#3944 = DIRECTION ( 'NONE',  ( -1.000000000000000000, 0.000000000000000000, 0.000000000000000000 ) ) ;
#3945 = CARTESIAN_POINT ( 'NONE',  ( -39.00000000000000711, -114.9929510916434339, 12.44250253426874941 ) ) ;
#3946 = DIRECTION ( 'NONE',  ( -1.000000000000000000, 0.000000000000000000, 0.000000000000000000 ) ) ;
#3947 = VECTOR ( 'NONE', #24632, 1000.000000000000000 ) ;
#3948 = AXIS2_PLACEMENT_3D ( 'NONE', #11696, #33656, #8990 ) ;
#3949 = DIRECTION ( 'NONE',  ( 0.000000000000000000, 0.000000000000000000, 1.000000000000000000 ) ) ;
#3950 = ADVANCED_BREP_SHAPE_REPRESENTATION ( '', ( #33931, #21307 ), #6954 ) ;
#3951 = CARTESIAN_POINT ( 'NONE',  ( -42.49999999999999289, -38.78532556477436088, 79.33933265213893549 ) ) ;
#3952 = CARTESIAN_POINT ( 'NONE',  ( 0.000000000000000000, 0.000000000000000000, 49.10000000000000142 ) ) ;
#3953 = EDGE_CURVE ( 'NONE', #11172, #20834, #21039, .T. ) ;
#3954 = EDGE_CURVE ( 'NONE', #33383, #23477, #23189, .T. ) ;
#3955 = DIRECTION ( 'NONE',  ( 0.000000000000000000, -0.1253332335643113082, 0.9921147013144768767 ) ) ;
#3956 = VERTEX_POINT ( 'NONE', #30233 ) ;
#3957 = CARTESIAN_POINT ( 'NONE',  ( -36.94073759706868287, -116.9999999999999858, 4.371475545821550845 ) ) ;
#3958 = DIRECTION ( 'NONE',  ( -1.000000000000000000, 0.000000000000000000, 0.000000000000000000 ) ) ;
#3959 = CARTESIAN_POINT ( 'NONE',  ( -35.50000000000000000, -113.0140978167137717, 0.8903425666012282358 ) ) ;
#3960 = ORIENTED_EDGE ( 'NONE', *, *, #22376, .F. ) ;
#3961 = ORIENTED_EDGE ( 'NONE', *, *, #1805, .T. ) ;
#3962 = FACE_OUTER_BOUND ( 'NONE', #29901, .T. ) ;
#3963 = DIRECTION ( 'NONE',  ( 8.708451184622495809E-17, -6.938893903907203726E-17, -1.000000000000000000 ) ) ;
#3964 = EDGE_LOOP ( 'NONE', ( #35428, #3544 ) ) ;
#3965 = AXIS2_PLACEMENT_3D ( 'NONE', #10553, #103, #30006 ) ;
#3966 = ADVANCED_FACE ( 'NONE', ( #5911 ), #17055, .F. ) ;
#3967 = ORIENTED_EDGE ( 'NONE', *, *, #7911, .F. ) ;
#3968 = AXIS2_PLACEMENT_3D ( 'NONE', #33944, #20053, #805 ) ;
#3969 = CIRCLE ( 'NONE', #24668, 4.000000000000000000 ) ;
#3970 = LINE ( 'NONE', #17432, #19410 ) ;
#3971 = ORIENTED_EDGE ( 'NONE', *, *, #13368, .F. ) ;
#3972 = CARTESIAN_POINT ( 'NONE',  ( -36.94073759706868287, -115.9999999999999858, 5.871475545821550845 ) ) ;
#3973 = CARTESIAN_POINT ( 'NONE',  ( 8.000000000000000000, -18.62763138773852134, 2.494040418455287345 ) ) ;
#3974 = ORIENTED_EDGE ( 'NONE', *, *, #3455, .F. ) ;
#3975 = ORIENTED_EDGE ( 'NONE', *, *, #21561, .T. ) ;
#3976 = CARTESIAN_POINT ( 'NONE',  ( -35.50000000000000000, -111.0140978167138570, -0.5622823525984297355 ) ) ;
#3977 = CARTESIAN_POINT ( 'NONE',  ( 4.000000000000003553, -13.61301047812919762, 3.268936481846118625 ) ) ;
#3978 = ORIENTED_EDGE ( 'NONE', *, *, #17424, .T. ) ;
#3979 = CARTESIAN_POINT ( 'NONE',  ( -37.66108410722335265, -114.9929510916434339, 13.09299768411426790 ) ) ;
#3980 = EDGE_CURVE ( 'NONE', #26953, #19119, #24653, .T. ) ;
#3981 = CARTESIAN_POINT ( 'NONE',  ( -38.69949915733018742, -113.9929510916434339, 13.54034599209165890 ) ) ;
#3982 = DIRECTION ( 'NONE',  ( -1.000000000000000000, 0.000000000000000000, 0.000000000000000000 ) ) ;
#3983 = DIRECTION ( 'NONE',  ( -1.000000000000000000, 0.000000000000000000, 0.000000000000000000 ) ) ;
#3984 = CARTESIAN_POINT ( 'NONE',  ( -38.98797722933581866, -113.9929510916434339, 12.81430620224974959 ) ) ;
#3985 = DIRECTION ( 'NONE',  ( 0.000000000000000000, 0.000000000000000000, 1.000000000000000000 ) ) ;
#3986 = AXIS2_PLACEMENT_3D ( 'NONE', #14226, #27918, #9179 ) ;
#3987 = CARTESIAN_POINT ( 'NONE',  ( -35.50000000000000711, -114.9929510916434339, 12.44250253426871033 ) ) ;
#3988 = DIRECTION ( 'NONE',  ( 0.1305261922200477154, 0.9914448613738109373, 2.653430841701508438E-16 ) ) ;
#3989 = VERTEX_POINT ( 'NONE', #14928 ) ;
#3990 = AXIS2_PLACEMENT_3D ( 'NONE', #35024, #21301, #7619 ) ;
#3991 = CARTESIAN_POINT ( 'NONE',  ( -22.99999999999999289, -12.99999999999999645, 0.000000000000000000 ) ) ;
#3992 = FACE_OUTER_BOUND ( 'NONE', #30123, .T. ) ;
#3993 = EDGE_CURVE ( 'NONE', #20175, #14032, #8812, .T. ) ;
#3994 = ORIENTED_EDGE ( 'NONE', *, *, #2520, .F. ) ;
#3995 = ADVANCED_FACE ( 'NONE', ( #27543 ), #25364, .T. ) ;
#3996 = CARTESIAN_POINT ( 'NONE',  ( -35.50000000000000711, -114.9929510916434339, 10.52000928670414126 ) ) ;
#3997 = VERTEX_POINT ( 'NONE', #30578 ) ;
#3998 = ADVANCED_FACE ( 'NONE', ( #16876 ), #677, .T. ) ;
#3999 = CARTESIAN_POINT ( 'NONE',  ( -35.02454729103298803, -114.8876895276775087, 3.097274454178448710 ) ) ;
#4000 = ORIENTED_EDGE ( 'NONE', *, *, #7661, .T. ) ;
#4001 = DIRECTION ( 'NONE',  ( 0.000000000000000000, 0.000000000000000000, 1.000000000000000000 ) ) ;
#4002 = VERTEX_POINT ( 'NONE', #8601 ) ;
#4003 = CARTESIAN_POINT ( 'NONE',  ( -34.50000000000000000, -113.0601156079281253, 0.8807106166081309917 ) ) ;
#4004 = LINE ( 'NONE', #7208, #22490 ) ;
#4005 = CARTESIAN_POINT ( 'NONE',  ( -38.97545270896704039, -113.1123104723225197, 8.347274454178448266 ) ) ;
#4006 = EDGE_CURVE ( 'NONE', #34436, #17571, #35292, .T. ) ;
#4007 = ORIENTED_EDGE ( 'NONE', *, *, #2084, .T. ) ;
#4008 = CARTESIAN_POINT ( 'NONE',  ( -35.00000000000000000, -114.0592624029313242, 4.503524454178448266 ) ) ;
#4009 = EDGE_CURVE ( 'NONE', #2675, #28676, #774, .T. ) ;
#4010 = LINE ( 'NONE', #23061, #19935 ) ;
#4011 = CARTESIAN_POINT ( 'NONE',  ( -35.50000000000000711, -113.8474311500459777, -1.624782352598427959 ) ) ;
#4012 = VERTEX_POINT ( 'NONE', #13841 ) ;
#4013 = ORIENTED_EDGE ( 'NONE', *, *, #27941, .F. ) ;
#4014 = DIRECTION ( 'NONE',  ( 0.000000000000000000, 0.000000000000000000, -1.000000000000000000 ) ) ;
#4015 = VECTOR ( 'NONE', #13104, 1000.000000000000000 ) ;
#4016 = DIRECTION ( 'NONE',  ( -1.000000000000000000, 0.000000000000000000, 0.000000000000000000 ) ) ;
#4017 = ORIENTED_EDGE ( 'NONE', *, *, #14512, .T. ) ;
#4018 = VERTEX_POINT ( 'NONE', #21935 ) ;
#4019 = CIRCLE ( 'NONE', #19505, 0.1999999999999998723 ) ;
#4020 = CARTESIAN_POINT ( 'NONE',  ( -34.50000000000000000, -113.2372261171341563, 2.916049522752222511 ) ) ;
#4021 = CARTESIAN_POINT ( 'NONE',  ( -35.50000000000000711, -112.8655373925166572, 1.864575885149403423 ) ) ;
#4022 = AXIS2_PLACEMENT_3D ( 'NONE', #15964, #23913, #4302 ) ;
#4023 = ORIENTED_EDGE ( 'NONE', *, *, #27764, .F. ) ;
#4024 = ORIENTED_EDGE ( 'NONE', *, *, #74, .F. ) ;
#4025 = CARTESIAN_POINT ( 'NONE',  ( 0.000000000000000000, -2.710505431213761085E-17, -21.89999999999999858 ) ) ;
#4026 = EDGE_CURVE ( 'NONE', #29368, #30768, #4813, .T. ) ;
#4027 = CARTESIAN_POINT ( 'NONE',  ( -36.00585935943765747, -113.9929510916434339, 13.11852578240983291 ) ) ;
#4028 = EDGE_CURVE ( 'NONE', #20179, #14725, #27358, .T. ) ;
#4029 = DIRECTION ( 'NONE',  ( 0.000000000000000000, 0.000000000000000000, 1.000000000000000000 ) ) ;
#4030 = ADVANCED_FACE ( 'NONE', ( #32930 ), #14188, .F. ) ;
#4031 = CARTESIAN_POINT ( 'NONE',  ( -35.99386409314529800, -113.9929510916434339, 13.11852378322482515 ) ) ;
#4032 = CARTESIAN_POINT ( 'NONE',  ( -35.50000000000000000, -115.9929510916434481, 12.56351784598954424 ) ) ;
#4033 = DIRECTION ( 'NONE',  ( 0.000000000000000000, 0.000000000000000000, -1.000000000000000000 ) ) ;
#4034 = DIRECTION ( 'NONE',  ( 0.000000000000000000, 1.000000000000000000, 0.000000000000000000 ) ) ;
#4035 = EDGE_CURVE ( 'NONE', #31214, #35587, #27806, .T. ) ;
#4036 = EDGE_CURVE ( 'NONE', #4537, #12439, #11122, .T. ) ;
#4037 = CARTESIAN_POINT ( 'NONE',  ( -21.15833593587365513, -21.98076211353320630, 83.49999999999994316 ) ) ;
#4038 = CARTESIAN_POINT ( 'NONE',  ( 8.000000000000000000, 19.83898331853701080, -9.508666619816441568 ) ) ;
#4039 = DIRECTION ( 'NONE',  ( -1.734723475976806848E-16, -0.8660254037844350439, -0.5000000000000061062 ) ) ;
#4040 = VERTEX_POINT ( 'NONE', #11491 ) ;
#4041 = AXIS2_PLACEMENT_3D ( 'NONE', #12019, #1576, #6789 ) ;
#4042 = PLANE ( 'NONE',  #23335 ) ;
#4043 = CARTESIAN_POINT ( 'NONE',  ( -35.50000000000000711, -112.9185811467682754, 1.870920967077121411 ) ) ;
#4044 = CARTESIAN_POINT ( 'NONE',  ( -21.15833593587365513, -27.48076211353330578, 101.9999999999999432 ) ) ;
#4045 = CONTEXT_DEPENDENT_SHAPE_REPRESENTATION ( #34051, #8403 ) ;
#4046 = AXIS2_PLACEMENT_3D ( 'NONE', #8922, #31077, #28028 ) ;
#4047 = CARTESIAN_POINT ( 'NONE',  ( -35.69809690994938478, -111.0245472910330022, 2.722274454178449155 ) ) ;
#4048 = AXIS2_PLACEMENT_3D ( 'NONE', #13665, #5221, #32392 ) ;
#4049 = LINE ( 'NONE', #7251, #31390 ) ;
#4050 = FACE_OUTER_BOUND ( 'NONE', #30940, .T. ) ;
#4051 = EDGE_CURVE ( 'NONE', #33849, #2400, #5948, .T. ) ;
#4052 = ORIENTED_EDGE ( 'NONE', *, *, #12390, .F. ) ;
#4053 = CARTESIAN_POINT ( 'NONE',  ( 1.398397006337009918, -6.091550361990587525, -0.7999999999999951594 ) ) ;
#4054 = CARTESIAN_POINT ( 'NONE',  ( -34.50000000000000000, -113.1807644833805426, -2.624782352598442614 ) ) ;
#4055 = DIRECTION ( 'NONE',  ( -1.000000000000000000, 0.000000000000000000, 0.000000000000000000 ) ) ;
#4056 = ORIENTED_EDGE ( 'NONE', *, *, #34152, .F. ) ;
#4057 = ORIENTED_EDGE ( 'NONE', *, *, #3575, .T. ) ;
#4058 = CARTESIAN_POINT ( 'NONE',  ( -38.02454729103296671, -114.3549511594417396, 3.659774454178448710 ) ) ;
#4059 = VERTEX_POINT ( 'NONE', #33622 ) ;
#4060 =( LENGTH_UNIT ( ) NAMED_UNIT ( * ) SI_UNIT ( .MILLI., .METRE. ) );
#4061 = VERTEX_POINT ( 'NONE', #8955 ) ;
#4062 = VERTEX_POINT ( 'NONE', #5398 ) ;
#4063 = CARTESIAN_POINT ( 'NONE',  ( -34.50000000000000000, -113.0256022645180707, 0.8765908897032291813 ) ) ;
#4064 = AXIS2_PLACEMENT_3D ( 'NONE', #2078, #10162, #24205 ) ;
#4065 = CARTESIAN_POINT ( 'NONE',  ( 8.000000000000000000, 14.48509162075963985, 8.733917826871412160 ) ) ;
#4066 = EDGE_CURVE ( 'NONE', #17047, #11373, #2879, .T. ) ;
#4067 = DIRECTION ( 'NONE',  ( 0.000000000000000000, 0.000000000000000000, 1.000000000000000000 ) ) ;
#4068 = AXIS2_PLACEMENT_3D ( 'NONE', #11325, #33289, #8606 ) ;
#4069 = ADVANCED_FACE ( 'NONE', ( #9499 ), #28946, .T. ) ;
#4070 = CARTESIAN_POINT ( 'NONE',  ( -35.50000000000000711, -114.9929510916434339, 11.73841344789270202 ) ) ;
#4071 = EDGE_CURVE ( 'NONE', #11477, #29543, #3673, .T. ) ;
#4072 = CARTESIAN_POINT ( 'NONE',  ( 1.498621416870293821, 0.000000000000000000, 0.000000000000000000 ) ) ;
#4073 = AXIS2_PLACEMENT_3D ( 'NONE', #16633, #27647, #35216 ) ;
#4074 = DIRECTION ( 'NONE',  ( 1.000000000000000000, -0.000000000000000000, -0.000000000000000000 ) ) ;
#4075 = CARTESIAN_POINT ( 'NONE',  ( -37.46093750000000711, -114.9929510916434339, 14.11852480586264846 ) ) ;
#4076 = LINE ( 'NONE', #23301, #31790 ) ;
#4077 = PRODUCT ( 'BR-594', 'BR-594', '', ( #19045 ) ) ;
#4078 = EDGE_CURVE ( 'NONE', #20179, #3685, #18014, .T. ) ;
#4079 = CARTESIAN_POINT ( 'NONE',  ( -3.799999999999999822, 4.382607293638566128E-16, 29.09999999999999787 ) ) ;
#4080 = ORIENTED_EDGE ( 'NONE', *, *, #33432, .T. ) ;
#4081 = CARTESIAN_POINT ( 'NONE',  ( -35.50000000000000000, -115.6492853190479337, 9.359470924297957239 ) ) ;
#4082 = CARTESIAN_POINT ( 'NONE',  ( -35.50000000000000711, -112.6919296022648638, -1.573728109100751116 ) ) ;
#4083 = CARTESIAN_POINT ( 'NONE',  ( -1.799999999999996048, 0.000000000000000000, 0.000000000000000000 ) ) ;
#4084 = EDGE_CURVE ( 'NONE', #29056, #20040, #34118, .T. ) ;
#4085 = CARTESIAN_POINT ( 'NONE',  ( 2.321707774797385326, -4.824281976788927118, -0.7999999999999951594 ) ) ;
#4086 = DIRECTION ( 'NONE',  ( 0.000000000000000000, 0.9672551082808338307, -0.2538061376417690695 ) ) ;
#4087 = CARTESIAN_POINT ( 'NONE',  ( -39.49999999999999289, -9.059673409587547965, 113.4689433211305811 ) ) ;
#4088 = DIRECTION ( 'NONE',  ( 0.000000000000000000, 0.000000000000000000, 1.000000000000000000 ) ) ;
#4089 = CYLINDRICAL_SURFACE ( 'NONE', #34332, 7.000000000000035527 ) ;
#4090 = CARTESIAN_POINT ( 'NONE',  ( -42.49999999999999289, -27.48076211353330578, 101.9999999999999432 ) ) ;
#4091 = VERTEX_POINT ( 'NONE', #26072 ) ;
#4092 = AXIS2_PLACEMENT_3D ( 'NONE', #23943, #1135, #23079 ) ;
#4093 = CARTESIAN_POINT ( 'NONE',  ( -37.47347596530441649, -113.0245472910329880, 8.027725545821551734 ) ) ;
#4094 = LINE ( 'NONE', #22599, #19795 ) ;
#4095 = FACE_OUTER_BOUND ( 'NONE', #13543, .T. ) ;
#4096 = ORIENTED_EDGE ( 'NONE', *, *, #7699, .F. ) ;
#4097 = ORIENTED_EDGE ( 'NONE', *, *, #16943, .F. ) ;
#4098 = CARTESIAN_POINT ( 'NONE',  ( 4.000000000000003553, -40.47821179127691238, -32.64221760512803172 ) ) ;
#4099 = ORIENTED_EDGE ( 'NONE', *, *, #1997, .F. ) ;
#4100 = CARTESIAN_POINT ( 'NONE',  ( -35.81662171581203324, -110.9754527089670546, 6.715225545821551734 ) ) ;
#4101 = VERTEX_POINT ( 'NONE', #3577 ) ;
#4102 = AXIS2_PLACEMENT_3D ( 'NONE', #29592, #17872, #13027 ) ;
#4103 = CIRCLE ( 'NONE', #624, 0.9999999999999974465 ) ;
#4104 = LINE ( 'NONE', #18469, #31061 ) ;
#4105 = CARTESIAN_POINT ( 'NONE',  ( 8.000000000000000000, -16.53603053422215297, 8.931325931664547468 ) ) ;
#4106 = CYLINDRICAL_SURFACE ( 'NONE', #7372, 8.000000000000001776 ) ;
#4107 = APPLICATION_PROTOCOL_DEFINITION ( 'draft international standard', 'automotive_design', 1998, #25537 ) ;
#4108 = CARTESIAN_POINT ( 'NONE',  ( 0.000000000000000000, -2.710505431213761085E-17, 45.89999999999999858 ) ) ;
#4109 = VERTEX_POINT ( 'NONE', #31470 ) ;
#4110 = ORIENTED_EDGE ( 'NONE', *, *, #7792, .F. ) ;
#4111 = ADVANCED_FACE ( 'NONE', ( #25901, #17767 ), #23356, .T. ) ;
#4112 = DIRECTION ( 'NONE',  ( 1.174092375852890260E-15, -4.222049128630259891E-16, -1.000000000000000000 ) ) ;
#4113 = CARTESIAN_POINT ( 'NONE',  ( -34.49999999999998579, -13.10640646055107084, 90.70096189432331357 ) ) ;
#4114 = VERTEX_POINT ( 'NONE', #34175 ) ;
#4115 = DIRECTION ( 'NONE',  ( 1.000000000000000000, 0.000000000000000000, 0.000000000000000000 ) ) ;
#4116 = CARTESIAN_POINT ( 'NONE',  ( -34.50000000000000000, -115.0140978167137860, -0.6411448143358557950 ) ) ;
#4117 = DIRECTION ( 'NONE',  ( -1.000000000000000000, 0.000000000000000000, 0.000000000000000000 ) ) ;
#4118 = DIRECTION ( 'NONE',  ( 0.000000000000000000, 0.000000000000000000, 1.000000000000000000 ) ) ;
#4119 = CARTESIAN_POINT ( 'NONE',  ( -37.43749999999998579, -115.9929510916434481, 14.11852480586265024 ) ) ;
#4120 = DIRECTION ( 'NONE',  ( 0.000000000000000000, 0.9510565162951523099, 0.3090169943749513926 ) ) ;
#4121 = CARTESIAN_POINT ( 'NONE',  ( 8.000000000000000000, -18.48663108841361336, 3.384281271887747078 ) ) ;
#4122 = AXIS2_PLACEMENT_3D ( 'NONE', #33510, #19985, #28297 ) ;
#4123 = CARTESIAN_POINT ( 'NONE',  ( -37.54906985245724371, -114.9929510916434339, 14.11777216781844579 ) ) ;
#4125 = DIRECTION ( 'NONE',  ( -1.000000000000000000, 0.000000000000000000, 0.000000000000000000 ) ) ;
#4124 = AXIS2_PLACEMENT_3D ( 'NONE', #1615, #29162, #4322 ) ;
#4126 = LINE ( 'NONE', #34003, #8071 ) ;
#4127 = DIRECTION ( 'NONE',  ( 0.000000000000000000, 0.000000000000000000, 1.000000000000000000 ) ) ;
#4128 = CARTESIAN_POINT ( 'NONE',  ( 0.000000000000000000, -8.605879768205326741, 12.89022243466705930 ) ) ;
#4129 = FACE_BOUND ( 'NONE', #21760, .T. ) ;
#4130 = ORIENTED_EDGE ( 'NONE', *, *, #12569, .F. ) ;
#4131 = CARTESIAN_POINT ( 'NONE',  ( -39.07941549657749647, -116.1632251905417803, 3.058975545821551734 ) ) ;
#4132 = PLANE ( 'NONE',  #16368 ) ;
#4133 = CARTESIAN_POINT ( 'NONE',  ( -35.50000000000000000, -113.0140978167138996, -0.6247823525984302906 ) ) ;
#4134 = ORIENTED_EDGE ( 'NONE', *, *, #30362, .T. ) ;
#4135 = ORIENTED_EDGE ( 'NONE', *, *, #2507, .T. ) ;
#4136 =( NAMED_UNIT ( * ) SI_UNIT ( $, .STERADIAN. ) SOLID_ANGLE_UNIT ( ) );
#4137 = LINE ( 'NONE', #6988, #4291 ) ;
#4138 = VERTEX_POINT ( 'NONE', #17231 ) ;
#4139 = ORIENTED_EDGE ( 'NONE', *, *, #11974, .F. ) ;
#4140 = ORIENTED_EDGE ( 'NONE', *, *, #17735, .F. ) ;
#4141 = DIRECTION ( 'NONE',  ( -1.000000000000000000, -0.000000000000000000, 0.000000000000000000 ) ) ;
#4142 = CARTESIAN_POINT ( 'NONE',  ( -38.45611840935523418, -112.6276912846090568, 4.933975545821551734 ) ) ;
#4143 = VECTOR ( 'NONE', #7228, 1000.000000000000000 ) ;
#4144 = CIRCLE ( 'NONE', #34024, 20.00000000000001066 ) ;
#4145 = CARTESIAN_POINT ( 'NONE',  ( 0.000000000000000000, 0.000000000000000000, 0.000000000000000000 ) ) ;
#4146 = DIRECTION ( 'NONE',  ( -1.000000000000000000, 0.000000000000000000, 0.000000000000000000 ) ) ;
#4147 = EDGE_LOOP ( 'NONE', ( #20861, #5933, #23613, #20709 ) ) ;
#4148 = EDGE_LOOP ( 'NONE', ( #3038, #28387, #26592, #11205 ) ) ;
#4149 = CARTESIAN_POINT ( 'NONE',  ( -35.50000000000000000, -114.9515981487115823, -2.624803185604625000 ) ) ;
#4150 = EDGE_CURVE ( 'NONE', #34739, #8636, #26079, .T. ) ;
#4151 = DIRECTION ( 'NONE',  ( 1.000000000000000000, 0.000000000000000000, 0.000000000000000000 ) ) ;
#4152 = CARTESIAN_POINT ( 'NONE',  ( 7.999999999999992895, 0.000000000000000000, 0.000000000000000000 ) ) ;
#4153 = ORIENTED_EDGE ( 'NONE', *, *, #25314, .F. ) ;
#4154 = FACE_OUTER_BOUND ( 'NONE', #29496, .T. ) ;
#4155 = STYLED_ITEM ( 'NONE', ( #23497 ), #22590 ) ;
#4156 = CARTESIAN_POINT ( 'NONE',  ( -34.50000000000000000, -114.1302255537607095, 9.515717283514957714 ) ) ;
#4157 = DIRECTION ( 'NONE',  ( -1.000000000000000000, 0.000000000000000000, 0.000000000000000000 ) ) ;
#4158 = CARTESIAN_POINT ( 'NONE',  ( -36.87500000000098055, -114.9929510916434339, 13.11852480586264669 ) ) ;
#4159 = DIRECTION ( 'NONE',  ( -1.000000000000000000, 0.000000000000000000, 0.000000000000000000 ) ) ;
#4160 = EDGE_CURVE ( 'NONE', #34443, #26484, #18590, .T. ) ;
#4161 = CARTESIAN_POINT ( 'NONE',  ( -36.07812499999994316, -113.9929510916434339, 14.11852480586265024 ) ) ;
#4162 = DIRECTION ( 'NONE',  ( 1.000000000000000000, 0.000000000000000000, -0.000000000000000000 ) ) ;
#4163 = CARTESIAN_POINT ( 'NONE',  ( -37.46093750000000711, -114.9929510916434339, 13.11852480586264669 ) ) ;
#4164 = DIRECTION ( 'NONE',  ( -1.000000000000000000, 0.000000000000000000, 0.000000000000000000 ) ) ;
#4165 = ORIENTED_EDGE ( 'NONE', *, *, #28596, .T. ) ;
#4166 = DIRECTION ( 'NONE',  ( -0.000000000000000000, 0.000000000000000000, -1.000000000000000000 ) ) ;
#4167 = CARTESIAN_POINT ( 'NONE',  ( 0.000000000000000000, 0.000000000000000000, 55.00000000000000000 ) ) ;
#4168 = ORIENTED_EDGE ( 'NONE', *, *, #7385, .F. ) ;
#4169 = CARTESIAN_POINT ( 'NONE',  ( -35.50160444427493189, -114.9929510916434339, 12.65937477241749853 ) ) ;
#4170 = EDGE_LOOP ( 'NONE', ( #11152, #15433, #25560, #1166 ) ) ;
#4171 = CIRCLE ( 'NONE', #12797, 8.000000000000010658 ) ;
#4172 = AXIS2_PLACEMENT_3D ( 'NONE', #35236, #18650, #16115 ) ;
#4173 = CARTESIAN_POINT ( 'NONE',  ( 7.999999999999992895, 0.000000000000000000, 0.000000000000000000 ) ) ;
#4174 = ORIENTED_EDGE ( 'NONE', *, *, #21174, .F. ) ;
#4175 = LINE ( 'NONE', #15115, #16469 ) ;
#4176 = ORIENTED_EDGE ( 'NONE', *, *, #30877, .T. ) ;
#4177 = CARTESIAN_POINT ( 'NONE',  ( -34.50000000000000000, -113.7503824761461004, 0.9631051547057219997 ) ) ;
#4178 = CARTESIAN_POINT ( 'NONE',  ( 8.000000000000007105, 0.000000000000000000, 0.000000000000000000 ) ) ;
#4179 = CARTESIAN_POINT ( 'NONE',  ( -35.02454729103298803, -114.8876895276775087, 7.597274454178450931 ) ) ;
#4180 = VERTEX_POINT ( 'NONE', #26245 ) ;
#4181 = CARTESIAN_POINT ( 'NONE',  ( -37.88768952767750164, -115.9754527089670262, 6.472274454178450043 ) ) ;
#4182 = EDGE_CURVE ( 'NONE', #185, #31659, #32397, .T. ) ;
#4183 = PRESENTATION_LAYER_ASSIGNMENT (  '', '', ( #8745 ) ) ;
#4184 = DIRECTION ( 'NONE',  ( -1.000000000000000000, -1.734723475976807094E-16, 0.000000000000000000 ) ) ;
#4185 = CARTESIAN_POINT ( 'NONE',  ( -35.50000000000000711, -113.1807644833805426, -1.624782352598427959 ) ) ;
#4186 = ORIENTED_EDGE ( 'NONE', *, *, #27677, .T. ) ;
#4187 = VERTEX_POINT ( 'NONE', #19920 ) ;
#4188 = AXIS2_PLACEMENT_3D ( 'NONE', #2479, #21713, #7674 ) ;
#4189 = DIRECTION ( 'NONE',  ( 1.387778780781445922E-16, -1.000000000000000000, 0.000000000000000000 ) ) ;
#4190 = SURFACE_STYLE_USAGE ( .BOTH. , #34607 ) ;
#4191 = CARTESIAN_POINT ( 'NONE',  ( -1.799999999999996048, 1.534828951630468330E-15, 8.000000000000051514 ) ) ;
#4192 = ORIENTED_EDGE ( 'NONE', *, *, #26875, .T. ) ;
#4193 = VERTEX_POINT ( 'NONE', #6439 ) ;
#4194 = CARTESIAN_POINT ( 'NONE',  ( -34.50000000000000000, -116.0060826362711595, -0.7553032835231661135 ) ) ;
#4195 = CARTESIAN_POINT ( 'NONE',  ( -35.50000000000000711, -112.1859307030124739, 1.448610958621386224 ) ) ;
#4196 = ADVANCED_FACE ( 'NONE', ( #12206 ), #33817, .T. ) ;
#4197 = AXIS2_PLACEMENT_3D ( 'NONE', #4744, #4912, #13362 ) ;
#4198 = EDGE_CURVE ( 'NONE', #1742, #29371, #15235, .T. ) ;
#4199 = CARTESIAN_POINT ( 'NONE',  ( 0.000000000000000000, -39.55064067543046491, -25.36340625197400200 ) ) ;
#4200 = ORIENTED_EDGE ( 'NONE', *, *, #30836, .T. ) ;
#4201 = AXIS2_PLACEMENT_3D ( 'NONE', #28271, #13396, #14390 ) ;
#4202 = VERTEX_POINT ( 'NONE', #33997 ) ;
#4203 = CARTESIAN_POINT ( 'NONE',  ( -23.00000000000000355, 3.857637417314161900E-15, 0.000000000000000000 ) ) ;
#4204 = CARTESIAN_POINT ( 'NONE',  ( -37.46093750000000711, -113.9929510916434339, 13.11852480586264846 ) ) ;
#4205 = DIRECTION ( 'NONE',  ( -1.000000000000000000, 0.000000000000000000, 0.000000000000000000 ) ) ;
#4206 = EDGE_CURVE ( 'NONE', #34373, #35474, #34924, .T. ) ;
#4207 = CARTESIAN_POINT ( 'NONE',  ( -37.18750000000004974, -113.9929510916434339, 13.11852480586264846 ) ) ;
#4208 = ADVANCED_FACE ( 'NONE', ( #13972, #6046, #32712, #19698, #2659 ), #32888, .T. ) ;
#4209 = CARTESIAN_POINT ( 'NONE',  ( -35.50100302244945993, -115.9929510916434481, 12.65121853911337446 ) ) ;
#4210 = CARTESIAN_POINT ( 'NONE',  ( 0.1085714285714300953, -3.798448662927791819, -0.7999999999999951594 ) ) ;
#4211 = AXIS2_PLACEMENT_3D ( 'NONE', #20845, #28800, #12952 ) ;
#4212 = CYLINDRICAL_SURFACE ( 'NONE', #27884, 8.000000000000007105 ) ;
#4213 = ORIENTED_EDGE ( 'NONE', *, *, #26015, .F. ) ;
#4214 = DIRECTION ( 'NONE',  ( -1.000000000000000000, 0.000000000000000000, 0.000000000000000000 ) ) ;
#4215 = CYLINDRICAL_SURFACE ( 'NONE', #24885, 6.000000000000005329 ) ;
#4216 = DIRECTION ( 'NONE',  ( 1.000000000000000000, 0.000000000000000000, 0.000000000000000000 ) ) ;
#4217 = ORIENTED_EDGE ( 'NONE', *, *, #22440, .F. ) ;
#4218 = CARTESIAN_POINT ( 'NONE',  ( 0.000000000000000000, 0.000000000000000000, 0.000000000000000000 ) ) ;
#4219 = AXIS2_PLACEMENT_3D ( 'NONE', #29701, #27009, #15634 ) ;
#4220 = CARTESIAN_POINT ( 'NONE',  ( -35.50000000000000711, -113.6807644833805995, -1.624782352598427959 ) ) ;
#4221 = CYLINDRICAL_SURFACE ( 'NONE', #5807, 2.999999999999988898 ) ;
#4222 = ITEM_DEFINED_TRANSFORMATION ( 'NONE', 'NONE', #5257,  #21307 ) ;
#4223 = DIRECTION ( 'NONE',  ( 0.000000000000000000, 0.8660254037844364872, 0.5000000000000036637 ) ) ;
#4224 = DIRECTION ( 'NONE',  ( 0.000000000000000000, 0.000000000000000000, -1.000000000000000000 ) ) ;
#4225 = EDGE_CURVE ( 'NONE', #11477, #19439, #7096, .T. ) ;
#4226 = ORIENTED_EDGE ( 'NONE', *, *, #7057, .F. ) ;
#4227 = DIRECTION ( 'NONE',  ( -1.000000000000000000, -0.000000000000000000, 0.000000000000000000 ) ) ;
#4228 = CARTESIAN_POINT ( 'NONE',  ( -34.50000000000000000, -116.9501796819249222, -1.143161139954000260 ) ) ;
#4229 = DIRECTION ( 'NONE',  ( 1.000000000000000000, 0.000000000000000000, 0.000000000000000000 ) ) ;
#4230 = ORIENTED_EDGE ( 'NONE', *, *, #20513, .F. ) ;
#4231 = VERTEX_POINT ( 'NONE', #27841 ) ;
#4232 = CARTESIAN_POINT ( 'NONE',  ( -37.47347596530441649, -114.9754527089670262, 3.472274454178448710 ) ) ;
#4234 = ORIENTED_EDGE ( 'NONE', *, *, #24706, .T. ) ;
#4233 = AXIS2_PLACEMENT_3D ( 'NONE', #17798, #34393, #9712 ) ;
#4235 = ORIENTED_EDGE ( 'NONE', *, *, #8593, .T. ) ;
#4236 = CARTESIAN_POINT ( 'NONE',  ( -35.50000000000000000, -115.0140978167138712, -0.6247823525985405357 ) ) ;
#4237 = ADVANCED_FACE ( 'NONE', ( #22415 ), #27501, .T. ) ;
#4238 = EDGE_CURVE ( 'NONE', #18735, #11499, #5355, .T. ) ;
#4239 = ADVANCED_FACE ( 'NONE', ( #19021, #14312 ), #28018, .F. ) ;
#4240 = DIRECTION ( 'NONE',  ( 0.000000000000000000, 0.000000000000000000, -1.000000000000000000 ) ) ;
#4241 = DIRECTION ( 'NONE',  ( 0.000000000000000000, 0.000000000000000000, 1.000000000000000000 ) ) ;
#4242 = CIRCLE ( 'NONE', #30675, 4.499999999999990230 ) ;
#4243 = CARTESIAN_POINT ( 'NONE',  ( -35.50000000000000711, -114.9929510916434339, 12.60752341388803544 ) ) ;
#4244 = AXIS2_PLACEMENT_3D ( 'NONE', #17585, #20457, #6796 ) ;
#4245 = CARTESIAN_POINT ( 'NONE',  ( -1.519999999999993578, 0.000000000000000000, 0.000000000000000000 ) ) ;
#4246 = EDGE_CURVE ( 'NONE', #20080, #7610, #9387, .T. ) ;
#4247 = CARTESIAN_POINT ( 'NONE',  ( -36.62499999999902656, -114.9929510916434339, 14.11852480586264846 ) ) ;
#4248 = CARTESIAN_POINT ( 'NONE',  ( 0.000000000000000000, 0.000000000000000000, 0.000000000000000000 ) ) ;
#4249 = CARTESIAN_POINT ( 'NONE',  ( 0.000000000000000000, -2.710505431213761085E-17, 29.09999999999999787 ) ) ;
#4250 = VERTEX_POINT ( 'NONE', #25140 ) ;
#4251 = CARTESIAN_POINT ( 'NONE',  ( -35.50000000000000000, -115.9929510916434481, 12.56351784598954424 ) ) ;
#4252 = CARTESIAN_POINT ( 'NONE',  ( -35.50000000000000711, -113.3474311500483935, -1.624782352598427959 ) ) ;
#4253 = DIRECTION ( 'NONE',  ( -1.000000000000000000, 0.000000000000000000, 0.000000000000000000 ) ) ;
#4254 = DIRECTION ( 'NONE',  ( 0.000000000000000000, 0.000000000000000000, 1.000000000000000000 ) ) ;
#4255 = CARTESIAN_POINT ( 'NONE',  ( 0.000000000000000000, 0.000000000000000000, 60.00000000000000000 ) ) ;
#4256 = VECTOR ( 'NONE', #16966, 1000.000000000000000 ) ;
#4257 = CARTESIAN_POINT ( 'NONE',  ( 7.999999999999992895, 30.03615769709793426, -42.44795908868959344 ) ) ;
#4258 = CARTESIAN_POINT ( 'NONE',  ( 0.000000000000000000, 0.000000000000000000, 0.000000000000000000 ) ) ;
#4259 = DIRECTION ( 'NONE',  ( -1.734723475976807094E-16, 1.000000000000000000, 0.000000000000000000 ) ) ;
#4260 = CARTESIAN_POINT ( 'NONE',  ( 0.000000000000000000, -2.710505431213761085E-17, 45.89999999999999858 ) ) ;
#4261 = ORIENTED_EDGE ( 'NONE', *, *, #7748, .T. ) ;
#4262 = CARTESIAN_POINT ( 'NONE',  ( -37.05926240293131713, -113.0000000000000000, 8.121475545821549957 ) ) ;
#4263 = CYLINDRICAL_SURFACE ( 'NONE', #33096, 9.999999999999994671 ) ;
#4264 = DIRECTION ( 'NONE',  ( -1.000000000000000000, 0.000000000000000000, 0.000000000000000000 ) ) ;
#4265 = EDGE_CURVE ( 'NONE', #3873, #375, #11694, .T. ) ;
#4266 = ORIENTED_EDGE ( 'NONE', *, *, #13822, .F. ) ;
#4267 = ORIENTED_EDGE ( 'NONE', *, *, #7475, .F. ) ;
#4268 = VECTOR ( 'NONE', #34963, 1000.000000000000000 ) ;
#4269 = CARTESIAN_POINT ( 'NONE',  ( 0.000000000000000000, 5.400000000000098943, 1.000000000000000888 ) ) ;
#4270 = CIRCLE ( 'NONE', #19766, 52.00000000000000711 ) ;
#4271 = EDGE_CURVE ( 'NONE', #2854, #9753, #31822, .T. ) ;
#4272 = CARTESIAN_POINT ( 'NONE',  ( -34.49999999999998579, -38.78532556477446036, 90.66066734786068082 ) ) ;
#4273 = ORIENTED_EDGE ( 'NONE', *, *, #14515, .F. ) ;
#4274 = CARTESIAN_POINT ( 'NONE',  ( -39.07941549657749647, -116.1632251905417803, 7.558975545821551734 ) ) ;
#4275 = ORIENTED_EDGE ( 'NONE', *, *, #12327, .F. ) ;
#4276 = CARTESIAN_POINT ( 'NONE',  ( 0.000000000000000000, 3.268936481846187903, 13.61301047812924025 ) ) ;
#4277 = ORIENTED_EDGE ( 'NONE', *, *, #33464, .T. ) ;
#4278 = DIRECTION ( 'NONE',  ( 0.000000000000000000, 0.7705132427757861446, 0.6374239897486934092 ) ) ;
#4279 = DIRECTION ( 'NONE',  ( -1.000000000000000000, -0.000000000000000000, -0.000000000000000000 ) ) ;
#4280 = EDGE_CURVE ( 'NONE', #30634, #22786, #19147, .T. ) ;
#4281 = EDGE_CURVE ( 'NONE', #11309, #17651, #27314, .T. ) ;
#4282 = CARTESIAN_POINT ( 'NONE',  ( 0.000000000000000000, -43.55304910509426009, 28.41006711799970574 ) ) ;
#4283 = EDGE_LOOP ( 'NONE', ( #22004, #17712 ) ) ;
#4284 = ORIENTED_EDGE ( 'NONE', *, *, #20246, .F. ) ;
#4285 = CARTESIAN_POINT ( 'NONE',  ( 12.55910585664917711, 0.7408941433508786645, -1.155557966632341512E-29 ) ) ;
#4286 = FACE_OUTER_BOUND ( 'NONE', #6788, .T. ) ;
#4287 = ORIENTED_EDGE ( 'NONE', *, *, #6451, .T. ) ;
#4288 = CARTESIAN_POINT ( 'NONE',  ( -46.00000000000000000, 0.000000000000000000, 78.00000000000001421 ) ) ;
#4289 = CYLINDRICAL_SURFACE ( 'NONE', #23423, 13.99999999999999822 ) ;
#4290 = DIRECTION ( 'NONE',  ( 0.000000000000000000, 1.000000000000000000, 0.000000000000000000 ) ) ;
#4291 = VECTOR ( 'NONE', #23376, 1000.000000000000000 ) ;
#4292 = CARTESIAN_POINT ( 'NONE',  ( -34.50075263804418313, -115.9929510916434481, 12.66759465831979981 ) ) ;
#4293 = AXIS2_PLACEMENT_3D ( 'NONE', #21671, #10888, #910 ) ;
#4294 = DIRECTION ( 'NONE',  ( 0.000000000000000000, 0.000000000000000000, 1.000000000000000000 ) ) ;
#4295 = DIRECTION ( 'NONE',  ( -1.000000000000000000, 0.000000000000000000, 0.000000000000000000 ) ) ;
#4296 = CARTESIAN_POINT ( 'NONE',  ( -34.50000000000000000, -115.9382890315277308, 10.02636389016632812 ) ) ;
#4297 = DIRECTION ( 'NONE',  ( 0.000000000000000000, 1.000000000000000000, 0.000000000000000000 ) ) ;
#4298 = LINE ( 'NONE', #1764, #28211 ) ;
#4299 = CARTESIAN_POINT ( 'NONE',  ( 7.999999999999992895, -13.56094713063606072, 50.20060470671736397 ) ) ;
#4300 = FACE_OUTER_BOUND ( 'NONE', #28429, .T. ) ;
#4301 = CARTESIAN_POINT ( 'NONE',  ( 0.000000000000000000, 14.87816164169115218, 4.342730381189920941 ) ) ;
#4302 = DIRECTION ( 'NONE',  ( 0.000000000000000000, 0.000000000000000000, -1.000000000000000000 ) ) ;
#4303 = VERTEX_POINT ( 'NONE', #16299 ) ;
#4304 = CARTESIAN_POINT ( 'NONE',  ( -39.97545270896702618, -115.3019030900506152, 6.152725545821551734 ) ) ;
#4305 = CARTESIAN_POINT ( 'NONE',  ( 8.000000000000000000, -12.46108038583301436, -15.64357617739007722 ) ) ;
#4306 = CARTESIAN_POINT ( 'NONE',  ( -35.50000000000000000, -113.0140978167138712, -0.6247823525988807081 ) ) ;
#4307 = EDGE_CURVE ( 'NONE', #403, #27203, #31234, .T. ) ;
#4308 = ORIENTED_EDGE ( 'NONE', *, *, #9532, .T. ) ;
#4309 = ORIENTED_EDGE ( 'NONE', *, *, #34176, .F. ) ;
#4310 = EDGE_CURVE ( 'NONE', #5141, #28364, #11449, .T. ) ;
#4311 = CARTESIAN_POINT ( 'NONE',  ( 3.799999999999999822, 4.653657836759942730E-16, -49.10000000000000142 ) ) ;
#4312 = CARTESIAN_POINT ( 'NONE',  ( 1.110223024625156540E-13, -1.000000000000042633, -44.50000000000000000 ) ) ;
#4313 = ORIENTED_EDGE ( 'NONE', *, *, #19839, .F. ) ;
#4314 = ORIENTED_EDGE ( 'NONE', *, *, #836, .F. ) ;
#4315 = VERTEX_POINT ( 'NONE', #113 ) ;
#4316 = TOROIDAL_SURFACE ( 'NONE', #841, 4.499999999999990230, 3.000000000000000000 ) ;
#4317 = DIRECTION ( 'NONE',  ( -0.000000000000000000, 0.000000000000000000, -1.000000000000000000 ) ) ;
#4318 = AXIS2_PLACEMENT_3D ( 'NONE', #3952, #23002, #17414 ) ;
#4319 = CARTESIAN_POINT ( 'NONE',  ( -39.02454729103295961, -113.2308352781851397, 4.840225545821550845 ) ) ;
#4320 = DIRECTION ( 'NONE',  ( 1.000000000000000000, 0.000000000000000000, 0.000000000000000000 ) ) ;
#4321 = VECTOR ( 'NONE', #17740, 1000.000000000000000 ) ;
#4322 = DIRECTION ( 'NONE',  ( -1.000000000000000000, 0.000000000000000000, 0.000000000000000000 ) ) ;
#4323 = ORIENTED_EDGE ( 'NONE', *, *, #1614, .F. ) ;
#4324 = ORIENTED_EDGE ( 'NONE', *, *, #33937, .T. ) ;
#4325 = CARTESIAN_POINT ( 'NONE',  ( -35.50000000000000000, -115.0631849411758196, -2.624765990393648885 ) ) ;
#4326 = LINE ( 'NONE', #26281, #28940 ) ;
#4327 = DIRECTION ( 'NONE',  ( -1.000000000000000000, 0.000000000000000000, 0.000000000000000000 ) ) ;
#4328 = VERTEX_POINT ( 'NONE', #33408 ) ;
#4329 = DIRECTION ( 'NONE',  ( -1.174092375852890457E-15, 4.222049128630259891E-16, 1.000000000000000000 ) ) ;
#4330 = VECTOR ( 'NONE', #33498, 1000.000000000000000 ) ;
#4331 = CARTESIAN_POINT ( 'NONE',  ( -34.50000000000000000, -114.9929510916434339, 11.91443571948719971 ) ) ;
#4332 = DIRECTION ( 'NONE',  ( 1.000000000000000000, 0.000000000000000000, 0.000000000000000000 ) ) ;
#4333 = CARTESIAN_POINT ( 'NONE',  ( -36.06250000000002132, -114.9929510916434339, 13.11852480586264669 ) ) ;
#4334 = CARTESIAN_POINT ( 'NONE',  ( 7.999999999999992895, 14.30000000000000071, -3.000000000000002665 ) ) ;
#4335 = CARTESIAN_POINT ( 'NONE',  ( -36.03906250000000000, -113.9929510916434339, 14.11852480586265024 ) ) ;
#4336 = CARTESIAN_POINT ( 'NONE',  ( -34.49999999999998579, -21.76666049839546346, 85.70096189432329936 ) ) ;
#4337 = CARTESIAN_POINT ( 'NONE',  ( -37.99599240977853754, -114.9929510916434339, 12.68378527132499478 ) ) ;
#4338 = LINE ( 'NONE', #20860, #21638 ) ;
#4339 = VERTEX_POINT ( 'NONE', #30370 ) ;
#4341 = CLOSED_SHELL ( 'NONE', ( #15947, #18099, #19316, #32509, #18270, #5524, #23984, #12345, #27807, #24043, #7928, #975, #16730, #24465, #13654, #21232, #1164, #30955, #2434, #8183, #31657, #7895, #33089, #511, #18722, #25890, #18884, #7023, #24106, #20664, #10368, #24900, #12930, #30914, #21392, #35532, #9898, #1569, #1883, #17817, #474, #22257, #31944, #27045, #33202, #27359, #2226, #32157, #10560, #32236, #9717, #3995, #24227, #9692, #13176, #8376, #1531, #12770, #35487, #19836, #6253, #21481, #27394, #2930, #8670, #3081, #8395, #10188, #7862, #19008, #15984, #28928, #21626, #2649, #24284, #26014, #31120, #8427, #20430, #29278, #25812, #22253, #32809, #8602, #20944, #13496, #27582, #25983, #16183, #27694, #33548, #20396, #30886 ) ) ;
#4340 = LINE ( 'NONE', #21048, #3198 ) ;
#4342 = DIRECTION ( 'NONE',  ( 0.000000000000000000, 0.000000000000000000, -1.000000000000000000 ) ) ;
#4343 = CIRCLE ( 'NONE', #29053, 4.000000000000000000 ) ;
#4344 = EDGE_LOOP ( 'NONE', ( #19756, #2369 ) ) ;
#4345 = CARTESIAN_POINT ( 'NONE',  ( -35.50640865667918433, -114.9929510916434339, 12.69998175888958514 ) ) ;
#4346 = VERTEX_POINT ( 'NONE', #30189 ) ;
#4347 = DIRECTION ( 'NONE',  ( 0.000000000000000000, 1.000000000000000000, 0.000000000000000000 ) ) ;
#4348 = ORIENTED_EDGE ( 'NONE', *, *, #33937, .F. ) ;
#4349 = FACE_OUTER_BOUND ( 'NONE', #14294, .T. ) ;
#4350 = VERTEX_POINT ( 'NONE', #17008 ) ;
#4351 = AXIS2_PLACEMENT_3D ( 'NONE', #9477, #20433, #21120 ) ;
#4352 = EDGE_CURVE ( 'NONE', #18803, #19338, #3365, .T. ) ;
#4353 = CARTESIAN_POINT ( 'NONE',  ( -34.50000000000000000, -113.0140978167137860, -0.6247823525984055326 ) ) ;
#4354 = FACE_OUTER_BOUND ( 'NONE', #29347, .T. ) ;
#4355 = CARTESIAN_POINT ( 'NONE',  ( -37.76916472181487450, -111.9754527089670404, 7.034774454178450931 ) ) ;
#4356 = ORIENTED_EDGE ( 'NONE', *, *, #18073, .F. ) ;
#4357 = CARTESIAN_POINT ( 'NONE',  ( -37.88768952767750164, -115.9754527089670262, 7.972274454178450043 ) ) ;
#4358 = CARTESIAN_POINT ( 'NONE',  ( -34.49999999999998579, -14.67619866229204284, 93.25874355921412473 ) ) ;
#4359 = CARTESIAN_POINT ( 'NONE',  ( -35.50000000000000711, -116.0060826362711595, -0.7553032835231661135 ) ) ;
#4360 = ORIENTED_EDGE ( 'NONE', *, *, #22271, .F. ) ;
#4361 = EDGE_LOOP ( 'NONE', ( #2387, #8402, #29708, #703 ) ) ;
#4362 = DIRECTION ( 'NONE',  ( -0.000000000000000000, 0.000000000000000000, -1.000000000000000000 ) ) ;
#4363 = EDGE_CURVE ( 'NONE', #26963, #32273, #24953, .T. ) ;
#4364 = FILL_AREA_STYLE_COLOUR ( '', #22512 ) ;
#4365 = DIRECTION ( 'NONE',  ( 0.000000000000000000, -6.938893903907226011E-15, 1.000000000000000000 ) ) ;
#4366 = ORIENTED_EDGE ( 'NONE', *, *, #16719, .F. ) ;
#4367 = VERTEX_POINT ( 'NONE', #16660 ) ;
#4368 = CARTESIAN_POINT ( 'NONE',  ( -34.50000000000000000, -112.9611193698460738, 2.883091707513499635 ) ) ;
#4369 = CARTESIAN_POINT ( 'NONE',  ( -35.50000000000000711, -112.0154707866092707, 0.9357013553229778235 ) ) ;
#4370 = PRODUCT_DEFINITION_SHAPE ( 'NONE', 'NONE',  #32378 ) ;
#4371 = AXIS2_PLACEMENT_3D ( 'NONE', #3331, #5492, #19669 ) ;
#4372 = CARTESIAN_POINT ( 'NONE',  ( -34.49999999999998579, -29.98076211353323473, 86.49999999999990052 ) ) ;
#4373 = ORIENTED_EDGE ( 'NONE', *, *, #3621, .T. ) ;
#4374 = ORIENTED_EDGE ( 'NONE', *, *, #18934, .F. ) ;
#4375 = CYLINDRICAL_SURFACE ( 'NONE', #15466, 47.49900000000001654 ) ;
#4376 = CIRCLE ( 'NONE', #3800, 52.00000000000000711 ) ;
#4377 = AXIS2_PLACEMENT_3D ( 'NONE', #21496, #27112, #35390 ) ;
#4378 = CARTESIAN_POINT ( 'NONE',  ( -34.50000000000000000, -113.9929510916433344, 10.50625754673586876 ) ) ;
#4379 = DIRECTION ( 'NONE',  ( -1.000000000000000000, 0.000000000000000000, 0.000000000000000000 ) ) ;
#4380 = CARTESIAN_POINT ( 'NONE',  ( -35.50000000000000000, -113.9929510916434339, 12.59652202191340464 ) ) ;
#4381 = CARTESIAN_POINT ( 'NONE',  ( -35.50000000000000000, -115.7766462221073454, 9.569741527169023598 ) ) ;
#4382 = DIRECTION ( 'NONE',  ( 0.000000000000000000, 0.000000000000000000, 1.000000000000000000 ) ) ;
#4383 = DIRECTION ( 'NONE',  ( 0.000000000000000000, 0.000000000000000000, -1.000000000000000000 ) ) ;
#4384 = VERTEX_POINT ( 'NONE', #3010 ) ;
#4385 = CARTESIAN_POINT ( 'NONE',  ( 8.000000000000000000, 0.000000000000000000, 0.000000000000000000 ) ) ;
#4386 = DIRECTION ( 'NONE',  ( 0.1305261922200496583, 0.9914448613738107152, -1.707538432754661574E-31 ) ) ;
#4387 = CARTESIAN_POINT ( 'NONE',  ( 7.999999999999992895, -22.43957647427188817, 41.27978878573619426 ) ) ;
#4388 = ORIENTED_EDGE ( 'NONE', *, *, #1064, .T. ) ;
#4389 = CARTESIAN_POINT ( 'NONE',  ( 0.000000000000000000, 0.000000000000000000, -40.89999999999999858 ) ) ;
#4390 = EDGE_CURVE ( 'NONE', #6784, #32201, #24383, .T. ) ;
#4391 = VECTOR ( 'NONE', #18228, 1000.000000000000000 ) ;
#4392 = CARTESIAN_POINT ( 'NONE',  ( -35.50000000000000711, -114.9724313160460696, -1.624792769101446765 ) ) ;
#4393 = PLANE ( 'NONE',  #10413 ) ;
#4394 = ADVANCED_FACE ( 'NONE', ( #34306 ), #14849, .T. ) ;
#4395 = ITEM_DEFINED_TRANSFORMATION ( 'NONE', 'NONE', #10418,  #21307 ) ;
#4396 = CARTESIAN_POINT ( 'NONE',  ( -35.50000000000000711, -114.0650276068786582, 9.507762098804159123 ) ) ;
#4397 = CYLINDRICAL_SURFACE ( 'NONE', #5550, 3.800000000000018918 ) ;
#4398 = AXIS2_PLACEMENT_3D ( 'NONE', #32622, #21272, #34800 ) ;
#4399 = AXIS2_PLACEMENT_3D ( 'NONE', #6904, #20573, #29240 ) ;
#4400 = EDGE_LOOP ( 'NONE', ( #17520, #32699, #15268, #30435 ) ) ;
#4401 = CIRCLE ( 'NONE', #28517, 7.020000000000045759 ) ;
#4402 = CARTESIAN_POINT ( 'NONE',  ( 0.000000000000000000, 0.000000000000000000, 0.000000000000000000 ) ) ;
#4403 = CARTESIAN_POINT ( 'NONE',  ( -34.50000000000000000, -116.9119893297194324, -1.269118781492768688 ) ) ;
#4404 = DIRECTION ( 'NONE',  ( -1.000000000000000000, 5.339440136655836216E-16, 0.000000000000000000 ) ) ;
#4405 = VERTEX_POINT ( 'NONE', #23306 ) ;
#4406 = ORIENTED_EDGE ( 'NONE', *, *, #25529, .F. ) ;
#4407 = CARTESIAN_POINT ( 'NONE',  ( -36.94073759706866156, -113.0000000000000000, 4.128524454178449155 ) ) ;
#4408 = ADVANCED_FACE ( 'NONE', ( #20596 ), #14482, .T. ) ;
#4409 = VECTOR ( 'NONE', #35396, 1000.000000000000000 ) ;
#4410 =( NAMED_UNIT ( * ) PLANE_ANGLE_UNIT ( ) SI_UNIT ( $, .RADIAN. ) );
#4411 = AXIS2_PLACEMENT_3D ( 'NONE', #1407, #23541, #9853 ) ;
#4412 = ORIENTED_EDGE ( 'NONE', *, *, #11688, .F. ) ;
#4413 = ORIENTED_EDGE ( 'NONE', *, *, #14504, .T. ) ;
#4414 = CARTESIAN_POINT ( 'NONE',  ( -35.50000000000000000, -115.0140978167138712, -0.1247823525984438492 ) ) ;
#4415 =( REPRESENTATION_RELATIONSHIP ('NONE','NONE', #26607, #11863 ) REPRESENTATION_RELATIONSHIP_WITH_TRANSFORMATION ( #436 )SHAPE_REPRESENTATION_RELATIONSHIP( ) );
#4416 = CARTESIAN_POINT ( 'NONE',  ( 0.000000000000000000, 0.000000000000000000, 17.49900000000000233 ) ) ;
#4417 = CARTESIAN_POINT ( 'NONE',  ( 0.000000000000000000, 24.47917365149946534, 45.87777302070943364 ) ) ;
#4418 = AXIS2_PLACEMENT_3D ( 'NONE', #18704, #32403, #15636 ) ;
#4419 = CARTESIAN_POINT ( 'NONE',  ( -35.50000000000000711, -114.9929510916434339, 10.59426868253284226 ) ) ;
#4420 = CARTESIAN_POINT ( 'NONE',  ( -34.49999999999998579, -25.98076211353322051, 84.99999999999992895 ) ) ;
#4421 = EDGE_CURVE ( 'NONE', #31693, #27894, #26683, .T. ) ;
#4422 = AXIS2_PLACEMENT_3D ( 'NONE', #15775, #15426, #18667 ) ;
#4423 = CARTESIAN_POINT ( 'NONE',  ( -36.06250000000002132, -114.9929510916434339, 14.11852480586264846 ) ) ;
#4424 = CARTESIAN_POINT ( 'NONE',  ( -43.99999999999999289, -19.99999999999999645, 0.000000000000000000 ) ) ;
#4425 = AXIS2_PLACEMENT_3D ( 'NONE', #22957, #33955, #814 ) ;
#4426 = LINE ( 'NONE', #23492, #3698 ) ;
#4427 = ORIENTED_EDGE ( 'NONE', *, *, #32912, .T. ) ;
#4428 = CARTESIAN_POINT ( 'NONE',  ( -35.95915003344518368, -115.9929510916434481, 13.11692036158763308 ) ) ;
#4429 = CARTESIAN_POINT ( 'NONE',  ( -35.50000000000000711, -116.0140978167138712, 0.0002176474015577116276 ) ) ;
#4430 =( LENGTH_UNIT ( ) NAMED_UNIT ( * ) SI_UNIT ( .MILLI., .METRE. ) );
#4431 = CIRCLE ( 'NONE', #11305, 3.799999999999999822 ) ;
#4432 = LINE ( 'NONE', #29444, #18787 ) ;
#4433 = CARTESIAN_POINT ( 'NONE',  ( -4.872650870659766653, 0.4273491293403325897, -5.720942237434546063E-15 ) ) ;
#4434 = AXIS2_PLACEMENT_3D ( 'NONE', #13073, #9996, #26752 ) ;
#4435 = VERTEX_POINT ( 'NONE', #26025 ) ;
#4436 = LINE ( 'NONE', #15194, #23992 ) ;
#4437 = CARTESIAN_POINT ( 'NONE',  ( 0.000000000000000000, 0.000000000000000000, 0.000000000000000000 ) ) ;
#4438 = EDGE_CURVE ( 'NONE', #4619, #31088, #17539, .T. ) ;
#4439 = LINE ( 'NONE', #10182, #11323 ) ;
#4440 = CARTESIAN_POINT ( 'NONE',  ( 0.000000000000000000, 0.000000000000000000, -40.00000000000000000 ) ) ;
#4441 = ORIENTED_EDGE ( 'NONE', *, *, #30217, .T. ) ;
#4442 = EDGE_CURVE ( 'NONE', #8092, #24798, #3707, .T. ) ;
#4443 = EDGE_CURVE ( 'NONE', #13336, #3876, #31242, .T. ) ;
#4444 = CARTESIAN_POINT ( 'NONE',  ( -36.02454729103298092, -114.4734759653044307, 3.097274454178448710 ) ) ;
#4445 = DIRECTION ( 'NONE',  ( 0.000000000000000000, 0.9980267284282717810, -0.06279051952930989056 ) ) ;
#4446 = LINE ( 'NONE', #34143, #26809 ) ;
#4447 = VERTEX_POINT ( 'NONE', #9636 ) ;
#4448 = ORIENTED_EDGE ( 'NONE', *, *, #18732, .F. ) ;
#4449 =( NAMED_UNIT ( * ) PLANE_ANGLE_UNIT ( ) SI_UNIT ( $, .RADIAN. ) );
#4450 = AXIS2_PLACEMENT_3D ( 'NONE', #5826, #33365, #30668 ) ;
#4451 = CARTESIAN_POINT ( 'NONE',  ( -35.00000000000000000, -114.0000000000000853, 2.000000000000001776 ) ) ;
#4452 = ORIENTED_EDGE ( 'NONE', *, *, #1176, .F. ) ;
#4453 = CARTESIAN_POINT ( 'NONE',  ( -40.02454729103296671, -112.8166217158120332, 6.340225545821551734 ) ) ;
#4454 = EDGE_CURVE ( 'NONE', #5280, #20493, #26103, .T. ) ;
#4455 = ORIENTED_EDGE ( 'NONE', *, *, #26584, .F. ) ;
#4456 = VECTOR ( 'NONE', #24225, 1000.000000000000000 ) ;
#4457 = ADVANCED_FACE ( 'NONE', ( #19876 ), #28545, .T. ) ;
#4458 = SURFACE_STYLE_FILL_AREA ( #34511 ) ;
#4459 = EDGE_LOOP ( 'NONE', ( #1431, #12773, #21732, #14037 ) ) ;
#4460 = VECTOR ( 'NONE', #33523, 1000.000000000000000 ) ;
#4461 = LINE ( 'NONE', #31619, #1073 ) ;
#4462 = CARTESIAN_POINT ( 'NONE',  ( 7.999999999999992895, 41.20225022064671805, -23.63323037071357646 ) ) ;
#4463 = AXIS2_PLACEMENT_3D ( 'NONE', #16099, #32498, #26948 ) ;
#4464 = VECTOR ( 'NONE', #21064, 1000.000000000000000 ) ;
#4465 = DIRECTION ( 'NONE',  ( 0.000000000000000000, 0.000000000000000000, -1.000000000000000000 ) ) ;
#4466 = ORIENTED_EDGE ( 'NONE', *, *, #8995, .T. ) ;
#4467 = ORIENTED_EDGE ( 'NONE', *, *, #14824, .F. ) ;
#4468 = CARTESIAN_POINT ( 'NONE',  ( -34.49999999999998579, -23.14406523420388950, 95.58669687932936654 ) ) ;
#4469 = FACE_OUTER_BOUND ( 'NONE', #35133, .T. ) ;
#4470 = ORIENTED_EDGE ( 'NONE', *, *, #20316, .T. ) ;
#4471 = CYLINDRICAL_SURFACE ( 'NONE', #34358, 19.99999999999999645 ) ;
#4472 = ADVANCED_FACE ( 'NONE', ( #809 ), #3893, .T. ) ;
#4473 = CIRCLE ( 'NONE', #32060, 4.800000000000006040 ) ;
#4474 = FACE_OUTER_BOUND ( 'NONE', #13684, .T. ) ;
#4475 = DIRECTION ( 'NONE',  ( 0.000000000000000000, 0.000000000000000000, -1.000000000000000000 ) ) ;
#4476 = CARTESIAN_POINT ( 'NONE',  ( -35.24442919769867899, -115.9929510916434481, 13.92914543265605509 ) ) ;
#4477 = VECTOR ( 'NONE', #3136, 1000.000000000000000 ) ;
#4478 = EDGE_CURVE ( 'NONE', #21589, #22983, #28898, .T. ) ;
#4479 = CARTESIAN_POINT ( 'NONE',  ( 0.000000000000000000, -2.710505431213761085E-17, 30.00000000000000000 ) ) ;
#4480 = CARTESIAN_POINT ( 'NONE',  ( -35.54388159064475872, -112.6276912846090568, 7.316024454178449155 ) ) ;
#4481 = EDGE_CURVE ( 'NONE', #32097, #28443, #9447, .T. ) ;
#4482 = CARTESIAN_POINT ( 'NONE',  ( -34.50000000000000000, -115.9920935318519923, 10.44577481630138749 ) ) ;
#4483 = CARTESIAN_POINT ( 'NONE',  ( 0.000000000000000000, 0.000000000000000000, 0.000000000000000000 ) ) ;
#4484 = CIRCLE ( 'NONE', #7339, 17.49900000000001299 ) ;
#4485 = AXIS2_PLACEMENT_3D ( 'NONE', #29986, #5324, #24932 ) ;
#4486 = DIRECTION ( 'NONE',  ( 0.000000000000000000, 1.000000000000000000, 3.491564676272318479E-15 ) ) ;
#4487 = VECTOR ( 'NONE', #23615, 1000.000000000000227 ) ;
#4488 = DIRECTION ( 'NONE',  ( -1.000000000000000000, 0.000000000000000000, 0.000000000000000000 ) ) ;
#4489 = DIRECTION ( 'NONE',  ( 0.000000000000000000, 0.000000000000000000, 1.000000000000000000 ) ) ;
#4490 = LINE ( 'NONE', #26618, #18172 ) ;
#4491 = DIRECTION ( 'NONE',  ( 1.000000000000000000, -0.000000000000000000, -0.000000000000000000 ) ) ;
#4492 = ORIENTED_EDGE ( 'NONE', *, *, #35130, .F. ) ;
#4493 = ADVANCED_FACE ( 'NONE', ( #22587 ), #25673, .F. ) ;
#4494 = CARTESIAN_POINT ( 'NONE',  ( -37.88768952767750875, -112.0245472910329880, 5.027725545821550845 ) ) ;
#4495 = ADVANCED_FACE ( 'NONE', ( #22770 ), #33771, .T. ) ;
#4496 = CIRCLE ( 'NONE', #3890, 14.00000000000000000 ) ;
#4497 = DIRECTION ( 'NONE',  ( -1.000000000000000000, 0.000000000000000000, 0.000000000000000000 ) ) ;
#4498 = CARTESIAN_POINT ( 'NONE',  ( -35.50000000000000000, -113.0140978167138712, -0.6247823525983134951 ) ) ;
#4499 = ORIENTED_EDGE ( 'NONE', *, *, #12958, .F. ) ;
#4500 = ORIENTED_EDGE ( 'NONE', *, *, #35245, .F. ) ;
#4501 = CARTESIAN_POINT ( 'NONE',  ( 0.000000000000000000, 0.000000000000000000, 55.00000000000000000 ) ) ;
#4502 = DIRECTION ( 'NONE',  ( -1.000000000000000000, 0.000000000000000000, 0.000000000000000000 ) ) ;
#4503 = ORIENTED_EDGE ( 'NONE', *, *, #17218, .F. ) ;
#4504 = ORIENTED_EDGE ( 'NONE', *, *, #33430, .T. ) ;
#4505 = VERTEX_POINT ( 'NONE', #9099 ) ;
#4506 = EDGE_CURVE ( 'NONE', #26981, #19156, #33949, .T. ) ;
#4507 = AXIS2_PLACEMENT_3D ( 'NONE', #25820, #11753, #28152 ) ;
#4508 = AXIS2_PLACEMENT_3D ( 'NONE', #30974, #17275, #12610 ) ;
#4509 = CYLINDRICAL_SURFACE ( 'NONE', #26341, 20.00000000000000355 ) ;
#4510 = CARTESIAN_POINT ( 'NONE',  ( -37.49999999999999289, -9.059673409587521320, 113.4689433211306095 ) ) ;
#4511 = CIRCLE ( 'NONE', #25777, 2.447112362156710574 ) ;
#4512 = AXIS2_PLACEMENT_3D ( 'NONE', #6289, #4141, #26095 ) ;
#4513 = DIRECTION ( 'NONE',  ( 0.000000000000000000, 0.000000000000000000, -1.000000000000000000 ) ) ;
#4514 = CARTESIAN_POINT ( 'NONE',  ( -9.999999999999994671, 0.000000000000000000, 0.000000000000000000 ) ) ;
#4515 = ORIENTED_EDGE ( 'NONE', *, *, #1138, .F. ) ;
#4516 = ORIENTED_EDGE ( 'NONE', *, *, #10844, .T. ) ;
#4517 = CARTESIAN_POINT ( 'NONE',  ( -35.50000000000000711, -112.0140978167138712, 0.0002176474015661141945 ) ) ;
#4518 = DIRECTION ( 'NONE',  ( -1.000000000000000000, 0.000000000000000000, 0.000000000000000000 ) ) ;
#4519 = DIRECTION ( 'NONE',  ( 1.000000000000000000, -0.000000000000000000, -0.000000000000000000 ) ) ;
#4520 = VERTEX_POINT ( 'NONE', #4079 ) ;
#4521 = STYLED_ITEM ( 'NONE', ( #15434 ), #33750 ) ;
#4522 = CARTESIAN_POINT ( 'NONE',  ( -38.00000000000000711, -114.9929510916434339, 11.91443571948719615 ) ) ;
#4523 = EDGE_CURVE ( 'NONE', #33987, #15078, #15021, .T. ) ;
#4524 = PLANE ( 'NONE',  #35139 ) ;
#4525 = EDGE_CURVE ( 'NONE', #10473, #7400, #27265, .T. ) ;
#4526 = CARTESIAN_POINT ( 'NONE',  ( -34.50075263804418313, -114.9929510916434339, 12.66759465831979981 ) ) ;
#4527 = DIRECTION ( 'NONE',  ( 0.000000000000000000, 0.000000000000000000, -1.000000000000000000 ) ) ;
#4528 = CARTESIAN_POINT ( 'NONE',  ( -36.07812499999994316, -114.9929510916434339, 13.11852480586264669 ) ) ;
#4529 = FACE_OUTER_BOUND ( 'NONE', #30724, .T. ) ;
#4530 = CARTESIAN_POINT ( 'NONE',  ( -34.50000000000000000, -114.9925223117477202, 10.47601618151863079 ) ) ;
#4531 = FACE_OUTER_BOUND ( 'NONE', #15351, .T. ) ;
#4532 = CARTESIAN_POINT ( 'NONE',  ( -37.97447287825094975, -114.9929510916434339, 12.77960891308616809 ) ) ;
#4533 = CYLINDRICAL_SURFACE ( 'NONE', #25429, 47.49900000000001654 ) ;
#4534 = VERTEX_POINT ( 'NONE', #7632 ) ;
#4535 = CARTESIAN_POINT ( 'NONE',  ( 50.00000000000000000, 20.00000000000001776, -25.00000000000000000 ) ) ;
#4536 = DIRECTION ( 'NONE',  ( 0.000000000000000000, 0.000000000000000000, 1.000000000000000000 ) ) ;
#4537 = VERTEX_POINT ( 'NONE', #2271 ) ;
#4538 = CARTESIAN_POINT ( 'NONE',  ( -36.06250000000002132, -114.9929510916434339, 13.11852480586264669 ) ) ;
#4539 = VERTEX_POINT ( 'NONE', #32307 ) ;
#4540 = EDGE_CURVE ( 'NONE', #4447, #27214, #6528, .T. ) ;
#4541 = CARTESIAN_POINT ( 'NONE',  ( -37.88768952767750164, -115.9754527089670262, 3.472274454178448266 ) ) ;
#4542 = AXIS2_PLACEMENT_3D ( 'NONE', #24522, #16204, #26878 ) ;
#4543 = DIRECTION ( 'NONE',  ( 0.000000000000000000, 0.5000000000000011102, -0.8660254037844379305 ) ) ;
#4544 = ORIENTED_EDGE ( 'NONE', *, *, #13246, .F. ) ;
#4545 = DIRECTION ( 'NONE',  ( -1.000000000000000000, -0.000000000000000000, -0.000000000000000000 ) ) ;
#4546 = EDGE_LOOP ( 'NONE', ( #17373, #23327 ) ) ;
#4547 = SHAPE_REPRESENTATION ( 'handle', ( #21307 ), #23057 ) ;
#4548 = CARTESIAN_POINT ( 'NONE',  ( -34.50000000000000000, -113.0140978167138712, -0.4997823525984338988 ) ) ;
#4549 = DIRECTION ( 'NONE',  ( -1.783119874454246424E-31, -1.187911941725854497E-31, 1.000000000000000000 ) ) ;
#4550 = CARTESIAN_POINT ( 'NONE',  ( 0.2142857142857085284, -10.49781318335649161, -1.200000000000006617 ) ) ;
#4551 = ORIENTED_EDGE ( 'NONE', *, *, #22256, .T. ) ;
#4552 = CARTESIAN_POINT ( 'NONE',  ( -35.02454729103298803, -114.8876895276775087, 7.597274454178450931 ) ) ;
#4553 = DIRECTION ( 'NONE',  ( 0.000000000000000000, 0.000000000000000000, -1.000000000000000000 ) ) ;
#4554 = DIRECTION ( 'NONE',  ( 1.000000000000000000, 0.000000000000000000, 0.000000000000000000 ) ) ;
#4555 = ORIENTED_EDGE ( 'NONE', *, *, #29947, .F. ) ;
#4556 = EDGE_LOOP ( 'NONE', ( #9217, #22059, #5444, #24711 ) ) ;
#4557 = DIRECTION ( 'NONE',  ( 0.000000000000000000, 0.5877852522924742473, -0.8090169943749466741 ) ) ;
#4558 = PRESENTATION_STYLE_ASSIGNMENT (( #26863 ) ) ;
#4559 = FACE_OUTER_BOUND ( 'NONE', #9559, .T. ) ;
#4560 = EDGE_LOOP ( 'NONE', ( #10454, #30109, #25468, #18298 ) ) ;
#4561 = ORIENTED_EDGE ( 'NONE', *, *, #2926, .F. ) ;
#4562 = CARTESIAN_POINT ( 'NONE',  ( -34.50000000000000000, -115.5178116849130276, -1.498529437126731034 ) ) ;
#4563 = AXIS2_PLACEMENT_3D ( 'NONE', #17575, #15052, #6787 ) ;
#4564 = CYLINDRICAL_SURFACE ( 'NONE', #31139, 47.49900000000001654 ) ;
#4565 = ORIENTED_EDGE ( 'NONE', *, *, #18024, .T. ) ;
#4566 = ORIENTED_EDGE ( 'NONE', *, *, #20245, .F. ) ;
#4567 = CARTESIAN_POINT ( 'NONE',  ( -34.49999999999998579, -39.98076211353324538, 86.49999999999991473 ) ) ;
#4568 = EDGE_CURVE ( 'NONE', #18652, #34234, #31770, .T. ) ;
#4569 = CARTESIAN_POINT ( 'NONE',  ( -34.50000000000000000, -113.9929510916434623, 10.50625754673586876 ) ) ;
#4570 = CYLINDRICAL_SURFACE ( 'NONE', #32914, 52.00000000000000711 ) ;
#4571 = CARTESIAN_POINT ( 'NONE',  ( -38.00000000000000711, -113.9929510916434339, 10.85830208992306822 ) ) ;
#4572 = CARTESIAN_POINT ( 'NONE',  ( -36.03125000000003553, -115.9929510916434481, 13.11852480586264846 ) ) ;
#4573 = DIRECTION ( 'NONE',  ( 1.000000000000000000, 1.734723475976807094E-16, 0.000000000000000000 ) ) ;
#4574 = DIRECTION ( 'NONE',  ( 1.000000000000000000, 0.000000000000000000, 0.000000000000000000 ) ) ;
#4575 = ORIENTED_EDGE ( 'NONE', *, *, #21635, .T. ) ;
#4576 = CARTESIAN_POINT ( 'NONE',  ( 0.000000000000000000, -50.95304419620832448, 10.38206564895643957 ) ) ;
#4577 = CARTESIAN_POINT ( 'NONE',  ( 0.000000000000000000, 3.872983346207420574, -1.000000000000000888 ) ) ;
#4578 = LINE ( 'NONE', #1682, #13404 ) ;
#4579 = VERTEX_POINT ( 'NONE', #35205 ) ;
#4580 = DIRECTION ( 'NONE',  ( 0.000000000000000000, 0.000000000000000000, -1.000000000000000000 ) ) ;
#4581 = CARTESIAN_POINT ( 'NONE',  ( -35.50000000000000711, -112.0140978167138712, -0.3747823525984256832 ) ) ;
#4582 = FACE_OUTER_BOUND ( 'NONE', #13992, .T. ) ;
#4583 = CIRCLE ( 'NONE', #1687, 8.000000000000007105 ) ;
#4584 = LINE ( 'NONE', #9783, #27949 ) ;
#4585 = DIRECTION ( 'NONE',  ( -1.000000000000000000, 0.000000000000000000, 0.000000000000000000 ) ) ;
#4586 = ORIENTED_EDGE ( 'NONE', *, *, #11027, .T. ) ;
#4587 = CIRCLE ( 'NONE', #24693, 3.999999999999996447 ) ;
#4588 = DIRECTION ( 'NONE',  ( 1.836970198721029934E-16, -1.000000000000000000, 0.000000000000000000 ) ) ;
#4589 = CARTESIAN_POINT ( 'NONE',  ( -34.50000000000000000, -111.4147656069378058, -1.853877267569947529 ) ) ;
#4590 = CARTESIAN_POINT ( 'NONE',  ( -3.799999999999999822, 0.000000000000000000, -49.10000000000000142 ) ) ;
#4591 = ORIENTED_EDGE ( 'NONE', *, *, #12276, .T. ) ;
#4592 = ORIENTED_EDGE ( 'NONE', *, *, #3389, .T. ) ;
#4593 = CARTESIAN_POINT ( 'NONE',  ( -37.05926240293133134, -115.0000000000000000, 3.378524454178448710 ) ) ;
#4594 = AXIS2_PLACEMENT_3D ( 'NONE', #2321, #12751, #21197 ) ;
#4595 = VECTOR ( 'NONE', #4519, 1000.000000000000000 ) ;
#4596 = DIRECTION ( 'NONE',  ( -1.000000000000000000, 0.000000000000000000, 0.000000000000000000 ) ) ;
#4597 = ORIENTED_EDGE ( 'NONE', *, *, #7502, .T. ) ;
#4598 = EDGE_LOOP ( 'NONE', ( #18366, #4470 ) ) ;
#4599 = CARTESIAN_POINT ( 'NONE',  ( -35.50000000000000000, -115.0140978167138712, -0.3122823525984416149 ) ) ;
#4600 = LINE ( 'NONE', #20394, #2257 ) ;
#4601 = DIRECTION ( 'NONE',  ( -1.000000000000000000, 0.000000000000000000, 0.000000000000000000 ) ) ;
#4602 = EDGE_CURVE ( 'NONE', #21628, #15307, #10523, .T. ) ;
#4603 = CARTESIAN_POINT ( 'NONE',  ( -35.50000000000000000, -113.9465028010160381, 10.50071319044726081 ) ) ;
#4604 = DIRECTION ( 'NONE',  ( 1.000000000000000000, 1.734723475976807094E-16, 0.000000000000000000 ) ) ;
#4605 = EDGE_CURVE ( 'NONE', #16930, #3480, #31848, .T. ) ;
#4606 = CARTESIAN_POINT ( 'NONE',  ( -35.61121590948313553, -114.9929510916434339, 14.07058620477040733 ) ) ;
#4607 = CARTESIAN_POINT ( 'NONE',  ( 4.000000000000003553, 49.25004636492388954, 16.68630974939777545 ) ) ;
#4608 = AXIS2_PLACEMENT_3D ( 'NONE', #11139, #16868, #25182 ) ;
#4609 = CARTESIAN_POINT ( 'NONE',  ( 7.999999999999992895, 0.000000000000000000, 0.000000000000000000 ) ) ;
#4610 = VERTEX_POINT ( 'NONE', #7810 ) ;
#4611 = EDGE_CURVE ( 'NONE', #23058, #16592, #11143, .T. ) ;
#4612 = CIRCLE ( 'NONE', #17808, 52.00000000000000711 ) ;
#4613 = PRODUCT_DEFINITION_FORMATION_WITH_SPECIFIED_SOURCE ( 'ANY', '', #8910, .NOT_KNOWN. ) ;
#4614 = CARTESIAN_POINT ( 'NONE',  ( -35.52552712174883709, -115.9929510916434481, 12.77960891308624625 ) ) ;
#4615 = CARTESIAN_POINT ( 'NONE',  ( -35.50000000000000711, -112.8511839106603247, -1.611965039240275122 ) ) ;
#4616 = CARTESIAN_POINT ( 'NONE',  ( -49.99999999999998579, -64.99999999999997158, -25.00000000000000000 ) ) ;
#4617 = DIRECTION ( 'NONE',  ( -0.000000000000000000, 0.8191520442889889120, 0.5735764363510502672 ) ) ;
#4618 = CARTESIAN_POINT ( 'NONE',  ( 7.999999999999992895, -30.93515269692138503, 36.04401931830242489 ) ) ;
#4619 = VERTEX_POINT ( 'NONE', #7103 ) ;
#4620 = LINE ( 'NONE', #1910, #35481 ) ;
#4621 = CARTESIAN_POINT ( 'NONE',  ( 38.00000000000000000, 10.58300524425836642, 3.000000000000002665 ) ) ;
#4622 = FACE_OUTER_BOUND ( 'NONE', #29568, .T. ) ;
#4623 = FACE_OUTER_BOUND ( 'NONE', #25068, .T. ) ;
#4624 = ORIENTED_EDGE ( 'NONE', *, *, #31983, .T. ) ;
#4625 = CARTESIAN_POINT ( 'NONE',  ( -36.33479806579561000, -114.7490116281687165, 6.191024454178448266 ) ) ;
#4626 = DIRECTION ( 'NONE',  ( 0.000000000000000000, 0.000000000000000000, -1.000000000000000000 ) ) ;
#4627 = CARTESIAN_POINT ( 'NONE',  ( -50.00000000000000000, 19.99999999999998934, 120.0000000000000000 ) ) ;
#4628 = VERTEX_POINT ( 'NONE', #26379 ) ;
#4629 = ORIENTED_EDGE ( 'NONE', *, *, #21374, .F. ) ;
#4630 =( NAMED_UNIT ( * ) PLANE_ANGLE_UNIT ( ) SI_UNIT ( $, .RADIAN. ) );
#4631 = CARTESIAN_POINT ( 'NONE',  ( -21.15833593587365513, -38.85511776651532756, 79.29903810567645905 ) ) ;
#4632 = ORIENTED_EDGE ( 'NONE', *, *, #7310, .T. ) ;
#4633 = CARTESIAN_POINT ( 'NONE',  ( -34.83677480945821259, -116.0794154965774965, 8.683975545821549957 ) ) ;
#4634 = EDGE_LOOP ( 'NONE', ( #29738, #4894, #23434, #33229 ) ) ;
#4635 = EDGE_CURVE ( 'NONE', #20295, #16000, #13237, .T. ) ;
#4636 = DIRECTION ( 'NONE',  ( 1.000000000000000000, 0.000000000000000000, -1.691777834109591064E-31 ) ) ;
#4637 = VERTEX_POINT ( 'NONE', #29264 ) ;
#4638 = VECTOR ( 'NONE', #16706, 1000.000000000000000 ) ;
#4639 = ORIENTED_EDGE ( 'NONE', *, *, #5293, .T. ) ;
#4640 = CARTESIAN_POINT ( 'NONE',  ( 5.400000000000015454, -1.000000000000002220, -30.00000000000000000 ) ) ;
#4641 = VECTOR ( 'NONE', #20780, 1000.000000000000000 ) ;
#4642 = CIRCLE ( 'NONE', #10388, 3.799999999999999822 ) ;
#4643 = VECTOR ( 'NONE', #14961, 1000.000000000000000 ) ;
#4644 = FACE_OUTER_BOUND ( 'NONE', #7398, .T. ) ;
#4645 = ORIENTED_EDGE ( 'NONE', *, *, #28476, .T. ) ;
#4646 = EDGE_LOOP ( 'NONE', ( #12462, #23064 ) ) ;
#4647 = EDGE_CURVE ( 'NONE', #21593, #18755, #15721, .T. ) ;
#4648 = DIRECTION ( 'NONE',  ( 0.000000000000000000, 0.000000000000000000, 1.000000000000000000 ) ) ;
#4649 = DIRECTION ( 'NONE',  ( 0.000000000000000000, 0.000000000000000000, 1.000000000000000000 ) ) ;
#4650 = ADVANCED_FACE ( 'NONE', ( #9987 ), #26929, .T. ) ;
#4651 = EDGE_CURVE ( 'NONE', #1430, #25395, #20770, .T. ) ;
#4652 = ORIENTED_EDGE ( 'NONE', *, *, #24673, .F. ) ;
#4653 = DIRECTION ( 'NONE',  ( 0.000000000000000000, 0.5735764363510502672, -0.8191520442889889120 ) ) ;
#4654 = CYLINDRICAL_SURFACE ( 'NONE', #28619, 20.00000000000000711 ) ;
#4655 = CARTESIAN_POINT ( 'NONE',  ( 4.000000000000000000, 4.898587196589412829E-16, 55.00000000000000000 ) ) ;
#4656 = CARTESIAN_POINT ( 'NONE',  ( -36.00976557831293690, -115.9929510916434481, 14.11852773550420359 ) ) ;
#4657 = CARTESIAN_POINT ( 'NONE',  ( -42.49999999999999289, -30.19486372867095980, 84.29903810567654432 ) ) ;
#4658 = CARTESIAN_POINT ( 'NONE',  ( -36.23083527818513261, -116.0245472910329880, 7.784774454178449155 ) ) ;
#4659 = EDGE_CURVE ( 'NONE', #13726, #9927, #4426, .T. ) ;
#4660 = CARTESIAN_POINT ( 'NONE',  ( -34.50000000000000000, -115.1342778146718473, 8.846135899190283425 ) ) ;
#4661 = DIRECTION ( 'NONE',  ( 1.000000000000000000, 1.836970198721029934E-16, 0.000000000000000000 ) ) ;
#4662 = ADVANCED_FACE ( 'NONE', ( #21138 ), #12698, .T. ) ;
#4663 = FACE_OUTER_BOUND ( 'NONE', #2305, .T. ) ;
#4664 = DIRECTION ( 'NONE',  ( 0.000000000000000000, 0.5877852522924686962, 0.8090169943749506709 ) ) ;
#4665 = LINE ( 'NONE', #7681, #18087 ) ;
#4666 = CARTESIAN_POINT ( 'NONE',  ( 0.000000000000000000, 0.000000000000000000, -40.89999999999999858 ) ) ;
#4667 = CARTESIAN_POINT ( 'NONE',  ( 7.999999999999992895, 0.000000000000000000, 0.000000000000000000 ) ) ;
#4668 = EDGE_LOOP ( 'NONE', ( #21258, #7130, #25073, #22230 ) ) ;
#4669 = MECHANICAL_DESIGN_GEOMETRIC_PRESENTATION_REPRESENTATION (  '', ( #24779 ), #25931 ) ;
#4670 = CARTESIAN_POINT ( 'NONE',  ( -35.00000000000000000, -113.9407375970686900, 2.496475545821551290 ) ) ;
#4671 = VECTOR ( 'NONE', #3833, 1000.000000000000000 ) ;
#4672 = DIRECTION ( 'NONE',  ( 0.000000000000000000, 0.000000000000000000, 1.000000000000000000 ) ) ;
#4673 = CARTESIAN_POINT ( 'NONE',  ( -35.50000000000000000, -113.9344536409997630, 0.9850770315317123327 ) ) ;
#4674 = EDGE_LOOP ( 'NONE', ( #27595, #20983, #3661, #23050 ) ) ;
#4675 = ORIENTED_EDGE ( 'NONE', *, *, #7522, .T. ) ;
#4676 = LINE ( 'NONE', #4311, #13705 ) ;
#4677 = DIRECTION ( 'NONE',  ( 0.000000000000000000, 0.000000000000000000, 1.000000000000000000 ) ) ;
#4678 = VERTEX_POINT ( 'NONE', #32477 ) ;
#4679 = ORIENTED_EDGE ( 'NONE', *, *, #33002, .F. ) ;
#4680 = ORIENTED_EDGE ( 'NONE', *, *, #24046, .T. ) ;
#4681 = EDGE_CURVE ( 'NONE', #9312, #20546, #15186, .T. ) ;
#4682 = DIRECTION ( 'NONE',  ( 0.000000000000000000, 0.000000000000000000, 1.000000000000000000 ) ) ;
#4683 = CARTESIAN_POINT ( 'NONE',  ( -29.99999999999999645, -26.99999999999999645, 113.9999999999999858 ) ) ;
#4684 = DIRECTION ( 'NONE',  ( 0.000000000000000000, -0.002057130845644464939, -0.9999978841041035071 ) ) ;
#4685 = CARTESIAN_POINT ( 'NONE',  ( 7.999999999999992895, -27.43636312076347394, 38.14186064215141414 ) ) ;
#4686 = ORIENTED_EDGE ( 'NONE', *, *, #31450, .T. ) ;
#4687 = ORIENTED_EDGE ( 'NONE', *, *, #9702, .F. ) ;
#4688 = CARTESIAN_POINT ( 'NONE',  ( -35.50000000000000711, -112.0157046079661995, -0.6902086197697556713 ) ) ;
#4689 = ADVANCED_FACE ( 'NONE', ( #34665 ), #15546, .T. ) ;
#4690 = DIRECTION ( 'NONE',  ( -1.783119874454246424E-31, -1.187911941725854497E-31, 1.000000000000000000 ) ) ;
#4691 = EDGE_CURVE ( 'NONE', #9, #23286, #20311, .T. ) ;
#4692 = ADVANCED_FACE ( 'NONE', ( #1902 ), #12877, .T. ) ;
#4693 = CYLINDRICAL_SURFACE ( 'NONE', #5183, 4.000000000000003553 ) ;
#4694 = VECTOR ( 'NONE', #4549, 1000.000000000000000 ) ;
#4695 = MECHANICAL_DESIGN_GEOMETRIC_PRESENTATION_REPRESENTATION (  '', ( #10435 ), #28238 ) ;
#4696 = ORIENTED_EDGE ( 'NONE', *, *, #12263, .T. ) ;
#4697 = CARTESIAN_POINT ( 'NONE',  ( 8.000000000000007105, 3.753907720749127819, 8.725776631572756514 ) ) ;
#4698 = CARTESIAN_POINT ( 'NONE',  ( -34.50000000000000000, -113.0106174888879877, 1.881901162060937827 ) ) ;
#4699 = CARTESIAN_POINT ( 'NONE',  ( -34.50000000000000000, -114.1861579685891712, 9.524983039397698192 ) ) ;
#4700 = DIRECTION ( 'NONE',  ( 1.000000000000000000, -5.339440136655842133E-16, -1.047965281155519420E-16 ) ) ;
#4701 = CARTESIAN_POINT ( 'NONE',  ( -35.83891589277640577, -114.9929510916434339, 13.09299768411358222 ) ) ;
#4702 = DIRECTION ( 'NONE',  ( 0.000000000000000000, 0.000000000000000000, 1.000000000000000000 ) ) ;
#4703 = CARTESIAN_POINT ( 'NONE',  ( -39.00000000000000000, -113.9929510916434339, 12.50851088611646311 ) ) ;
#4704 = DIRECTION ( 'NONE',  ( -1.734723475976807094E-16, 0.8660254037844385966, 0.5000000000000001110 ) ) ;
#4705 = ADVANCED_FACE ( 'NONE', ( #21853 ), #8338, .T. ) ;
#4706 = CARTESIAN_POINT ( 'NONE',  ( -37.54084996655477369, -114.9929510916434339, 13.11692036158760466 ) ) ;
#4707 = CARTESIAN_POINT ( 'NONE',  ( -1.398397006337051440, -6.091550361990532458, 0.000000000000000000 ) ) ;
#4708 = VERTEX_POINT ( 'NONE', #13579 ) ;
#4709 = DIRECTION ( 'NONE',  ( -1.000000000000000000, 0.000000000000000000, 0.000000000000000000 ) ) ;
#4710 = DIRECTION ( 'NONE',  ( -1.000000000000000000, 0.000000000000000000, 0.000000000000000000 ) ) ;
#4711 = ORIENTED_EDGE ( 'NONE', *, *, #22449, .T. ) ;
#4712 = CARTESIAN_POINT ( 'NONE',  ( -37.99899697755054717, -114.9929510916434339, 12.65121853911336736 ) ) ;
#4713 = VERTEX_POINT ( 'NONE', #18977 ) ;
#4714 = CARTESIAN_POINT ( 'NONE',  ( -36.94073759706868287, -112.0000000000000142, 7.128524454178449155 ) ) ;
#4715 = CYLINDRICAL_SURFACE ( 'NONE', #23752, 7.199999999999994849 ) ;
#4716 = ORIENTED_EDGE ( 'NONE', *, *, #13607, .T. ) ;
#4717 = ORIENTED_EDGE ( 'NONE', *, *, #22497, .T. ) ;
#4718 = FACE_BOUND ( 'NONE', #4546, .T. ) ;
#4719 = AXIS2_PLACEMENT_3D ( 'NONE', #33993, #1223, #25359 ) ;
#4720 = ORIENTED_EDGE ( 'NONE', *, *, #6449, .T. ) ;
#4721 = AXIS2_PLACEMENT_3D ( 'NONE', #25348, #5898, #22098 ) ;
#4722 = CARTESIAN_POINT ( 'NONE',  ( -36.11231047232249125, -112.0245472910329880, 8.722274454178448266 ) ) ;
#4723 = EDGE_CURVE ( 'NONE', #6235, #33126, #5973, .T. ) ;
#4724 = EDGE_CURVE ( 'NONE', #9813, #32383, #35320, .T. ) ;
#4725 = DIRECTION ( 'NONE',  ( 0.000000000000000000, 0.000000000000000000, 1.000000000000000000 ) ) ;
#4726 = DIRECTION ( 'NONE',  ( 0.000000000000000000, 0.5000000000000062172, -0.8660254037844351549 ) ) ;
#4727 = ORIENTED_EDGE ( 'NONE', *, *, #4150, .F. ) ;
#4729 = ORIENTED_EDGE ( 'NONE', *, *, #30126, .T. ) ;
#4728 = EDGE_CURVE ( 'NONE', #31732, #32324, #24572, .T. ) ;
#4730 = CARTESIAN_POINT ( 'NONE',  ( 70.00000600000001327, -25.98076211353320986, 88.99999999999994316 ) ) ;
#4731 = LINE ( 'NONE', #5081, #19576 ) ;
#4732 = ORIENTED_EDGE ( 'NONE', *, *, #32747, .T. ) ;
#4733 = ORIENTED_EDGE ( 'NONE', *, *, #2523, .F. ) ;
#4734 = CIRCLE ( 'NONE', #19090, 0.7500000000000039968 ) ;
#4735 = CARTESIAN_POINT ( 'NONE',  ( -34.50000000000000000, -111.0397324434303101, -0.9506101647064429949 ) ) ;
#4736 = ADVANCED_FACE ( 'NONE', ( #22032, #11708 ), #14405, .F. ) ;
#4737 = DIRECTION ( 'NONE',  ( 0.000000000000000000, 0.000000000000000000, -1.000000000000000000 ) ) ;
#4738 = ORIENTED_EDGE ( 'NONE', *, *, #29385, .T. ) ;
#4739 = ORIENTED_EDGE ( 'NONE', *, *, #20853, .T. ) ;
#4740 = ADVANCED_FACE ( 'NONE', ( #22679 ), #3454, .T. ) ;
#4741 = CARTESIAN_POINT ( 'NONE',  ( -35.50000000000000711, -114.3464919575557843, 9.568884482464163455 ) ) ;
#4742 = CARTESIAN_POINT ( 'NONE',  ( -38.00000000000000711, -113.9929510916434339, 12.60752341388803721 ) ) ;
#4743 = DIRECTION ( 'NONE',  ( 0.000000000000000000, 0.000000000000000000, 1.000000000000000000 ) ) ;
#4744 = CARTESIAN_POINT ( 'NONE',  ( 0.000000000000000000, 0.000000000000000000, 0.000000000000000000 ) ) ;
#4745 = CARTESIAN_POINT ( 'NONE',  ( -37.99899697755054717, -113.9929510916434339, 12.65121853911336913 ) ) ;
#4746 = CARTESIAN_POINT ( 'NONE',  ( -37.58145695302688694, -115.9929510916434481, 13.11211614918362756 ) ) ;
#4747 = CYLINDRICAL_SURFACE ( 'NONE', #34880, 47.49900000000001654 ) ;
#4748 = LINE ( 'NONE', #12835, #30758 ) ;
#4749 = EDGE_LOOP ( 'NONE', ( #29469, #8930, #24312, #15619 ) ) ;
#4750 = CARTESIAN_POINT ( 'NONE',  ( 0.000000000000000000, 21.80633394113452539, 2.912696353505896063 ) ) ;
#4751 = DIRECTION ( 'NONE',  ( -1.000000000000000000, 0.000000000000000000, 0.000000000000000000 ) ) ;
#4752 = LINE ( 'NONE', #10317, #187 ) ;
#4753 = ORIENTED_EDGE ( 'NONE', *, *, #12466, .F. ) ;
#4754 = CYLINDRICAL_SURFACE ( 'NONE', #29111, 20.00000000000000355 ) ;
#4755 = CARTESIAN_POINT ( 'NONE',  ( -35.50000000000000711, -112.0140900043112282, 0.8439677466545482121 ) ) ;
#4756 = DIRECTION ( 'NONE',  ( 0.000000000000000000, 0.000000000000000000, 1.000000000000000000 ) ) ;
#4757 = CARTESIAN_POINT ( 'NONE',  ( -35.50000000000000711, -114.8211182053456838, 9.932864235516914775 ) ) ;
#4758 = DIRECTION ( 'NONE',  ( -1.000000000000000000, 0.000000000000000000, 0.000000000000000000 ) ) ;
#4759 = ADVANCED_FACE ( 'NONE', ( #35564 ), #16437, .T. ) ;
#4760 = ORIENTED_EDGE ( 'NONE', *, *, #11760, .T. ) ;
#4761 = EDGE_CURVE ( 'NONE', #6860, #26487, #4270, .T. ) ;
#4762 = DIRECTION ( 'NONE',  ( 1.000000000000000000, -5.339440136655842133E-16, -1.047965281155519420E-16 ) ) ;
#4763 = CARTESIAN_POINT ( 'NONE',  ( -35.50000000000000000, -111.0140978167138570, -0.4685323525984296800 ) ) ;
#4764 = DIRECTION ( 'NONE',  ( -1.000000000000000000, 0.000000000000000000, 0.000000000000000000 ) ) ;
#4765 = EDGE_LOOP ( 'NONE', ( #20616, #8302, #6492, #18096 ) ) ;
#4766 = VERTEX_POINT ( 'NONE', #33671 ) ;
#4767 = CARTESIAN_POINT ( 'NONE',  ( -36.64504884055823908, -115.0245472910329880, 7.784774454178449155 ) ) ;
#4768 = VECTOR ( 'NONE', #29640, 1000.000000000000000 ) ;
#4769 = AXIS2_PLACEMENT_3D ( 'NONE', #29069, #23847, #5132 ) ;
#4770 = FACE_OUTER_BOUND ( 'NONE', #28713, .T. ) ;
#4771 = VERTEX_POINT ( 'NONE', #30980 ) ;
#4772 = ORIENTED_EDGE ( 'NONE', *, *, #31314, .F. ) ;
#4773 = CARTESIAN_POINT ( 'NONE',  ( -34.50000000000000000, -113.0349311500474982, -0.6247823525985715110 ) ) ;
#4774 = DIRECTION ( 'NONE',  ( 0.000000000000000000, 0.8660254037844385966, 0.5000000000000001110 ) ) ;
#4775 = LINE ( 'NONE', #29611, #21416 ) ;
#4776 = CARTESIAN_POINT ( 'NONE',  ( -37.62959469683911351, -114.9929510916434339, 13.10254527216511633 ) ) ;
#4777 = CARTESIAN_POINT ( 'NONE',  ( -4.000000000000000000, 0.000000000000000000, -55.89999999999999858 ) ) ;
#4778 = DIRECTION ( 'NONE',  ( -1.000000000000000000, 0.000000000000000000, 0.000000000000000000 ) ) ;
#4779 = CARTESIAN_POINT ( 'NONE',  ( -34.50000000000000000, -112.0141053790792114, 0.9054673897245171243 ) ) ;
#4780 = CARTESIAN_POINT ( 'NONE',  ( -35.87745010033553683, -114.9929510916434339, 14.11371147303761298 ) ) ;
#4781 = CYLINDRICAL_SURFACE ( 'NONE', #203, 20.00000000000000711 ) ;
#4782 = AXIS2_PLACEMENT_3D ( 'NONE', #10707, #19324, #30338 ) ;
#4783 = VECTOR ( 'NONE', #6481, 1000.000000000000000 ) ;
#4784 = DIRECTION ( 'NONE',  ( -1.000000000000000000, -8.673617379884210501E-17, 1.502314598737149170E-16 ) ) ;
#4785 = ORIENTED_EDGE ( 'NONE', *, *, #14974, .F. ) ;
#4786 = CARTESIAN_POINT ( 'NONE',  ( -37.18750000000004974, -115.9929510916434481, 13.11852480586264846 ) ) ;
#4787 = CARTESIAN_POINT ( 'NONE',  ( -35.50000000000000711, -113.6807644833805995, -1.624782352598427959 ) ) ;
#4788 = LINE ( 'NONE', #4616, #35231 ) ;
#4789 = CARTESIAN_POINT ( 'NONE',  ( 3.872983346207429900, -1.000000000000003553, 38.00000000000000711 ) ) ;
#4790 = CARTESIAN_POINT ( 'NONE',  ( 8.000000000000007105, -9.919332006307262972, 5.363026430117087351 ) ) ;
#4791 = ORIENTED_EDGE ( 'NONE', *, *, #33012, .F. ) ;
#4792 = DIRECTION ( 'NONE',  ( 9.178431089824344374E-17, -6.938893903907203726E-17, -1.000000000000000000 ) ) ;
#4793 = DIRECTION ( 'NONE',  ( 0.000000000000000000, -0.3681245526846853022, 0.9297764858882484607 ) ) ;
#4794 = CYLINDRICAL_SURFACE ( 'NONE', #22795, 2.799122904894268071 ) ;
#4795 = LINE ( 'NONE', #15738, #14958 ) ;
#4796 = CARTESIAN_POINT ( 'NONE',  ( -37.47347596530441649, -114.9754527089670262, 3.472274454178448710 ) ) ;
#4797 = CARTESIAN_POINT ( 'NONE',  ( -1.599999999999989875, -4.627228502943551802E-14, 4.980000000000000426 ) ) ;
#4798 = DIRECTION ( 'NONE',  ( 0.000000000000000000, 0.000000000000000000, -1.000000000000000000 ) ) ;
#4799 = EDGE_LOOP ( 'NONE', ( #26119, #27654, #34244, #26720 ) ) ;
#4800 = CIRCLE ( 'NONE', #13425, 8.000000000000001776 ) ;
#4801 = ORIENTED_EDGE ( 'NONE', *, *, #275, .F. ) ;
#4802 = EDGE_CURVE ( 'NONE', #2896, #1026, #27635, .T. ) ;
#4803 = DIRECTION ( 'NONE',  ( -1.000000000000000000, 0.000000000000000000, 0.000000000000000000 ) ) ;
#4804 = DIRECTION ( 'NONE',  ( 0.000000000000000000, 0.000000000000000000, 1.000000000000000000 ) ) ;
#4805 = CARTESIAN_POINT ( 'NONE',  ( 65.00000000000001421, -25.98076211353320986, 84.99999999999994316 ) ) ;
#4806 = VERTEX_POINT ( 'NONE', #14578 ) ;
#4807 = CARTESIAN_POINT ( 'NONE',  ( -36.23083527818512550, -111.9754527089670404, 3.715225545821550845 ) ) ;
#4808 = ORIENTED_EDGE ( 'NONE', *, *, #3131, .T. ) ;
#4809 = ORIENTED_EDGE ( 'NONE', *, *, #18799, .T. ) ;
#4810 = ORIENTED_EDGE ( 'NONE', *, *, #16382, .F. ) ;
#4811 = CYLINDRICAL_SURFACE ( 'NONE', #34415, 8.000000000000000000 ) ;
#4812 = CIRCLE ( 'NONE', #19718, 4.000000000000003553 ) ;
#4813 = CIRCLE ( 'NONE', #27243, 52.00000000000000711 ) ;
#4814 = ADVANCED_FACE ( 'NONE', ( #2805, #25590 ), #16254, .F. ) ;
#4815 = DIRECTION ( 'NONE',  ( 9.178431089824344374E-17, -6.938893903907203726E-17, -1.000000000000000000 ) ) ;
#4816 = ORIENTED_EDGE ( 'NONE', *, *, #1843, .T. ) ;
#4817 = EDGE_LOOP ( 'NONE', ( #23966, #32613, #7392, #28962 ) ) ;
#4818 = DIRECTION ( 'NONE',  ( 0.000000000000000000, 0.000000000000000000, -1.000000000000000000 ) ) ;
#4819 = CARTESIAN_POINT ( 'NONE',  ( 4.000000000000003553, 39.64889472655781333, -33.64468972902464827 ) ) ;
#4820 = ORIENTED_EDGE ( 'NONE', *, *, #27797, .F. ) ;
#4821 = DIRECTION ( 'NONE',  ( -1.783119874454246424E-31, -1.187911941725854497E-31, 1.000000000000000000 ) ) ;
#4822 = AXIS2_PLACEMENT_3D ( 'NONE', #11490, #25363, #14889 ) ;
#4823 = LINE ( 'NONE', #7145, #15357 ) ;
#4824 = LINE ( 'NONE', #23902, #6376 ) ;
#4825 = DIRECTION ( 'NONE',  ( -1.000000000000000000, 0.000000000000000000, 0.000000000000000000 ) ) ;
#4826 = CARTESIAN_POINT ( 'NONE',  ( -35.54388159064475872, -112.6276912846090568, 8.816024454178448266 ) ) ;
#4827 = CARTESIAN_POINT ( 'NONE',  ( -34.49999793727135966, -115.9929510916434481, 12.61164896875036767 ) ) ;
#4828 = CARTESIAN_POINT ( 'NONE',  ( 38.00000000000000000, 6.980486755139912911E-15, 0.000000000000000000 ) ) ;
#4829 = DIRECTION ( 'NONE',  ( -1.000000000000000000, 0.000000000000000000, 0.000000000000000000 ) ) ;
#4830 = CARTESIAN_POINT ( 'NONE',  ( 0.000000000000000000, 0.000000000000000000, 0.000000000000000000 ) ) ;
#4831 = CARTESIAN_POINT ( 'NONE',  ( 7.999999999999992895, 5.667686777401707232, 46.64153600743606631 ) ) ;
#4832 = VECTOR ( 'NONE', #31692, 1000.000000000000000 ) ;
#4833 = DIRECTION ( 'NONE',  ( -1.000000000000000000, -1.734723475976807094E-16, -0.000000000000000000 ) ) ;
#4834 = LINE ( 'NONE', #32009, #33893 ) ;
#4835 = VERTEX_POINT ( 'NONE', #7995 ) ;
#4836 = CARTESIAN_POINT ( 'NONE',  ( -37.76916472181486739, -116.0245472910329880, 5.965225545821550845 ) ) ;
#4837 = CARTESIAN_POINT ( 'NONE',  ( -34.49999999999998579, -22.68172400785649501, 82.28589838486220742 ) ) ;
#4838 = FACE_BOUND ( 'NONE', #2201, .T. ) ;
#4839 = VERTEX_POINT ( 'NONE', #11889 ) ;
#4840 = VERTEX_POINT ( 'NONE', #8167 ) ;
#4841 = EDGE_CURVE ( 'NONE', #29049, #18180, #7708, .T. ) ;
#4842 = FACE_OUTER_BOUND ( 'NONE', #15782, .T. ) ;
#4843 = CARTESIAN_POINT ( 'NONE',  ( 0.000000000000000000, 5.871425383721554425, 51.66745943012285380 ) ) ;
#4844 = ORIENTED_EDGE ( 'NONE', *, *, #15258, .T. ) ;
#4845 = EDGE_CURVE ( 'NONE', #12683, #2615, #22867, .T. ) ;
#4846 = ORIENTED_EDGE ( 'NONE', *, *, #22366, .F. ) ;
#4847 = ORIENTED_EDGE ( 'NONE', *, *, #34173, .F. ) ;
#4848 = DIRECTION ( 'NONE',  ( -1.000000000000000000, -0.000000000000000000, -0.000000000000000000 ) ) ;
#4849 = CARTESIAN_POINT ( 'NONE',  ( -38.97545270896704039, -114.8876895276775087, 9.152725545821553510 ) ) ;
#4850 = EDGE_CURVE ( 'NONE', #13312, #3956, #1400, .T. ) ;
#4851 = CARTESIAN_POINT ( 'NONE',  ( 3.747002708109903324E-15, -26.99999999999998579, 0.000000000000000000 ) ) ;
#4852 = ADVANCED_FACE ( 'NONE', ( #27098, #13408 ), #35376, .T. ) ;
#4853 = LINE ( 'NONE', #12947, #8691 ) ;
#4854 = VERTEX_POINT ( 'NONE', #23771 ) ;
#4855 = ORIENTED_EDGE ( 'NONE', *, *, #9500, .F. ) ;
#4856 = CARTESIAN_POINT ( 'NONE',  ( -35.50000000000000711, -112.0140900043112282, 0.8439677466545482121 ) ) ;
#4857 = AXIS2_PLACEMENT_3D ( 'NONE', #9340, #1419, #20124 ) ;
#4858 = VECTOR ( 'NONE', #24661, 1000.000000000000000 ) ;
#4859 = CARTESIAN_POINT ( 'NONE',  ( 0.000000000000000000, -1.693188892523641798, -15.40623615209873876 ) ) ;
#4860 = DIRECTION ( 'NONE',  ( 1.000000000000000000, 1.734723475976807094E-16, 0.000000000000000000 ) ) ;
#4861 = ORIENTED_EDGE ( 'NONE', *, *, #15180, .T. ) ;
#4862 = DIRECTION ( 'NONE',  ( 0.000000000000000000, 1.067522139062650474E-15, 1.000000000000000000 ) ) ;
#4863 = CARTESIAN_POINT ( 'NONE',  ( -34.50000000000000000, -112.0250551866464548, 1.025914454044489332 ) ) ;
#4864 = CARTESIAN_POINT ( 'NONE',  ( -34.50481333282507279, -114.9929510916434339, 12.74107470552716492 ) ) ;
#4865 = CARTESIAN_POINT ( 'NONE',  ( 46.00000000000000000, 0.000000000000000000, 70.00000000000000000 ) ) ;
#4866 = CARTESIAN_POINT ( 'NONE',  ( -37.99599240977853754, -114.9929510916434339, 12.68378527132499478 ) ) ;
#4867 = LINE ( 'NONE', #26475, #21457 ) ;
#4868 = CARTESIAN_POINT ( 'NONE',  ( -39.00000000000000000, -113.9929510916434339, 10.85830208992306822 ) ) ;
#4869 = DIRECTION ( 'NONE',  ( 0.000000000000000000, 0.9929510916431029122, -0.1185248058626136303 ) ) ;
#4870 = EDGE_CURVE ( 'NONE', #27386, #20308, #12918, .T. ) ;
#4871 = CARTESIAN_POINT ( 'NONE',  ( -38.00000000000000711, -114.9929510916434339, 11.21034663311206181 ) ) ;
#4872 = DIRECTION ( 'NONE',  ( 1.174092375852890260E-15, -4.222049128630259891E-16, -1.000000000000000000 ) ) ;
#4873 = VERTEX_POINT ( 'NONE', #3806 ) ;
#4874 = FACE_OUTER_BOUND ( 'NONE', #4361, .T. ) ;
#4875 = DIRECTION ( 'NONE',  ( 0.000000000000000000, 0.000000000000000000, -1.000000000000000000 ) ) ;
#4876 = ORIENTED_EDGE ( 'NONE', *, *, #17833, .T. ) ;
#4877 = CARTESIAN_POINT ( 'NONE',  ( -37.99599240977853754, -114.9929510916434339, 12.68378527132499478 ) ) ;
#4878 = VERTEX_POINT ( 'NONE', #31685 ) ;
#4879 = CARTESIAN_POINT ( 'NONE',  ( -35.00000000000000000, -114.0592624029313242, 9.003524454178448266 ) ) ;
#4880 = DIRECTION ( 'NONE',  ( 1.000000000000000000, -0.000000000000000000, -0.000000000000000000 ) ) ;
#4881 = VERTEX_POINT ( 'NONE', #17462 ) ;
#4882 = ORIENTED_EDGE ( 'NONE', *, *, #15628, .F. ) ;
#4883 = CIRCLE ( 'NONE', #20959, 4.800000000000002487 ) ;
#4884 = ADVANCED_FACE ( 'NONE', ( #3992, #23044 ), #14763, .F. ) ;
#4885 = AXIS2_PLACEMENT_3D ( 'NONE', #3231, #22470, #8610 ) ;
#4886 = DIRECTION ( 'NONE',  ( -1.000000000000000000, 0.000000000000000000, 0.000000000000000000 ) ) ;
#4887 = ADVANCED_FACE ( 'NONE', ( #12431 ), #9728, .T. ) ;
#4888 = ADVANCED_FACE ( 'NONE', ( #28460 ), #28993, .F. ) ;
#4889 = ORIENTED_EDGE ( 'NONE', *, *, #7647, .T. ) ;
#4890 = CARTESIAN_POINT ( 'NONE',  ( -36.94073759706866156, -111.0000000000000284, 2.628524454178448710 ) ) ;
#4891 = AXIS2_PLACEMENT_3D ( 'NONE', #30428, #19587, #8090 ) ;
#4892 = FACE_OUTER_BOUND ( 'NONE', #15777, .T. ) ;
#4893 = DIRECTION ( 'NONE',  ( 0.000000000000000000, -0.4817536741017035551, -0.8763066800438700232 ) ) ;
#4894 = ORIENTED_EDGE ( 'NONE', *, *, #17863, .T. ) ;
#4895 = ORIENTED_EDGE ( 'NONE', *, *, #1547, .F. ) ;
#4896 = DIRECTION ( 'NONE',  ( 0.000000000000000000, 0.000000000000000000, -1.000000000000000000 ) ) ;
#4897 = EDGE_CURVE ( 'NONE', #28967, #28820, #17816, .T. ) ;
#4898 = SURFACE_SIDE_STYLE ('',( #29384 ) ) ;
#4899 = ADVANCED_FACE ( 'NONE', ( #25945 ), #15288, .T. ) ;
#4900 = DIRECTION ( 'NONE',  ( 0.000000000000000000, 0.000000000000000000, -1.000000000000000000 ) ) ;
#4902 = EDGE_LOOP ( 'NONE', ( #20074, #26565, #28777, #32466 ) ) ;
#4901 = VECTOR ( 'NONE', #24351, 1000.000000000000000 ) ;
#4903 = ORIENTED_EDGE ( 'NONE', *, *, #2228, .F. ) ;
#4904 = CARTESIAN_POINT ( 'NONE',  ( -34.50000000000000000, -111.0140978167138570, 0.0002176474015659786963 ) ) ;
#4905 = CARTESIAN_POINT ( 'NONE',  ( 1.799999999999996048, 0.000000000000000000, 0.000000000000000000 ) ) ;
#4906 = EDGE_LOOP ( 'NONE', ( #19942, #33349, #3240, #23801 ) ) ;
#4907 = CARTESIAN_POINT ( 'NONE',  ( -35.50000000000000711, -114.2305202833893816, 9.534416457224700991 ) ) ;
#4908 = CIRCLE ( 'NONE', #870, 47.49900000000000944 ) ;
#4909 = CARTESIAN_POINT ( 'NONE',  ( -34.50000000000000000, -113.9929510916434339, 10.52000928670414126 ) ) ;
#4910 = AXIS2_PLACEMENT_3D ( 'NONE', #32006, #7345, #24099 ) ;
#4911 = CYLINDRICAL_SURFACE ( 'NONE', #19404, 10.99999999999999289 ) ;
#4912 = DIRECTION ( 'NONE',  ( -1.000000000000000000, -0.000000000000000000, 0.000000000000000000 ) ) ;
#4913 = CARTESIAN_POINT ( 'NONE',  ( -34.50000000000000000, -113.9917898843777522, 10.50611893782865813 ) ) ;
#4914 = EDGE_CURVE ( 'NONE', #33676, #29329, #1449, .T. ) ;
#4915 = AXIS2_PLACEMENT_3D ( 'NONE', #33256, #2495, #19544 ) ;
#4916 = CARTESIAN_POINT ( 'NONE',  ( -37.42187499999996447, -115.9929510916434481, 13.11852480586264846 ) ) ;
#4917 = CYLINDRICAL_SURFACE ( 'NONE', #3830, 52.00000000000000711 ) ;
#4918 = DIRECTION ( 'NONE',  ( -1.000000000000000000, 0.000000000000000000, 0.000000000000000000 ) ) ;
#4919 = EDGE_CURVE ( 'NONE', #9813, #26454, #24409, .T. ) ;
#4920 = ORIENTED_EDGE ( 'NONE', *, *, #2300, .T. ) ;
#4921 = EDGE_CURVE ( 'NONE', #35237, #29395, #12321, .T. ) ;
#4922 = LINE ( 'NONE', #21623, #8484 ) ;
#4923 = CARTESIAN_POINT ( 'NONE',  ( 8.000000000000000000, -9.508666619816503740, -19.83898331853700014 ) ) ;
#4924 = CARTESIAN_POINT ( 'NONE',  ( 0.000000000000000000, 3.384281271887823461, 18.48663108841358138 ) ) ;
#4925 = CIRCLE ( 'NONE', #19833, 4.800000000000000711 ) ;
#4926 = ORIENTED_EDGE ( 'NONE', *, *, #10455, .T. ) ;
#4927 = DIRECTION ( 'NONE',  ( -1.000000000000000000, 0.000000000000000000, -0.000000000000000000 ) ) ;
#4928 = CARTESIAN_POINT ( 'NONE',  ( -35.50000000000000711, -112.0140978167138712, 0.8127176474015721519 ) ) ;
#4929 = FACE_OUTER_BOUND ( 'NONE', #25889, .T. ) ;
#4930 = ADVANCED_FACE ( 'NONE', ( #14936 ), #1817, .F. ) ;
#4931 = EDGE_CURVE ( 'NONE', #10012, #34823, #7149, .T. ) ;
#4932 = CARTESIAN_POINT ( 'NONE',  ( -35.50160444427493189, -114.9929510916434339, 12.65937477241749853 ) ) ;
#4933 = CARTESIAN_POINT ( 'NONE',  ( 0.000000000000000000, 0.2227391519116599106, 46.98410307550729215 ) ) ;
#4934 = EDGE_LOOP ( 'NONE', ( #8011, #7197, #29948, #581 ) ) ;
#4935 = CARTESIAN_POINT ( 'NONE',  ( 4.000000000000000000, -19.77827456857333743, -2.969824084036673639 ) ) ;
#4936 = VECTOR ( 'NONE', #35385, 1000.000000000000000 ) ;
#4937 = CARTESIAN_POINT ( 'NONE',  ( -35.50000000000000000, -113.8474311500459777, -2.624782352598442614 ) ) ;
#4938 = ORIENTED_EDGE ( 'NONE', *, *, #1254, .T. ) ;
#4939 = ORIENTED_EDGE ( 'NONE', *, *, #12357, .F. ) ;
#4940 = CARTESIAN_POINT ( 'NONE',  ( -35.99999999999999289, -114.0592624029313242, 7.503524454178450043 ) ) ;
#4941 = AXIS2_PLACEMENT_3D ( 'NONE', #7301, #29096, #26397 ) ;
#4942 = CARTESIAN_POINT ( 'NONE',  ( -0.6000000000000037526, -12.74999999999999822, -1.200000000000006617 ) ) ;
#4943 = VERTEX_POINT ( 'NONE', #1268 ) ;
#4944 = ORIENTED_EDGE ( 'NONE', *, *, #26740, .F. ) ;
#4945 = CARTESIAN_POINT ( 'NONE',  ( -34.50000000000000000, -114.6807644833805000, -0.6247823525984269599 ) ) ;
#4946 = CARTESIAN_POINT ( 'NONE',  ( 0.000000000000000000, -39.64889472655708857, -33.64468972902551513 ) ) ;
#4947 = DIRECTION ( 'NONE',  ( -1.000000000000000000, 0.000000000000000000, 0.000000000000000000 ) ) ;
#4948 = CARTESIAN_POINT ( 'NONE',  ( -38.00000000000000711, -114.9929510916434339, 12.39849696637031151 ) ) ;
#4949 = CARTESIAN_POINT ( 'NONE',  ( 8.000000000000000000, 17.47118961583601759, -0.9861715913088253682 ) ) ;
#4950 = LINE ( 'NONE', #7806, #33755 ) ;
#4951 = CARTESIAN_POINT ( 'NONE',  ( -34.50000000000000000, -112.0140978167138712, -0.5622823525984296245 ) ) ;
#4952 = EDGE_CURVE ( 'NONE', #9169, #19399, #18177, .T. ) ;
#4953 = DIRECTION ( 'NONE',  ( 0.000000000000000000, 0.000000000000000000, 1.000000000000000000 ) ) ;
#4954 = EDGE_CURVE ( 'NONE', #19206, #12602, #26128, .T. ) ;
#4955 = CIRCLE ( 'NONE', #34296, 4.800000000000003375 ) ;
#4956 = DIRECTION ( 'NONE',  ( -1.000000000000000000, 0.000000000000000000, 0.000000000000000000 ) ) ;
#4957 = EDGE_LOOP ( 'NONE', ( #35361, #31161, #15292, #4277 ) ) ;
#4958 = CARTESIAN_POINT ( 'NONE',  ( -37.48437500000004263, -115.9929510916434481, 13.11852480586264846 ) ) ;
#4959 = LINE ( 'NONE', #33028, #11930 ) ;
#4960 = DIRECTION ( 'NONE',  ( 1.000000000000000000, 0.000000000000000000, 0.000000000000000000 ) ) ;
#4961 = AXIS2_PLACEMENT_3D ( 'NONE', #6185, #14096, #3320 ) ;
#4962 = AXIS2_PLACEMENT_3D ( 'NONE', #17066, #520, #25375 ) ;
#4963 = FACE_BOUND ( 'NONE', #20149, .T. ) ;
#4964 = EDGE_LOOP ( 'NONE', ( #23071, #23246, #173, #15881 ) ) ;
#4965 = DIRECTION ( 'NONE',  ( -1.000000000000000000, -0.000000000000000000, -0.000000000000000000 ) ) ;
#4966 = CYLINDRICAL_SURFACE ( 'NONE', #16975, 4.799999999999998934 ) ;
#4967 = DIRECTION ( 'NONE',  ( -1.000000000000000000, 0.000000000000000000, 0.000000000000000000 ) ) ;
#4968 = CARTESIAN_POINT ( 'NONE',  ( 0.000000000000000000, -2.710505431213761085E-17, 45.00000000000000000 ) ) ;
#4969 = CIRCLE ( 'NONE', #3811, 52.00000000000000711 ) ;
#4970 = DIRECTION ( 'NONE',  ( -1.000000000000000000, 0.000000000000000000, 0.000000000000000000 ) ) ;
#4971 = CARTESIAN_POINT ( 'NONE',  ( -44.00000000000000000, -3.999999999999993339, 0.000000000000000000 ) ) ;
#4972 = ORIENTED_EDGE ( 'NONE', *, *, #4390, .F. ) ;
#4973 = VECTOR ( 'NONE', #9505, 1000.000000000000000 ) ;
#4974 = ORIENTED_EDGE ( 'NONE', *, *, #3829, .F. ) ;
#4975 = CYLINDRICAL_SURFACE ( 'NONE', #4463, 7.199999999999994849 ) ;
#4976 = DIRECTION ( 'NONE',  ( -1.000000000000000000, -0.000000000000000000, -0.000000000000000000 ) ) ;
#4977 = LINE ( 'NONE', #10546, #28900 ) ;
#4978 = VERTEX_POINT ( 'NONE', #31337 ) ;
#4979 = CARTESIAN_POINT ( 'NONE',  ( -37.76916472181486739, -116.0245472910329880, 4.465225545821550845 ) ) ;
#4980 = ORIENTED_EDGE ( 'NONE', *, *, #11686, .F. ) ;
#4981 = ORIENTED_EDGE ( 'NONE', *, *, #13607, .F. ) ;
#4982 = ORIENTED_EDGE ( 'NONE', *, *, #18025, .F. ) ;
#4983 = DIRECTION ( 'NONE',  ( -1.000000000000000000, 0.000000000000000000, 0.000000000000000000 ) ) ;
#4984 = CIRCLE ( 'NONE', #8967, 20.00000000000000711 ) ;
#4985 = CIRCLE ( 'NONE', #9573, 10.00000000000000000 ) ;
#4986 = CARTESIAN_POINT ( 'NONE',  ( 5.400000000000015454, -1.000000000000002220, -22.00000000000000000 ) ) ;
#4987 = ORIENTED_EDGE ( 'NONE', *, *, #32459, .F. ) ;
#4988 = ORIENTED_EDGE ( 'NONE', *, *, #7057, .T. ) ;
#4989 = AXIS2_PLACEMENT_3D ( 'NONE', #610, #19337, #11244 ) ;
#4990 = CARTESIAN_POINT ( 'NONE',  ( 7.999999999999992895, -51.85248208264516023, -3.914090171286743747 ) ) ;
#4991 = LINE ( 'NONE', #4819, #34483 ) ;
#4992 = CARTESIAN_POINT ( 'NONE',  ( 0.000000000000000000, -3.968388925834960723, 21.63912866391138934 ) ) ;
#4993 = AXIS2_PLACEMENT_3D ( 'NONE', #10499, #34818, #15704 ) ;
#4994 = VECTOR ( 'NONE', #20065, 1000.000000000000000 ) ;
#4995 = FACE_OUTER_BOUND ( 'NONE', #23443, .T. ) ;
#4996 = DIRECTION ( 'NONE',  ( 0.000000000000000000, 0.000000000000000000, 1.000000000000000000 ) ) ;
#4997 = EDGE_CURVE ( 'NONE', #15078, #352, #9436, .T. ) ;
#4998 = CARTESIAN_POINT ( 'NONE',  ( 0.000000000000000000, 9.637487275701349887, -10.15474465512039615 ) ) ;
#4999 = CARTESIAN_POINT ( 'NONE',  ( -38.97545270896704039, -113.1123104723225055, 6.847274454178450043 ) ) ;
#5000 = CARTESIAN_POINT ( 'NONE',  ( -34.50000000000000000, -115.9929510916434481, 12.56351784598954424 ) ) ;
#5001 = DIRECTION ( 'NONE',  ( 1.734723475976807341E-16, -1.000000000000000000, 0.000000000000000000 ) ) ;
#5002 = AXIS2_PLACEMENT_3D ( 'NONE', #29082, #1539, #9453 ) ;
#5003 = CARTESIAN_POINT ( 'NONE',  ( -46.00000000000000000, 1.347111479062088405E-15, -11.00000000000000000 ) ) ;
#5004 = AXIS2_PLACEMENT_3D ( 'NONE', #22998, #3580, #14527 ) ;
#5005 = DIRECTION ( 'NONE',  ( 0.000000000000000000, 0.000000000000000000, 1.000000000000000000 ) ) ;
#5006 = DIRECTION ( 'NONE',  ( 1.000000000000000000, 0.000000000000000000, 0.000000000000000000 ) ) ;
#5007 = CIRCLE ( 'NONE', #10193, 6.000000000000005329 ) ;
#5008 = LINE ( 'NONE', #32362, #33147 ) ;
#5009 = CYLINDRICAL_SURFACE ( 'NONE', #5208, 47.49900000000001654 ) ;
#5010 = ORIENTED_EDGE ( 'NONE', *, *, #16114, .F. ) ;
#5011 = EDGE_CURVE ( 'NONE', #13957, #10771, #1976, .T. ) ;
#5012 = CARTESIAN_POINT ( 'NONE',  ( -36.94073759706868287, -116.9999999999999858, 8.871475545821548181 ) ) ;
#5013 = PRESENTATION_LAYER_ASSIGNMENT (  '', '', ( #20502 ) ) ;
#5014 = CYLINDRICAL_SURFACE ( 'NONE', #7766, 52.00000000000000711 ) ;
#5015 = CIRCLE ( 'NONE', #9027, 4.000000000000006217 ) ;
#5016 = DIRECTION ( 'NONE',  ( -1.000000000000000000, 0.000000000000000000, 0.000000000000000000 ) ) ;
#5017 = ORIENTED_EDGE ( 'NONE', *, *, #2507, .F. ) ;
#5018 = ORIENTED_EDGE ( 'NONE', *, *, #22614, .F. ) ;
#5019 = CIRCLE ( 'NONE', #967, 47.49900000000001654 ) ;
#5020 = DIRECTION ( 'NONE',  ( 0.000000000000000000, -0.8660254037844433705, 0.4999999999999918954 ) ) ;
#5021 = DIRECTION ( 'NONE',  ( -1.000000000000000000, 0.000000000000000000, 0.000000000000000000 ) ) ;
#5022 = ORIENTED_EDGE ( 'NONE', *, *, #31954, .T. ) ;
#5023 = CIRCLE ( 'NONE', #22240, 47.49900000000001654 ) ;
#5024 = CIRCLE ( 'NONE', #6720, 6.765000000000044977 ) ;
#5025 = ORIENTED_EDGE ( 'NONE', *, *, #12344, .T. ) ;
#5026 = DIRECTION ( 'NONE',  ( 0.000000000000000000, 0.8090169943749448977, 0.5877852522924766898 ) ) ;
#5027 = DIRECTION ( 'NONE',  ( -1.000000000000000000, 0.000000000000000000, 0.000000000000000000 ) ) ;
#5028 = CARTESIAN_POINT ( 'NONE',  ( 46.00000000000000711, -25.98076211353322051, 84.99999999999997158 ) ) ;
#5029 = CARTESIAN_POINT ( 'NONE',  ( -55.00000000000000000, 10.00000000000000888, 120.0000000000000000 ) ) ;
#5030 = CIRCLE ( 'NONE', #26307, 3.799999999999999822 ) ;
#5031 = EDGE_LOOP ( 'NONE', ( #18459, #29819, #13472, #32503 ) ) ;
#5032 = ORIENTED_EDGE ( 'NONE', *, *, #26877, .F. ) ;
#5033 = CARTESIAN_POINT ( 'NONE',  ( -35.50000000000000711, -112.0154707866092707, 0.9357013553229778235 ) ) ;
#5034 = VECTOR ( 'NONE', #33715, 1000.000000000000000 ) ;
#5035 = LINE ( 'NONE', #35454, #33534 ) ;
#5036 = DIRECTION ( 'NONE',  ( 0.000000000000000000, 0.000000000000000000, 1.000000000000000000 ) ) ;
#5037 = ORIENTED_EDGE ( 'NONE', *, *, #17189, .F. ) ;
#5038 = DIRECTION ( 'NONE',  ( 1.000000000000000000, -0.000000000000000000, -0.000000000000000000 ) ) ;
#5039 = CIRCLE ( 'NONE', #9624, 4.000000000000003553 ) ;
#5040 = AXIS2_PLACEMENT_3D ( 'NONE', #7405, #16016, #4893 ) ;
#5041 = CARTESIAN_POINT ( 'NONE',  ( -34.50000000000000000, -115.8878449012421754, -1.128496220799388494 ) ) ;
#5042 = CIRCLE ( 'NONE', #7343, 52.00000000000000711 ) ;
#5043 = APPLICATION_CONTEXT ( 'automotive_design' ) ;
#5044 = EDGE_CURVE ( 'NONE', #11158, #11697, #2193, .T. ) ;
#5045 = CARTESIAN_POINT ( 'NONE',  ( -34.50000000000000000, -114.3464919575557843, 9.568884482464163455 ) ) ;
#5046 = EDGE_CURVE ( 'NONE', #3725, #12104, #29542, .T. ) ;
#5047 = CIRCLE ( 'NONE', #25165, 10.49999999999999645 ) ;
#5048 = CYLINDRICAL_SURFACE ( 'NONE', #15382, 22.00000000000000000 ) ;
#5049 = CARTESIAN_POINT ( 'NONE',  ( -35.50000000000000000, -113.9883062625807071, 10.50570311110699961 ) ) ;
#5050 = DIRECTION ( 'NONE',  ( 0.000000000000000000, -0.8660254037844327124, -0.5000000000000102141 ) ) ;
#5051 = CARTESIAN_POINT ( 'NONE',  ( -34.50000000000000000, -114.9492820284331742, 10.20776876943783940 ) ) ;
#5052 = CYLINDRICAL_SURFACE ( 'NONE', #6116, 52.00000000000000711 ) ;
#5053 = CARTESIAN_POINT ( 'NONE',  ( -37.99839555572501837, -114.9929510916434339, 12.65937477241748965 ) ) ;
#5054 = CYLINDRICAL_SURFACE ( 'NONE', #35202, 15.49899999999998457 ) ;
#5055 = ORIENTED_EDGE ( 'NONE', *, *, #16264, .F. ) ;
#5056 = DIRECTION ( 'NONE',  ( 0.000000000000000000, -0.2486898871648416942, -0.9685831611286345177 ) ) ;
#5057 = DIRECTION ( 'NONE',  ( 0.000000000000000000, 0.000000000000000000, 1.000000000000000000 ) ) ;
#5058 = ORIENTED_EDGE ( 'NONE', *, *, #34445, .T. ) ;
#5059 = CARTESIAN_POINT ( 'NONE',  ( -38.00000000000000711, -114.9929510916434339, 12.50851088611646311 ) ) ;
#5060 = ORIENTED_EDGE ( 'NONE', *, *, #2411, .F. ) ;
#5061 = ADVANCED_FACE ( 'NONE', ( #10622 ), #9182, .T. ) ;
#5062 = CARTESIAN_POINT ( 'NONE',  ( -35.02454729103298803, -114.8876895276775087, 6.097274454178449155 ) ) ;
#5063 = CARTESIAN_POINT ( 'NONE',  ( 8.000000000000000000, -4.460989585141086344, 16.92083251265324151 ) ) ;
#5064 = CIRCLE ( 'NONE', #15951, 7.020000000000045759 ) ;
#5065 = VERTEX_POINT ( 'NONE', #21578 ) ;
#5066 = ORIENTED_EDGE ( 'NONE', *, *, #8119, .T. ) ;
#5067 = AXIS2_PLACEMENT_3D ( 'NONE', #21520, #32886, #27669 ) ;
#5068 = CARTESIAN_POINT ( 'NONE',  ( 8.000000000000007105, 9.919332006307387317, -5.363026430117004750 ) ) ;
#5069 = DIRECTION ( 'NONE',  ( -1.000000000000000000, 0.000000000000000000, 0.000000000000000000 ) ) ;
#5070 = EDGE_LOOP ( 'NONE', ( #12284, #35440, #2417, #18326 ) ) ;
#5071 = CARTESIAN_POINT ( 'NONE',  ( -40.02454729103296671, -115.1833782841879525, 5.159774454178449155 ) ) ;
#5072 = AXIS2_PLACEMENT_3D ( 'NONE', #13308, #4848, #4682 ) ;
#5073 = AXIS2_PLACEMENT_3D ( 'NONE', #8061, #3209, #14170 ) ;
#5074 = CARTESIAN_POINT ( 'NONE',  ( 4.000000000000000000, 0.5097555531873367851, 19.99350267651958291 ) ) ;
#5075 = CARTESIAN_POINT ( 'NONE',  ( 65.00000000000001421, -30.47068043442695284, 93.33026027086508236 ) ) ;
#5076 = VERTEX_POINT ( 'NONE', #32578 ) ;
#5077 = ORIENTED_EDGE ( 'NONE', *, *, #6885, .T. ) ;
#5078 = CARTESIAN_POINT ( 'NONE',  ( 70.00001200000002655, -22.78209474394049039, 87.45818687989959983 ) ) ;
#5079 = CIRCLE ( 'NONE', #6215, 4.000000000000000000 ) ;
#5080 = EDGE_CURVE ( 'NONE', #16643, #30312, #18538, .T. ) ;
#5081 = CARTESIAN_POINT ( 'NONE',  ( 7.999999999999992895, 24.72041153920734047, 40.55929306992698002 ) ) ;
#5082 = ORIENTED_EDGE ( 'NONE', *, *, #9526, .F. ) ;
#5083 = EDGE_LOOP ( 'NONE', ( #7070, #31003, #30832, #16173 ) ) ;
#5084 = CARTESIAN_POINT ( 'NONE',  ( -34.50000000000000000, -111.0278007905855588, 1.116632271043183078 ) ) ;
#5085 = DIRECTION ( 'NONE',  ( -1.000000000000000000, -1.836970198721029934E-16, -0.000000000000000000 ) ) ;
#5086 = ORIENTED_EDGE ( 'NONE', *, *, #7009, .T. ) ;
#5087 = DIRECTION ( 'NONE',  ( -1.783119874454246424E-31, -1.187911941725854497E-31, 1.000000000000000000 ) ) ;
#5088 = EDGE_CURVE ( 'NONE', #15252, #22087, #16332, .T. ) ;
#5089 = CARTESIAN_POINT ( 'NONE',  ( -34.50000000000000000, -113.9929510916434339, 10.50625754673588474 ) ) ;
#5090 = EDGE_CURVE ( 'NONE', #31100, #34028, #10805, .T. ) ;
#5091 = CARTESIAN_POINT ( 'NONE',  ( 4.000000000000003553, 3.968388925834817282, 21.63912866391139289 ) ) ;
#5092 = AXIS2_PLACEMENT_3D ( 'NONE', #30970, #366, #22858 ) ;
#5093 = FACE_OUTER_BOUND ( 'NONE', #24107, .T. ) ;
#5094 = EDGE_CURVE ( 'NONE', #18961, #3813, #2577, .T. ) ;
#5095 = CARTESIAN_POINT ( 'NONE',  ( -34.50000000000000000, -113.9929510916434623, 10.50625754673586876 ) ) ;
#5096 = VECTOR ( 'NONE', #8374, 1000.000000000000000 ) ;
#5097 = CARTESIAN_POINT ( 'NONE',  ( -37.18750000000004974, -115.9929510916434481, 13.11852480586264846 ) ) ;
#5098 = CARTESIAN_POINT ( 'NONE',  ( 7.999999999999992895, 0.6505223195683029758, 51.99593080916758936 ) ) ;
#5099 = VECTOR ( 'NONE', #5822, 1000.000000000000000 ) ;
#5100 =( REPRESENTATION_RELATIONSHIP ('NONE','NONE', #26607, #33742 ) REPRESENTATION_RELATIONSHIP_WITH_TRANSFORMATION ( #6367 )SHAPE_REPRESENTATION_RELATIONSHIP( ) );
#5101 = DIRECTION ( 'NONE',  ( 0.000000000000000000, 0.9510565162951523099, 0.3090169943749513370 ) ) ;
#5102 = ORIENTED_EDGE ( 'NONE', *, *, #30443, .F. ) ;
#5103 = EDGE_CURVE ( 'NONE', #9658, #16930, #817, .T. ) ;
#5104 = DIRECTION ( 'NONE',  ( 0.000000000000000000, 0.000000000000000000, -1.000000000000000000 ) ) ;
#5105 = CARTESIAN_POINT ( 'NONE',  ( 44.00000000000000000, 11.00000000000001066, 0.000000000000000000 ) ) ;
#5106 = AXIS2_PLACEMENT_3D ( 'NONE', #16854, #3201, #30908 ) ;
#5107 = DIRECTION ( 'NONE',  ( 0.000000000000000000, 0.000000000000000000, 1.000000000000000000 ) ) ;
#5108 = ADVANCED_FACE ( 'NONE', ( #5235 ), #21049, .T. ) ;
#5109 = VERTEX_POINT ( 'NONE', #16175 ) ;
#5110 = CARTESIAN_POINT ( 'NONE',  ( -50.00000000000000000, 0.000000000000000000, 0.000000000000000000 ) ) ;
#5111 = CARTESIAN_POINT ( 'NONE',  ( -35.50000000000000000, -113.0140978167138712, 0.3752176474015639918 ) ) ;
#5112 = DIRECTION ( 'NONE',  ( -1.000000000000000000, 0.000000000000000000, 0.000000000000000000 ) ) ;
#5113 = CARTESIAN_POINT ( 'NONE',  ( -35.50000000000000711, -114.9929501463477663, 10.50247632894551231 ) ) ;
#5114 = DIRECTION ( 'NONE',  ( -1.000000000000000000, -0.000000000000000000, -0.000000000000000000 ) ) ;
#5115 = VERTEX_POINT ( 'NONE', #10274 ) ;
#5116 = CARTESIAN_POINT ( 'NONE',  ( 8.000000000000007105, 0.000000000000000000, 0.000000000000000000 ) ) ;
#5117 = CARTESIAN_POINT ( 'NONE',  ( -35.50000000000000000, -111.0140821919084715, 0.8283428459075261596 ) ) ;
#5118 = ORIENTED_EDGE ( 'NONE', *, *, #26925, .F. ) ;
#5119 = ORIENTED_EDGE ( 'NONE', *, *, #4225, .F. ) ;
#5120 = CARTESIAN_POINT ( 'NONE',  ( -37.47347596530441649, -114.9754527089670262, 6.472274454178449155 ) ) ;
#5121 = CIRCLE ( 'NONE', #5675, 47.49900000000001654 ) ;
#5122 = EDGE_CURVE ( 'NONE', #18755, #33477, #10451, .T. ) ;
#5123 = DIRECTION ( 'NONE',  ( 1.000000000000000000, -0.000000000000000000, 0.000000000000000000 ) ) ;
#5124 = ORIENTED_EDGE ( 'NONE', *, *, #9438, .F. ) ;
#5125 = EDGE_LOOP ( 'NONE', ( #27947, #16717, #4515, #11775 ) ) ;
#5126 = AXIS2_PLACEMENT_3D ( 'NONE', #6386, #28352, #625 ) ;
#5127 = CARTESIAN_POINT ( 'NONE',  ( -34.50000000000000000, -113.0140978167138712, 0.7502176474015694874 ) ) ;
#5128 = DIRECTION ( 'NONE',  ( 0.000000000000000000, 0.000000000000000000, 1.000000000000000000 ) ) ;
#5129 = PRODUCT_DEFINITION ( 'UNKNOWN', '', #4613, #9044 ) ;
#5130 = ADVANCED_FACE ( 'NONE', ( #2536 ), #21411, .T. ) ;
#5131 = CARTESIAN_POINT ( 'NONE',  ( 0.000000000000000000, 19.60123832284022782, -3.973846525876240765 ) ) ;
#5132 = DIRECTION ( 'NONE',  ( 0.000000000000000000, 0.4999999999999951150, 0.8660254037844414832 ) ) ;
#5133 = CARTESIAN_POINT ( 'NONE',  ( -37.97447287825094975, -114.9929510916434339, 12.77960891308616809 ) ) ;
#5134 = CARTESIAN_POINT ( 'NONE',  ( -39.49999999999999289, -12.06102132296306451, 91.30451528491657598 ) ) ;
#5135 = EDGE_CURVE ( 'NONE', #31456, #19390, #25564, .T. ) ;
#5136 = CARTESIAN_POINT ( 'NONE',  ( 0.000000000000000000, 0.000000000000000000, 0.000000000000000000 ) ) ;
#5137 = EDGE_CURVE ( 'NONE', #33885, #18771, #32232, .T. ) ;
#5138 = CARTESIAN_POINT ( 'NONE',  ( -34.50000000000000000, -115.0468226098135744, -1.624774171496087716 ) ) ;
#5139 = CARTESIAN_POINT ( 'NONE',  ( -55.00000000000000000, -2.775557561562891351E-14, 110.0000000000000000 ) ) ;
#5140 = DIRECTION ( 'NONE',  ( -1.000000000000000000, 0.000000000000000000, 0.000000000000000000 ) ) ;
#5141 = VERTEX_POINT ( 'NONE', #32054 ) ;
#5142 = VECTOR ( 'NONE', #3695, 1000.000000000000000 ) ;
#5143 = CARTESIAN_POINT ( 'NONE',  ( -38.00000000000000711, -115.9929510916434481, 12.26648026267477221 ) ) ;
#5144 = CARTESIAN_POINT ( 'NONE',  ( 7.999999999999992895, 17.50309955389611716, 43.60271849949368317 ) ) ;
#5145 = CARTESIAN_POINT ( 'NONE',  ( -21.15833593587365513, -42.98076211353323828, 83.49999999999991473 ) ) ;
#5146 = DIRECTION ( 'NONE',  ( -1.000000000000000000, 0.000000000000000000, 0.000000000000000000 ) ) ;
#5147 = LINE ( 'NONE', #24580, #30329 ) ;
#5148 = EDGE_CURVE ( 'NONE', #29518, #34240, #7727, .T. ) ;
#5149 = ORIENTED_EDGE ( 'NONE', *, *, #7263, .T. ) ;
#5150 = AXIS2_PLACEMENT_3D ( 'NONE', #16069, #24559, #35553 ) ;
#5151 = DIRECTION ( 'NONE',  ( 1.000000000000000000, -0.000000000000000000, -0.000000000000000000 ) ) ;
#5152 = DIRECTION ( 'NONE',  ( 0.000000000000000000, 0.000000000000000000, 1.000000000000000000 ) ) ;
#5153 = CYLINDRICAL_SURFACE ( 'NONE', #2178, 15.49899999999998457 ) ;
#5154 = DIRECTION ( 'NONE',  ( -1.000000000000000000, 0.000000000000000000, 0.000000000000000000 ) ) ;
#5155 = CARTESIAN_POINT ( 'NONE',  ( 4.000000000000000000, 13.24207120356965461, 14.98824707027445768 ) ) ;
#5156 = DIRECTION ( 'NONE',  ( -1.000000000000000000, 0.000000000000000000, 0.000000000000000000 ) ) ;
#5157 = ORIENTED_EDGE ( 'NONE', *, *, #18480, .T. ) ;
#5158 = VERTEX_POINT ( 'NONE', #1994 ) ;
#5159 = CARTESIAN_POINT ( 'NONE',  ( -34.49999999999998579, -12.31102132296306451, 91.23752798680880005 ) ) ;
#5160 = DIRECTION ( 'NONE',  ( 0.000000000000000000, -0.6427876096865456912, 0.7660444431189726844 ) ) ;
#5161 = CARTESIAN_POINT ( 'NONE',  ( -34.49999999999998579, -18.23076211353324183, 92.74999999999997158 ) ) ;
#5162 = ORIENTED_EDGE ( 'NONE', *, *, #25330, .F. ) ;
#5163 = CARTESIAN_POINT ( 'NONE',  ( -35.62769128460905677, -112.5438815906447729, 3.808975545821551290 ) ) ;
#5164 = ORIENTED_EDGE ( 'NONE', *, *, #31526, .T. ) ;
#5165 = EDGE_CURVE ( 'NONE', #27200, #11310, #35341, .T. ) ;
#5166 = SHAPE_REPRESENTATION_RELATIONSHIP ( 'NONE' , 'NONE' ,  #13971, #12087 ) ;
#5167 = ORIENTED_EDGE ( 'NONE', *, *, #33726, .T. ) ;
#5168 = ORIENTED_EDGE ( 'NONE', *, *, #32346, .T. ) ;
#5169 = LINE ( 'NONE', #2116, #8557 ) ;
#5170 = EDGE_CURVE ( 'NONE', #4180, #7835, #27366, .T. ) ;
#5171 = ADVANCED_FACE ( 'NONE', ( #2362 ), #13681, .T. ) ;
#5172 = PLANE ( 'NONE',  #19101 ) ;
#5173 = ORIENTED_EDGE ( 'NONE', *, *, #29602, .T. ) ;
#5174 = VERTEX_POINT ( 'NONE', #22297 ) ;
#5175 = AXIS2_PLACEMENT_3D ( 'NONE', #17449, #14748, #18525 ) ;
#5176 = DIRECTION ( 'NONE',  ( -1.000000000000000000, 0.000000000000000000, 0.000000000000000000 ) ) ;
#5177 = CARTESIAN_POINT ( 'NONE',  ( -39.49999999999999289, 0.4463568765849662556, 113.0433323525902125 ) ) ;
#5178 = EDGE_CURVE ( 'NONE', #18718, #18057, #8259, .T. ) ;
#5179 = VECTOR ( 'NONE', #10667, 1000.000000000000000 ) ;
#5180 = AXIS2_PLACEMENT_3D ( 'NONE', #1613, #17260, #17436 ) ;
#5181 = DIRECTION ( 'NONE',  ( -1.000000000000000000, 0.000000000000000000, 0.000000000000000000 ) ) ;
#5182 = EDGE_CURVE ( 'NONE', #32593, #5158, #14054, .T. ) ;
#5183 = AXIS2_PLACEMENT_3D ( 'NONE', #18695, #7891, #21221 ) ;
#5184 = LINE ( 'NONE', #5521, #21124 ) ;
#5185 = CARTESIAN_POINT ( 'NONE',  ( 7.999999999999992895, 27.79676263918186052, 37.88001506494778425 ) ) ;
#5186 = CARTESIAN_POINT ( 'NONE',  ( -38.97545270896704039, -113.1123104723225055, 5.347274454178449155 ) ) ;
#5187 = CARTESIAN_POINT ( 'NONE',  ( -37.59808119975203766, -115.9929510916434481, 14.11551573851449071 ) ) ;
#5188 = DIRECTION ( 'NONE',  ( 0.000000000000000000, 0.000000000000000000, -1.000000000000000000 ) ) ;
#5189 = CARTESIAN_POINT ( 'NONE',  ( 0.000000000000000000, 0.000000000000000000, 0.000000000000000000 ) ) ;
#5190 = CYLINDRICAL_SURFACE ( 'NONE', #33155, 4.000000000000000000 ) ;
#5191 = CYLINDRICAL_SURFACE ( 'NONE', #29029, 3.799999999999999822 ) ;
#5192 = CARTESIAN_POINT ( 'NONE',  ( -37.49999999999999289, -11.52052244843579309, 118.1848168619253556 ) ) ;
#5193 =( NAMED_UNIT ( * ) PLANE_ANGLE_UNIT ( ) SI_UNIT ( $, .RADIAN. ) );
#5194 = ORIENTED_EDGE ( 'NONE', *, *, #657, .F. ) ;
#5195 = CIRCLE ( 'NONE', #12662, 7.020000000000045759 ) ;
#5196 = CARTESIAN_POINT ( 'NONE',  ( -34.02454729103297382, -112.6980969099494132, 9.902725545821553510 ) ) ;
#5197 = CYLINDRICAL_SURFACE ( 'NONE', #31343, 20.00000000000000355 ) ;
#5198 = LINE ( 'NONE', #1646, #8429 ) ;
#5199 = CYLINDRICAL_SURFACE ( 'NONE', #22826, 20.00000000000000355 ) ;
#5200 = ORIENTED_EDGE ( 'NONE', *, *, #7172, .F. ) ;
#5201 = CIRCLE ( 'NONE', #4068, 47.49900000000000944 ) ;
#5202 = CARTESIAN_POINT ( 'NONE',  ( -34.50000000000000000, -113.9344536409997630, 0.9850770315317123327 ) ) ;
#5203 = ORIENTED_EDGE ( 'NONE', *, *, #9976, .F. ) ;
#5204 = DIRECTION ( 'NONE',  ( 0.000000000000000000, 0.000000000000000000, 1.000000000000000000 ) ) ;
#5205 = CARTESIAN_POINT ( 'NONE',  ( -3.799999999999999822, 4.653657836759942730E-16, 35.10000000000000142 ) ) ;
#5206 = ORIENTED_EDGE ( 'NONE', *, *, #23066, .F. ) ;
#5207 = ORIENTED_EDGE ( 'NONE', *, *, #241, .F. ) ;
#5208 = AXIS2_PLACEMENT_3D ( 'NONE', #7684, #26980, #7865 ) ;
#5209 = EDGE_LOOP ( 'NONE', ( #23961, #2216, #35094, #7402 ) ) ;
#5210 = AXIS2_PLACEMENT_3D ( 'NONE', #7374, #10787, #2347 ) ;
#5211 = EDGE_CURVE ( 'NONE', #25508, #21169, #27719, .T. ) ;
#5212 = DIRECTION ( 'NONE',  ( -1.000000000000000000, 0.000000000000000000, 0.000000000000000000 ) ) ;
#5213 = DIRECTION ( 'NONE',  ( 1.000000000000000000, 0.000000000000000000, 0.000000000000000000 ) ) ;
#5214 = DIRECTION ( 'NONE',  ( 6.674297938534164038E-17, 0.9946645111845822118, 0.1031625425720821693 ) ) ;
#5215 = LINE ( 'NONE', #18871, #17297 ) ;
#5216 = VERTEX_POINT ( 'NONE', #33292 ) ;
#5217 = VERTEX_POINT ( 'NONE', #33628 ) ;
#5218 = CARTESIAN_POINT ( 'NONE',  ( -35.50000000000000711, -114.0000000000000853, 2.000000000000001776 ) ) ;
#5219 = DIRECTION ( 'NONE',  ( 0.000000000000000000, 0.000000000000000000, 1.000000000000000000 ) ) ;
#5220 = AXIS2_PLACEMENT_3D ( 'NONE', #767, #6000, #14267 ) ;
#5221 = DIRECTION ( 'NONE',  ( 1.000000000000000000, 0.000000000000000000, 0.000000000000000000 ) ) ;
#5222 = ORIENTED_EDGE ( 'NONE', *, *, #877, .F. ) ;
#5223 = DIRECTION ( 'NONE',  ( -1.000000000000000000, 0.000000000000000000, 0.000000000000000000 ) ) ;
#5224 = CARTESIAN_POINT ( 'NONE',  ( -34.50000000000000000, -116.0140978167138712, -0.4997823525984418369 ) ) ;
#5225 = CARTESIAN_POINT ( 'NONE',  ( -35.95093014754292682, -114.9929510916434339, 14.11777216781842448 ) ) ;
#5226 = FACE_OUTER_BOUND ( 'NONE', #23693, .T. ) ;
#5227 = CARTESIAN_POINT ( 'NONE',  ( -35.50000000000000000, -113.9929510916434339, 10.50625754673588474 ) ) ;
#5228 = DIRECTION ( 'NONE',  ( 0.000000000000000000, 0.000000000000000000, 1.000000000000000000 ) ) ;
#5229 = CARTESIAN_POINT ( 'NONE',  ( -39.00000000000000000, -113.9929510916434339, 12.59102132592609102 ) ) ;
#5230 = DIRECTION ( 'NONE',  ( -1.000000000000000000, -0.000000000000000000, -0.000000000000000000 ) ) ;
#5231 = DIRECTION ( 'NONE',  ( 0.000000000000000000, -0.5000000000000092149, 0.8660254037844333785 ) ) ;
#5232 = CARTESIAN_POINT ( 'NONE',  ( 7.999999999999992895, -17.08890430202781374, 43.76671000081938701 ) ) ;
#5233 = ORIENTED_EDGE ( 'NONE', *, *, #32854, .T. ) ;
#5234 = CARTESIAN_POINT ( 'NONE',  ( 0.000000000000000000, 5.667686777401707232, 46.64153600743606631 ) ) ;
#5235 = FACE_OUTER_BOUND ( 'NONE', #33749, .T. ) ;
#5236 = ORIENTED_EDGE ( 'NONE', *, *, #33283, .F. ) ;
#5237 = CARTESIAN_POINT ( 'NONE',  ( -37.66108410722335265, -114.9929510916434339, 13.09299768411426790 ) ) ;
#5238 = ORIENTED_EDGE ( 'NONE', *, *, #20458, .F. ) ;
#5239 = CARTESIAN_POINT ( 'NONE',  ( -35.62769128460905677, -115.4561184093552413, 7.691024454178449155 ) ) ;
#5240 = CARTESIAN_POINT ( 'NONE',  ( 7.999999999999992895, 25.61928775981107265, -45.25098998563451147 ) ) ;
#5241 = ORIENTED_EDGE ( 'NONE', *, *, #29308, .F. ) ;
#5242 = ORIENTED_EDGE ( 'NONE', *, *, #16113, .T. ) ;
#5243 = LINE ( 'NONE', #27379, #33207 ) ;
#5244 = DIRECTION ( 'NONE',  ( -1.000000000000000000, 0.000000000000000000, 0.000000000000000000 ) ) ;
#5245 = AXIS2_PLACEMENT_3D ( 'NONE', #28406, #30931, #3749 ) ;
#5246 = ORIENTED_EDGE ( 'NONE', *, *, #18229, .T. ) ;
#5247 = CARTESIAN_POINT ( 'NONE',  ( -34.00000000000000000, -113.9407375970686758, 2.496475545821551290 ) ) ;
#5248 = DIRECTION ( 'NONE',  ( -1.000000000000000000, 0.000000000000000000, -0.000000000000000000 ) ) ;
#5249 = EDGE_CURVE ( 'NONE', #13216, #19089, #3057, .T. ) ;
#5250 = CARTESIAN_POINT ( 'NONE',  ( -35.50000000000000711, -116.0140978167138712, 0.8752176474015622709 ) ) ;
#5251 = EDGE_LOOP ( 'NONE', ( #31104, #6666, #24073, #34586 ) ) ;
#5252 = ORIENTED_EDGE ( 'NONE', *, *, #29758, .T. ) ;
#5253 = CARTESIAN_POINT ( 'NONE',  ( -9.999999999999994671, 0.000000000000000000, 0.000000000000000000 ) ) ;
#5254 = VECTOR ( 'NONE', #26166, 1000.000000000000000 ) ;
#5255 = STYLED_ITEM ( 'NONE', ( #25657 ), #3950 ) ;
#5256 = FILL_AREA_STYLE_COLOUR ( '', #17344 ) ;
#5257 = AXIS2_PLACEMENT_3D ( 'NONE', #29161, #26458, #10056 ) ;
#5258 = CYLINDRICAL_SURFACE ( 'NONE', #33978, 8.000000000000001776 ) ;
#5259 = ORIENTED_EDGE ( 'NONE', *, *, #9211, .F. ) ;
#5260 = VERTEX_POINT ( 'NONE', #5917 ) ;
#5261 = CARTESIAN_POINT ( 'NONE',  ( -34.50000000000000000, -111.4147656069378058, -1.853877267569947529 ) ) ;
#5262 = EDGE_CURVE ( 'NONE', #19686, #31127, #17495, .T. ) ;
#5263 = DIRECTION ( 'NONE',  ( 1.000000000000000000, 0.000000000000000000, 0.000000000000000000 ) ) ;
#5264 = EDGE_LOOP ( 'NONE', ( #32286, #15409, #28994, #19073 ) ) ;
#5265 = CARTESIAN_POINT ( 'NONE',  ( -35.50000000000000711, -114.9929510916434339, 10.59426868253284226 ) ) ;
#5266 = CARTESIAN_POINT ( 'NONE',  ( -36.00976557831293690, -113.9929510916434339, 14.11852773550420359 ) ) ;
#5267 = DIRECTION ( 'NONE',  ( 0.000000000000000000, -6.938893903907203726E-17, -1.000000000000000000 ) ) ;
#5268 = CARTESIAN_POINT ( 'NONE',  ( 0.000000000000000000, 0.000000000000000000, 0.000000000000000000 ) ) ;
#5269 = CARTESIAN_POINT ( 'NONE',  ( -38.00000000000000711, -113.9929510916434339, 12.57451923796417681 ) ) ;
#5270 = CARTESIAN_POINT ( 'NONE',  ( -37.66108410722335265, -115.9929510916434481, 13.09299768411426612 ) ) ;
#5271 = CARTESIAN_POINT ( 'NONE',  ( -10.00000000000000000, 0.000000000000000000, 0.000000000000000000 ) ) ;
#5272 = CARTESIAN_POINT ( 'NONE',  ( 65.00000000000001421, -30.47068043442695284, 88.33026027086506815 ) ) ;
#5273 = ORIENTED_EDGE ( 'NONE', *, *, #22487, .F. ) ;
#5274 = VECTOR ( 'NONE', #28232, 1000.000000000000000 ) ;
#5275 = DIRECTION ( 'NONE',  ( -1.000000000000000000, -1.836970198721029934E-16, -0.000000000000000000 ) ) ;
#5276 = DIRECTION ( 'NONE',  ( 1.000000000000000000, 0.000000000000000000, 0.000000000000000000 ) ) ;
#5277 = CIRCLE ( 'NONE', #12147, 4.000000000000000000 ) ;
#5278 = FACE_OUTER_BOUND ( 'NONE', #24335, .T. ) ;
#5279 = EDGE_CURVE ( 'NONE', #25119, #16586, #7174, .T. ) ;
#5280 = VERTEX_POINT ( 'NONE', #11665 ) ;
#5281 = DIRECTION ( 'NONE',  ( 0.000000000000000000, 0.000000000000000000, 1.000000000000000000 ) ) ;
#5282 = VERTEX_POINT ( 'NONE', #19582 ) ;
#5283 = CARTESIAN_POINT ( 'NONE',  ( -35.50000000000000711, -116.0140978167138712, -0.1247823525984439463 ) ) ;
#5284 = DIRECTION ( 'NONE',  ( -0.000000000000000000, 0.000000000000000000, -1.000000000000000000 ) ) ;
#5285 = CARTESIAN_POINT ( 'NONE',  ( -35.50000000000000711, -114.9929296450195721, 10.49869535309826674 ) ) ;
#5286 = DIRECTION ( 'NONE',  ( 0.000000000000000000, 0.000000000000000000, -1.000000000000000000 ) ) ;
#5287 = VERTEX_POINT ( 'NONE', #8960 ) ;
#5288 = CARTESIAN_POINT ( 'NONE',  ( -3.160591952521663028, -3.281206521718052382, 0.000000000000000000 ) ) ;
#5289 = EDGE_CURVE ( 'NONE', #12439, #23662, #25197, .T. ) ;
#5290 = CARTESIAN_POINT ( 'NONE',  ( -35.50000000000000000, -112.0066700803175763, -2.372276521656937920 ) ) ;
#5291 = ORIENTED_EDGE ( 'NONE', *, *, #5443, .T. ) ;
#5292 = EDGE_LOOP ( 'NONE', ( #13744, #22570, #19434, #35394 ) ) ;
#5293 = EDGE_CURVE ( 'NONE', #6915, #2288, #1426, .T. ) ;
#5294 = CARTESIAN_POINT ( 'NONE',  ( -35.97545270896702618, -113.6450488405582604, 8.909774454178450043 ) ) ;
#5295 = PRESENTATION_STYLE_ASSIGNMENT (( #13222 ) ) ;
#5296 = DIRECTION ( 'NONE',  ( -1.000000000000000000, 0.000000000000000000, 0.000000000000000000 ) ) ;
#5297 = EDGE_LOOP ( 'NONE', ( #4980, #5563, #26332, #12257 ) ) ;
#5298 = EDGE_LOOP ( 'NONE', ( #28096, #24123 ) ) ;
#5299 = CARTESIAN_POINT ( 'NONE',  ( -34.50000000000000000, -113.0140978167143260, -0.6247823525984285142 ) ) ;
#5300 = CARTESIAN_POINT ( 'NONE',  ( 2.000000000000002665, -5.412337245047654898E-16, -7.800000000000051337 ) ) ;
#5301 = ADVANCED_FACE ( 'NONE', ( #3415 ), #14363, .T. ) ;
#5302 = VECTOR ( 'NONE', #5780, 1000.000000000000000 ) ;
#5303 = AXIS2_PLACEMENT_3D ( 'NONE', #9310, #31099, #6423 ) ;
#5304 = LINE ( 'NONE', #16242, #22925 ) ;
#5305 = EDGE_CURVE ( 'NONE', #29834, #8656, #6574, .T. ) ;
#5306 = DIRECTION ( 'NONE',  ( -1.000000000000000000, -0.000000000000000000, 0.000000000000000000 ) ) ;
#5307 = CARTESIAN_POINT ( 'NONE',  ( -35.50000000000000000, -113.9929510916434339, 10.55026311463432087 ) ) ;
#5308 = CARTESIAN_POINT ( 'NONE',  ( 0.000000000000000000, 0.000000000000000000, -40.40000000000000568 ) ) ;
#5309 = DIRECTION ( 'NONE',  ( -1.000000000000000000, 0.000000000000000000, 0.000000000000000000 ) ) ;
#5310 = CARTESIAN_POINT ( 'NONE',  ( -34.50000000000000000, -112.0140978167138712, 0.2502176474015765373 ) ) ;
#5311 = CARTESIAN_POINT ( 'NONE',  ( -34.50120407906360498, -115.9929510916434481, 12.67985367974112343 ) ) ;
#5312 = DIRECTION ( 'NONE',  ( -1.000000000000000000, 0.000000000000000000, 0.000000000000000000 ) ) ;
#5313 = CIRCLE ( 'NONE', #27159, 52.00000000000000711 ) ;
#5314 = CARTESIAN_POINT ( 'NONE',  ( 4.000000000000000000, 7.317194182740413666, -18.61340026142641690 ) ) ;
#5315 = ORIENTED_EDGE ( 'NONE', *, *, #24033, .F. ) ;
#5316 = CARTESIAN_POINT ( 'NONE',  ( -35.50000000000000711, -114.0743172650041686, 9.508870970061893857 ) ) ;
#5317 = LINE ( 'NONE', #7998, #24027 ) ;
#5318 = LINE ( 'NONE', #19153, #16229 ) ;
#5319 = EDGE_CURVE ( 'NONE', #2939, #31530, #15765, .T. ) ;
#5320 = CARTESIAN_POINT ( 'NONE',  ( -9.999999999999994671, 0.000000000000000000, 0.000000000000000000 ) ) ;
#5321 = EDGE_LOOP ( 'NONE', ( #17064, #15114, #2783, #31356 ) ) ;
#5322 = CARTESIAN_POINT ( 'NONE',  ( 1.799999999999996936, -5.412337245047654898E-16, -7.800000000000051337 ) ) ;
#5323 = DIRECTION ( 'NONE',  ( -1.000000000000000000, 1.110223024625156540E-16, 0.000000000000000000 ) ) ;
#5324 = DIRECTION ( 'NONE',  ( -1.000000000000000000, -0.000000000000000000, 0.000000000000000000 ) ) ;
#5325 = CARTESIAN_POINT ( 'NONE',  ( 8.000000000000007105, 9.604183132802424083, -1.108880290975567950 ) ) ;
#5326 = VECTOR ( 'NONE', #31056, 1000.000000000000000 ) ;
#5327 = CARTESIAN_POINT ( 'NONE',  ( 8.000000000000000000, 0.000000000000000000, 0.000000000000000000 ) ) ;
#5328 = DIRECTION ( 'NONE',  ( 0.000000000000000000, -0.3681245526846853022, 0.9297764858882484607 ) ) ;
#5329 = VERTEX_POINT ( 'NONE', #17237 ) ;
#5330 = ORIENTED_EDGE ( 'NONE', *, *, #496, .T. ) ;
#5331 = DIRECTION ( 'NONE',  ( 0.000000000000000000, -0.9510565162951502005, -0.3090169943749580539 ) ) ;
#5332 = EDGE_CURVE ( 'NONE', #28748, #25299, #8325, .T. ) ;
#5333 = DIRECTION ( 'NONE',  ( -1.000000000000000000, 0.000000000000000000, 0.000000000000000000 ) ) ;
#5334 = DIRECTION ( 'NONE',  ( 1.282131172192753642E-16, -6.938893903907203726E-17, -1.000000000000000000 ) ) ;
#5335 = VERTEX_POINT ( 'NONE', #14531 ) ;
#5336 = ADVANCED_FACE ( 'NONE', ( #19235 ), #10978, .T. ) ;
#5337 = CARTESIAN_POINT ( 'NONE',  ( -36.94073759706868287, -115.9999999999999858, 5.871475545821550845 ) ) ;
#5338 = ADVANCED_FACE ( 'NONE', ( #22118 ), #5580, .T. ) ;
#5339 = EDGE_LOOP ( 'NONE', ( #13689, #7556, #30424, #9224 ) ) ;
#5341 = ORIENTED_EDGE ( 'NONE', *, *, #27641, .F. ) ;
#5340 = AXIS2_PLACEMENT_3D ( 'NONE', #31201, #22203, #963 ) ;
#5342 = ORIENTED_EDGE ( 'NONE', *, *, #17563, .T. ) ;
#5343 = CARTESIAN_POINT ( 'NONE',  ( 7.999999999999992895, 49.65209126885785906, -15.44894276735497840 ) ) ;
#5344 = ADVANCED_FACE ( 'NONE', ( #19425 ), #5750, .T. ) ;
#5345 = CARTESIAN_POINT ( 'NONE',  ( 7.999999999999992895, 31.08872492060014991, -41.68322423723069647 ) ) ;
#5346 = ORIENTED_EDGE ( 'NONE', *, *, #14740, .F. ) ;
#5347 = ORIENTED_EDGE ( 'NONE', *, *, #16789, .T. ) ;
#5348 = AXIS2_PLACEMENT_3D ( 'NONE', #1495, #20913, #31381 ) ;
#5349 = DIRECTION ( 'NONE',  ( -1.000000000000000000, 0.000000000000000000, 0.000000000000000000 ) ) ;
#5350 = AXIS2_PLACEMENT_3D ( 'NONE', #17684, #18216, #29222 ) ;
#5351 = CARTESIAN_POINT ( 'NONE',  ( -10.00000000000000000, 0.000000000000000000, 0.000000000000000000 ) ) ;
#5352 = DIRECTION ( 'NONE',  ( -0.000000000000000000, 1.000000000000000000, 0.000000000000000000 ) ) ;
#5353 = DIRECTION ( 'NONE',  ( -1.047965281155515106E-16, 6.938893903907203726E-17, 1.000000000000000000 ) ) ;
#5354 = DIRECTION ( 'NONE',  ( 0.000000000000000000, -0.9980267284282708928, -0.06279051952932436509 ) ) ;
#5355 = LINE ( 'NONE', #2841, #17417 ) ;
#5356 = CARTESIAN_POINT ( 'NONE',  ( -36.15625000000007816, -115.9929510916434481, 14.11852480586265024 ) ) ;
#5357 = DIRECTION ( 'NONE',  ( -1.000000000000000000, 0.000000000000000000, 0.000000000000000000 ) ) ;
#5358 = EDGE_CURVE ( 'NONE', #9823, #30224, #18658, .T. ) ;
#5359 = CARTESIAN_POINT ( 'NONE',  ( 8.000000000000000000, -17.06000345190446055, 10.43821259704015425 ) ) ;
#5360 = AXIS2_PLACEMENT_3D ( 'NONE', #35171, #27416, #29762 ) ;
#5361 = LINE ( 'NONE', #15961, #21056 ) ;
#5362 = DIRECTION ( 'NONE',  ( 0.000000000000000000, 0.000000000000000000, -1.000000000000000000 ) ) ;
#5363 = EDGE_CURVE ( 'NONE', #34165, #17302, #12212, .T. ) ;
#5364 = LINE ( 'NONE', #8220, #31414 ) ;
#5365 = PLANE ( 'NONE',  #12648 ) ;
#5366 = VERTEX_POINT ( 'NONE', #34364 ) ;
#5367 = CARTESIAN_POINT ( 'NONE',  ( -36.02454729103297382, -113.5265240346956261, 3.902725545821552178 ) ) ;
#5368 = CARTESIAN_POINT ( 'NONE',  ( 8.000000000000007105, -1.111908866155017606, -9.433698091065132019 ) ) ;
#5369 = DIRECTION ( 'NONE',  ( -1.000000000000000000, 0.000000000000000000, 0.000000000000000000 ) ) ;
#5370 = CARTESIAN_POINT ( 'NONE',  ( 7.999999999999992895, -47.00885577955417460, 6.806061952192132836 ) ) ;
#5371 = ORIENTED_EDGE ( 'NONE', *, *, #14296, .T. ) ;
#5372 = ORIENTED_EDGE ( 'NONE', *, *, #16356, .T. ) ;
#5373 = AXIS2_PLACEMENT_3D ( 'NONE', #15870, #18406, #27061 ) ;
#5374 = CARTESIAN_POINT ( 'NONE',  ( 0.000000000000000000, 0.000000000000000000, -0.7999999999999951594 ) ) ;
#5375 = AXIS2_PLACEMENT_3D ( 'NONE', #23582, #26111, #12608 ) ;
#5376 = DIRECTION ( 'NONE',  ( -1.000000000000000000, 0.000000000000000000, 0.000000000000000000 ) ) ;
#5377 = ORIENTED_EDGE ( 'NONE', *, *, #3561, .F. ) ;
#5378 = ADVANCED_FACE ( 'NONE', ( #3759 ), #6803, .F. ) ;
#5379 = AXIS2_PLACEMENT_3D ( 'NONE', #24595, #35586, #16814 ) ;
#5380 = VERTEX_POINT ( 'NONE', #7157 ) ;
#5381 = EDGE_CURVE ( 'NONE', #18606, #22707, #26732, .T. ) ;
#5382 = CARTESIAN_POINT ( 'NONE',  ( 7.999999999999992895, 42.60732521687599217, -19.80331771201615609 ) ) ;
#5383 = CARTESIAN_POINT ( 'NONE',  ( 9.714451465470119729E-14, 0.9999999999999870104, -32.00000000000000000 ) ) ;
#5384 = DIRECTION ( 'NONE',  ( -1.794995435874483979E-16, 0.9771500033919933159, 0.2125508665496976812 ) ) ;
#5385 = DIRECTION ( 'NONE',  ( -1.783119874454246424E-31, -1.187911941725854497E-31, 1.000000000000000000 ) ) ;
#5386 = VERTEX_POINT ( 'NONE', #23186 ) ;
#5387 = ORIENTED_EDGE ( 'NONE', *, *, #20047, .F. ) ;
#5388 = CARTESIAN_POINT ( 'NONE',  ( 55.00000000000000711, -25.99649394950422021, 81.00003093645240426 ) ) ;
#5389 = DIRECTION ( 'NONE',  ( 0.000000000000000000, -0.7071067811865483499, 0.7071067811865466846 ) ) ;
#5390 = ORIENTED_EDGE ( 'NONE', *, *, #7142, .F. ) ;
#5391 = CARTESIAN_POINT ( 'NONE',  ( 50.00005079999998969, 14.30000000000000071, 3.000000000000002665 ) ) ;
#5392 = CARTESIAN_POINT ( 'NONE',  ( -34.50000000000000000, -114.5974311500472425, -1.624782352598427959 ) ) ;
#5393 = CIRCLE ( 'NONE', #9408, 20.00000000000000355 ) ;
#5394 = CARTESIAN_POINT ( 'NONE',  ( -36.03125000000004263, -114.9929510916434339, 14.11852480586264846 ) ) ;
#5395 = AXIS2_PLACEMENT_3D ( 'NONE', #13673, #8252, #25002 ) ;
#5396 = CARTESIAN_POINT ( 'NONE',  ( -10.00000000000000178, 0.000000000000000000, 0.000000000000000000 ) ) ;
#5397 = CARTESIAN_POINT ( 'NONE',  ( -35.50000000000000000, -113.9465028010160381, 10.50071319044726081 ) ) ;
#5398 = CARTESIAN_POINT ( 'NONE',  ( 0.000000000000000000, 1.693188892523745936, 15.40623615209872632 ) ) ;
#5399 = CARTESIAN_POINT ( 'NONE',  ( -34.50000000000000000, -114.9929510916434339, 12.44250253426871033 ) ) ;
#5400 = LINE ( 'NONE', #22465, #3281 ) ;
#5401 = EDGE_CURVE ( 'NONE', #13238, #3289, #31820, .T. ) ;
#5402 = CARTESIAN_POINT ( 'NONE',  ( 0.000000000000000000, 12.49559743815781587, 9.169462670380626790 ) ) ;
#5403 = CARTESIAN_POINT ( 'NONE',  ( 0.000000000000000000, 5.400000000000021672, 1.000000000000001776 ) ) ;
#5404 = CARTESIAN_POINT ( 'NONE',  ( 0.000000000000000000, 0.000000000000000000, 0.000000000000000000 ) ) ;
#5405 = CARTESIAN_POINT ( 'NONE',  ( 7.999999999999992895, -11.46872990052412611, 45.56340405422440654 ) ) ;
#5406 = DIRECTION ( 'NONE',  ( 1.000000000000000000, -0.000000000000000000, 0.000000000000000000 ) ) ;
#5407 = EDGE_CURVE ( 'NONE', #23250, #34581, #1408, .T. ) ;
#5408 = ORIENTED_EDGE ( 'NONE', *, *, #9207, .F. ) ;
#5409 = CARTESIAN_POINT ( 'NONE',  ( -0.1374368770859779598, -4.808326913195978491, 0.000000000000000000 ) ) ;
#5410 = VERTEX_POINT ( 'NONE', #31478 ) ;
#5411 = CARTESIAN_POINT ( 'NONE',  ( -34.97545270896703329, -113.2308352781851539, 8.909774454178450043 ) ) ;
#5412 = DIRECTION ( 'NONE',  ( 0.000000000000000000, 0.000000000000000000, 1.000000000000000000 ) ) ;
#5413 = ORIENTED_EDGE ( 'NONE', *, *, #7663, .F. ) ;
#5414 = AXIS2_PLACEMENT_3D ( 'NONE', #12024, #22995, #17584 ) ;
#5415 = VERTEX_POINT ( 'NONE', #17772 ) ;
#5416 = PLANE ( 'NONE',  #426 ) ;
#5417 = DIRECTION ( 'NONE',  ( 0.000000000000000000, 0.000000000000000000, -1.000000000000000000 ) ) ;
#5418 = VERTEX_POINT ( 'NONE', #20110 ) ;
#5419 = CARTESIAN_POINT ( 'NONE',  ( -39.97545270896702618, -115.3019030900506152, 3.152725545821551734 ) ) ;
#5420 = CARTESIAN_POINT ( 'NONE',  ( 8.000000000000000000, 0.000000000000000000, 0.000000000000000000 ) ) ;
#5421 = AXIS2_PLACEMENT_3D ( 'NONE', #21421, #16185, #29553 ) ;
#5422 = DIRECTION ( 'NONE',  ( 1.000000000000000000, -5.339440136655842133E-16, -1.047965281155519420E-16 ) ) ;
#5423 = AXIS2_PLACEMENT_3D ( 'NONE', #9008, #5664, #11062 ) ;
#5424 = ORIENTED_EDGE ( 'NONE', *, *, #18024, .F. ) ;
#5425 = ORIENTED_EDGE ( 'NONE', *, *, #19565, .F. ) ;
#5426 = DIRECTION ( 'NONE',  ( 0.000000000000000000, 0.6845471059286900584, -0.7289686274214103312 ) ) ;
#5427 = CARTESIAN_POINT ( 'NONE',  ( -34.49999999999998579, -12.06102132296306451, 91.30451528491657598 ) ) ;
#5428 = VERTEX_POINT ( 'NONE', #23542 ) ;
#5429 = ORIENTED_EDGE ( 'NONE', *, *, #23302, .F. ) ;
#5430 = CARTESIAN_POINT ( 'NONE',  ( -34.50000000000000000, -111.1162063037085801, -1.269118781493287607 ) ) ;
#5431 = LINE ( 'NONE', #27746, #12168 ) ;
#5432 = VERTEX_POINT ( 'NONE', #28775 ) ;
#5433 = CARTESIAN_POINT ( 'NONE',  ( -35.50000000000000711, -114.9929510916434339, 10.56126450660895699 ) ) ;
#5434 = CARTESIAN_POINT ( 'NONE',  ( -34.68937937320795584, -113.9929510916434339, 13.37409560816408671 ) ) ;
#5435 = CARTESIAN_POINT ( 'NONE',  ( -39.49999999999999289, -13.92619866229204106, 93.69175626110634880 ) ) ;
#5436 = CYLINDRICAL_SURFACE ( 'NONE', #15643, 20.00000000000000711 ) ;
#5437 = CARTESIAN_POINT ( 'NONE',  ( -34.57658136524561598, -113.9929510916434339, 13.10177712753338675 ) ) ;
#5438 = FACE_OUTER_BOUND ( 'NONE', #5083, .T. ) ;
#5439 = CARTESIAN_POINT ( 'NONE',  ( -35.50000000000000711, -114.2305202833893816, 9.534416457224700991 ) ) ;
#5440 = CYLINDRICAL_SURFACE ( 'NONE', #20469, 19.99999999999998579 ) ;
#5442 = AXIS2_PLACEMENT_3D ( 'NONE', #12937, #21734, #13303 ) ;
#5441 = LINE ( 'NONE', #19785, #4330 ) ;
#5443 = EDGE_CURVE ( 'NONE', #18320, #18718, #17590, .T. ) ;
#5444 = ORIENTED_EDGE ( 'NONE', *, *, #24880, .F. ) ;
#5445 = DIRECTION ( 'NONE',  ( 1.000000000000000000, -0.000000000000000000, -0.000000000000000000 ) ) ;
#5446 = DIRECTION ( 'NONE',  ( 0.000000000000000000, 0.000000000000000000, 1.000000000000000000 ) ) ;
#5447 = DIRECTION ( 'NONE',  ( 1.000000000000000000, -0.000000000000000000, 0.000000000000000000 ) ) ;
#5448 = AXIS2_PLACEMENT_3D ( 'NONE', #16888, #27892, #10810 ) ;
#5449 = EDGE_LOOP ( 'NONE', ( #20171, #15087, #11966, #4760 ) ) ;
#5450 = CYLINDRICAL_SURFACE ( 'NONE', #21036, 3.799999999999999822 ) ;
#5451 = ORIENTED_EDGE ( 'NONE', *, *, #3535, .T. ) ;
#5452 = CARTESIAN_POINT ( 'NONE',  ( -35.50000000000000000, -113.0140978167142833, 0.8752176474015604946 ) ) ;
#5453 = LINE ( 'NONE', #11033, #13842 ) ;
#5454 = CARTESIAN_POINT ( 'NONE',  ( -36.02454729103298092, -114.4734759653044307, 4.597274454178449155 ) ) ;
#5455 = ADVANCED_FACE ( 'NONE', ( #4300 ), #31119, .T. ) ;
#5456 = CARTESIAN_POINT ( 'NONE',  ( -35.50000000000000711, -114.9929510916434339, 12.60752341388803544 ) ) ;
#5457 = DIRECTION ( 'NONE',  ( -1.000000000000000000, -0.000000000000000000, 0.000000000000000000 ) ) ;
#5458 = VERTEX_POINT ( 'NONE', #4128 ) ;
#5459 = PLANE ( 'NONE',  #17039 ) ;
#5460 = CARTESIAN_POINT ( 'NONE',  ( -35.50000000000000000, -112.6882700046066645, -2.599147725882136939 ) ) ;
#5461 = ORIENTED_EDGE ( 'NONE', *, *, #28615, .F. ) ;
#5462 = ORIENTED_EDGE ( 'NONE', *, *, #17437, .T. ) ;
#5463 = CARTESIAN_POINT ( 'NONE',  ( -35.62769128460905677, -115.4561184093552413, 7.691024454178449155 ) ) ;
#5464 = LINE ( 'NONE', #19298, #28469 ) ;
#5465 = VERTEX_POINT ( 'NONE', #6445 ) ;
#5466 = ORIENTED_EDGE ( 'NONE', *, *, #5289, .F. ) ;
#5467 = CARTESIAN_POINT ( 'NONE',  ( -34.50000000000000000, -114.5974311500472567, -0.6247823525984269599 ) ) ;
#5468 = FACE_OUTER_BOUND ( 'NONE', #18827, .T. ) ;
#5469 = AXIS2_PLACEMENT_3D ( 'NONE', #4451, #1376, #17383 ) ;
#5470 = AXIS2_PLACEMENT_3D ( 'NONE', #25373, #17063, #19747 ) ;
#5471 = DIRECTION ( 'NONE',  ( 1.691777834109591064E-31, -1.187911941725854715E-31, 1.000000000000000000 ) ) ;
#5472 = VECTOR ( 'NONE', #28959, 1000.000000000000000 ) ;
#5473 = PLANE ( 'NONE',  #10506 ) ;
#5474 = AXIS2_PLACEMENT_3D ( 'NONE', #29955, #22008, #35546 ) ;
#5475 = CARTESIAN_POINT ( 'NONE',  ( -35.50000000000000000, -113.9929510916433912, 10.50625754673588474 ) ) ;
#5476 = LINE ( 'NONE', #29432, #29933 ) ;
#5477 = DIRECTION ( 'NONE',  ( 0.000000000000000000, 0.000000000000000000, 1.000000000000000000 ) ) ;
#5478 = CARTESIAN_POINT ( 'NONE',  ( -34.50000000000000000, -111.0140978167138570, -0.3122823525984338988 ) ) ;
#5479 = CARTESIAN_POINT ( 'NONE',  ( -35.50000000000000000, -114.2265172349312508, 8.519938377296172760 ) ) ;
#5480 = DIRECTION ( 'NONE',  ( -1.174092375852890260E-15, 4.222049128630259891E-16, 1.000000000000000000 ) ) ;
#5481 = EDGE_CURVE ( 'NONE', #19767, #30356, #11769, .T. ) ;
#5482 = ADVANCED_FACE ( 'NONE', ( #6621, #15067 ), #17951, .F. ) ;
#5483 = DIRECTION ( 'NONE',  ( 1.783119874454246424E-31, 1.187911941725854497E-31, -1.000000000000000000 ) ) ;
#5484 = ORIENTED_EDGE ( 'NONE', *, *, #20613, .F. ) ;
#5485 = CARTESIAN_POINT ( 'NONE',  ( -37.66108410722335265, -115.9929510916434481, 13.09299768411426612 ) ) ;
#5486 = DIRECTION ( 'NONE',  ( 0.000000000000000000, -0.7705132427757815927, -0.6374239897486989603 ) ) ;
#5487 = PLANE ( 'NONE',  #26590 ) ;
#5488 = CYLINDRICAL_SURFACE ( 'NONE', #8204, 20.00000000000000711 ) ;
#5489 = DIRECTION ( 'NONE',  ( -1.000000000000000000, 0.000000000000000000, 0.000000000000000000 ) ) ;
#5490 = VERTEX_POINT ( 'NONE', #20642 ) ;
#5491 = DIRECTION ( 'NONE',  ( 0.000000000000000000, 0.000000000000000000, 1.000000000000000000 ) ) ;
#5492 = DIRECTION ( 'NONE',  ( 1.000000000000000000, -0.000000000000000000, 0.000000000000000000 ) ) ;
#5493 = CLOSED_SHELL ( 'NONE', ( #26968, #27749, #28907, #22483, #29677, #13524, #20199, #5336, #7924, #12190, #15124, #8795, #20485, #20576, #27272, #28640, #13379, #17490, #9704, #32827, #29515, #23382, #300, #3358, #28616, #12758, #20945, #24432, #29155, #3506, #20278, #25731, #27800, #4493, #29320, #2045, #9764, #15995, #27342, #34969, #5725, #9052, #20289, #2832, #2900, #31902, #29927, #23062, #34794, #27356, #13730, #4030, #32793, #4759, #7265, #13638 ) ) ;
#5494 = AXIS2_PLACEMENT_3D ( 'NONE', #33073, #19372, #11280 ) ;
#5495 = DIRECTION ( 'NONE',  ( -1.000000000000000000, -0.000000000000000000, -0.000000000000000000 ) ) ;
#5496 = DIRECTION ( 'NONE',  ( -1.000000000000000000, 0.000000000000000000, 0.000000000000000000 ) ) ;
#5497 = CONTEXT_DEPENDENT_SHAPE_REPRESENTATION ( #18636, #31365 ) ;
#5498 = EDGE_CURVE ( 'NONE', #21576, #30905, #34005, .T. ) ;
#5499 = CYLINDRICAL_SURFACE ( 'NONE', #34253, 17.49900000000000233 ) ;
#5500 = PLANE ( 'NONE',  #15316 ) ;
#5501 = AXIS2_PLACEMENT_3D ( 'NONE', #15560, #20609, #31609 ) ;
#5502 = ORIENTED_EDGE ( 'NONE', *, *, #11527, .F. ) ;
#5503 = CYLINDRICAL_SURFACE ( 'NONE', #34862, 11.00000000000000000 ) ;
#5504 = CYLINDRICAL_SURFACE ( 'NONE', #26325, 20.00000000000000711 ) ;
#5505 = CARTESIAN_POINT ( 'NONE',  ( 0.000000000000000000, -6.359167119270331625, -18.96209359615098577 ) ) ;
#5506 = ORIENTED_EDGE ( 'NONE', *, *, #5170, .T. ) ;
#5507 = CARTESIAN_POINT ( 'NONE',  ( -36.94073759706868287, -115.9999999999999858, 7.371475545821551734 ) ) ;
#5508 = VERTEX_POINT ( 'NONE', #26251 ) ;
#5509 = AXIS2_PLACEMENT_3D ( 'NONE', #21410, #7726, #18709 ) ;
#5510 = ORIENTED_EDGE ( 'NONE', *, *, #30673, .F. ) ;
#5511 = ORIENTED_EDGE ( 'NONE', *, *, #25488, .T. ) ;
#5512 = CARTESIAN_POINT ( 'NONE',  ( 3.799999999999999822, 0.000000000000000000, 60.90000000000001279 ) ) ;
#5513 = EDGE_CURVE ( 'NONE', #31100, #11172, #2602, .T. ) ;
#5514 = DIRECTION ( 'NONE',  ( 0.000000000000000000, 0.000000000000000000, -1.000000000000000000 ) ) ;
#5515 = EDGE_LOOP ( 'NONE', ( #12905, #15381 ) ) ;
#5516 = AXIS2_PLACEMENT_3D ( 'NONE', #18629, #13418, #18085 ) ;
#5517 = CARTESIAN_POINT ( 'NONE',  ( -35.50000000000000711, -114.9929510916434339, 10.52826033068511435 ) ) ;
#5518 = DIRECTION ( 'NONE',  ( 1.000000000000000000, 0.000000000000000000, 0.000000000000000000 ) ) ;
#5519 = DIRECTION ( 'NONE',  ( -1.000000000000000000, 0.000000000000000000, 0.000000000000000000 ) ) ;
#5520 = AXIS2_PLACEMENT_3D ( 'NONE', #8524, #25985, #14978 ) ;
#5521 = CARTESIAN_POINT ( 'NONE',  ( 3.872983346207429900, -1.000000000000003553, 55.00000000000000000 ) ) ;
#5522 = CARTESIAN_POINT ( 'NONE',  ( 0.000000000000000000, 7.613867765417711375, -5.679790370315948245 ) ) ;
#5523 = EDGE_CURVE ( 'NONE', #3460, #24278, #8890, .T. ) ;
#5524 = ADVANCED_FACE ( 'NONE', ( #31295 ), #12572, .F. ) ;
#5525 = CARTESIAN_POINT ( 'NONE',  ( 4.000000000000003553, 10.46102064772339979, 19.35373470438986843 ) ) ;
#5526 = ADVANCED_FACE ( 'NONE', ( #11841 ), #15595, .T. ) ;
#5527 = CARTESIAN_POINT ( 'NONE',  ( -38.98077402996267438, -115.9929510916434481, 12.86289566494346204 ) ) ;
#5528 = CYLINDRICAL_SURFACE ( 'NONE', #18245, 3.799999999999999822 ) ;
#5529 = AXIS2_PLACEMENT_3D ( 'NONE', #13950, #6024, #24940 ) ;
#5530 = DIRECTION ( 'NONE',  ( 0.000000000000000000, 0.6427876096865403621, -0.7660444431189771253 ) ) ;
#5531 = PLANE ( 'NONE',  #29720 ) ;
#5532 = DIRECTION ( 'NONE',  ( -1.174092375852890260E-15, 4.222049128630259891E-16, 1.000000000000000000 ) ) ;
#5533 = FACE_OUTER_BOUND ( 'NONE', #29475, .T. ) ;
#5534 =( NAMED_UNIT ( * ) SI_UNIT ( $, .STERADIAN. ) SOLID_ANGLE_UNIT ( ) );
#5535 = ORIENTED_EDGE ( 'NONE', *, *, #2090, .T. ) ;
#5536 = EDGE_CURVE ( 'NONE', #30763, #32738, #10633, .T. ) ;
#5537 = CARTESIAN_POINT ( 'NONE',  ( -39.02454729103295961, -113.2308352781851539, 9.340225545821549957 ) ) ;
#5538 = DIRECTION ( 'NONE',  ( 2.668805347656627171E-16, -1.000000000000000000, 0.000000000000000000 ) ) ;
#5539 = DIRECTION ( 'NONE',  ( 1.000000000000000000, -0.000000000000000000, -0.000000000000000000 ) ) ;
#5540 = CARTESIAN_POINT ( 'NONE',  ( 8.000000000000007105, 9.433698091065187086, -1.111908866155128628 ) ) ;
#5541 = ADVANCED_FACE ( 'NONE', ( #35255 ), #13457, .T. ) ;
#5542 = ORIENTED_EDGE ( 'NONE', *, *, #16562, .T. ) ;
#5543 = ORIENTED_EDGE ( 'NONE', *, *, #18986, .T. ) ;
#5544 = VECTOR ( 'NONE', #22343, 1000.000000000000000 ) ;
#5545 = DIRECTION ( 'NONE',  ( -1.000000000000000000, 0.000000000000000000, 0.000000000000000000 ) ) ;
#5546 = ORIENTED_EDGE ( 'NONE', *, *, #17697, .F. ) ;
#5547 = ORIENTED_EDGE ( 'NONE', *, *, #15003, .F. ) ;
#5548 = AXIS2_PLACEMENT_3D ( 'NONE', #24170, #10124, #2039 ) ;
#5549 = VECTOR ( 'NONE', #16666, 1000.000000000000000 ) ;
#5550 = AXIS2_PLACEMENT_3D ( 'NONE', #23276, #23653, #18051 ) ;
#5551 = DIRECTION ( 'NONE',  ( -1.000000000000000000, -0.000000000000000000, -0.000000000000000000 ) ) ;
#5552 = DIRECTION ( 'NONE',  ( 0.000000000000000000, 0.000000000000000000, 1.000000000000000000 ) ) ;
#5553 = PRESENTATION_LAYER_ASSIGNMENT (  '', '', ( #2131 ) ) ;
#5554 = EDGE_CURVE ( 'NONE', #16680, #26953, #34793, .T. ) ;
#5555 = DIRECTION ( 'NONE',  ( 0.000000000000000000, 0.000000000000000000, -1.000000000000000000 ) ) ;
#5557 = ORIENTED_EDGE ( 'NONE', *, *, #13905, .T. ) ;
#5556 = AXIS2_PLACEMENT_3D ( 'NONE', #27320, #22077, #24438 ) ;
#5558 = ORIENTED_EDGE ( 'NONE', *, *, #30852, .T. ) ;
#5559 = ADVANCED_FACE ( 'NONE', ( #10576 ), #5191, .T. ) ;
#5560 = DIRECTION ( 'NONE',  ( -1.000000000000000000, -0.000000000000000000, 0.000000000000000000 ) ) ;
#5561 = DIRECTION ( 'NONE',  ( -1.000000000000000000, -0.000000000000000000, 0.000000000000000000 ) ) ;
#5562 = EDGE_CURVE ( 'NONE', #31717, #20111, #12749, .T. ) ;
#5563 = ORIENTED_EDGE ( 'NONE', *, *, #32159, .T. ) ;
#5564 = CYLINDRICAL_SURFACE ( 'NONE', #21260, 52.00000000000000711 ) ;
#5565 = CIRCLE ( 'NONE', #1523, 10.99999999999999467 ) ;
#5566 = CARTESIAN_POINT ( 'NONE',  ( -34.50000000000000000, -112.0140978167138712, -0.5622823525984296245 ) ) ;
#5567 = CARTESIAN_POINT ( 'NONE',  ( -38.99984940073101569, -114.9929510916434339, 12.64306614848957189 ) ) ;
#5568 = AXIS2_PLACEMENT_3D ( 'NONE', #7028, #18002, #28999 ) ;
#5569 = ADVANCED_FACE ( 'NONE', ( #18852 ), #32528, .T. ) ;
#5570 = CARTESIAN_POINT ( 'NONE',  ( -35.50000000000000000, -113.9929510916436470, 10.50625754673581724 ) ) ;
#5571 = DIRECTION ( 'NONE',  ( 1.000000000000000000, -0.000000000000000000, -0.000000000000000000 ) ) ;
#5572 = EDGE_CURVE ( 'NONE', #9519, #12635, #4665, .T. ) ;
#5573 = CARTESIAN_POINT ( 'NONE',  ( -34.51202277066418844, -114.9929510916434339, 12.81430620224972294 ) ) ;
#5574 = PLANE ( 'NONE',  #17617 ) ;
#5575 = AXIS2_PLACEMENT_3D ( 'NONE', #31781, #2282, #23869 ) ;
#5576 = DIRECTION ( 'NONE',  ( -1.000000000000000000, 0.000000000000000000, 0.000000000000000000 ) ) ;
#5577 = CYLINDRICAL_SURFACE ( 'NONE', #9484, 15.49899999999998457 ) ;
#5578 = CIRCLE ( 'NONE', #27455, 19.99999999999998579 ) ;
#5579 = LINE ( 'NONE', #10804, #27383 ) ;
#5580 = CYLINDRICAL_SURFACE ( 'NONE', #27312, 7.499999999999992895 ) ;
#5581 = EDGE_LOOP ( 'NONE', ( #5157, #29192, #3774, #25220 ) ) ;
#5582 = DIRECTION ( 'NONE',  ( 0.000000000000000000, 0.000000000000000000, -1.000000000000000000 ) ) ;
#5583 = ORIENTED_EDGE ( 'NONE', *, *, #15851, .F. ) ;
#5584 = CARTESIAN_POINT ( 'NONE',  ( -37.05926240293133134, -116.9999999999999858, 7.878524454178450043 ) ) ;
#5585 = VECTOR ( 'NONE', #20536, 1000.000000000000000 ) ;
#5586 = FACE_OUTER_BOUND ( 'NONE', #2906, .T. ) ;
#5587 = EDGE_CURVE ( 'NONE', #12439, #29235, #29850, .T. ) ;
#5588 = VECTOR ( 'NONE', #31602, 1000.000000000000000 ) ;
#5589 = ORIENTED_EDGE ( 'NONE', *, *, #27567, .T. ) ;
#5590 = ORIENTED_EDGE ( 'NONE', *, *, #33478, .F. ) ;
#5591 = CARTESIAN_POINT ( 'NONE',  ( 7.999999999999992895, 39.64889472655731595, 33.64468972902522381 ) ) ;
#5592 = CARTESIAN_POINT ( 'NONE',  ( 0.000000000000000000, -14.80634052301628145, 8.177498406287162069 ) ) ;
#5593 = EDGE_LOOP ( 'NONE', ( #31361, #24336, #6274, #32233 ) ) ;
#5594 = CARTESIAN_POINT ( 'NONE',  ( -34.83677480945819838, -111.9205845034225462, 7.316024454178450043 ) ) ;
#5595 = AXIS2_PLACEMENT_3D ( 'NONE', #24655, #19577, #27545 ) ;
#5596 = FACE_OUTER_BOUND ( 'NONE', #11254, .T. ) ;
#5597 = VECTOR ( 'NONE', #25086, 1000.000000000000000 ) ;
#5598 = DIRECTION ( 'NONE',  ( -1.000000000000000000, 0.000000000000000000, 0.000000000000000000 ) ) ;
#5599 = ORIENTED_EDGE ( 'NONE', *, *, #5279, .T. ) ;
#5600 = ORIENTED_EDGE ( 'NONE', *, *, #27556, .T. ) ;
#5601 = FACE_OUTER_BOUND ( 'NONE', #30432, .T. ) ;
#5602 = AXIS2_PLACEMENT_3D ( 'NONE', #10715, #27646, #14106 ) ;
#5603 = EDGE_CURVE ( 'NONE', #13189, #34283, #17517, .T. ) ;
#5604 = CARTESIAN_POINT ( 'NONE',  ( 0.000000000000000000, 0.000000000000000000, 55.00000000000000711 ) ) ;
#5605 = ORIENTED_EDGE ( 'NONE', *, *, #34796, .T. ) ;
#5606 = ORIENTED_EDGE ( 'NONE', *, *, #10861, .F. ) ;
#5607 = CARTESIAN_POINT ( 'NONE',  ( -35.50000000000000000, -111.2304026862503719, 1.811733666967775713 ) ) ;
#5608 = AXIS2_PLACEMENT_3D ( 'NONE', #8631, #32778, #19603 ) ;
#5609 = EDGE_CURVE ( 'NONE', #11196, #14042, #7738, .T. ) ;
#5610 = VECTOR ( 'NONE', #19327, 1000.000000000000000 ) ;
#5611 = CYLINDRICAL_SURFACE ( 'NONE', #32296, 52.00000000000000711 ) ;
#5612 = VERTEX_POINT ( 'NONE', #10229 ) ;
#5613 = CARTESIAN_POINT ( 'NONE',  ( -36.12500000000014211, -114.9929510916434339, 13.11852480586264669 ) ) ;
#5614 = CARTESIAN_POINT ( 'NONE',  ( -35.87745010033553683, -113.9929510916434339, 14.11371147303761475 ) ) ;
#5615 = CARTESIAN_POINT ( 'NONE',  ( 8.000000000000007105, 5.679790370316226245, -7.613867765417517752 ) ) ;
#5616 = EDGE_CURVE ( 'NONE', #32249, #2504, #3772, .T. ) ;
#5617 = CARTESIAN_POINT ( 'NONE',  ( 0.000000000000000000, 0.000000000000000000, 0.000000000000000000 ) ) ;
#5618 = ADVANCED_FACE ( 'NONE', ( #18494 ), #8044, .T. ) ;
#5619 = CARTESIAN_POINT ( 'NONE',  ( -34.50000000000000000, -113.9929510916435618, 10.50625754673588474 ) ) ;
#5620 = DIRECTION ( 'NONE',  ( 1.000000000000000000, 0.000000000000000000, 0.000000000000000000 ) ) ;
#5621 = CARTESIAN_POINT ( 'NONE',  ( -35.50000000000000711, -114.9929510916434339, 10.72628538622835670 ) ) ;
#5622 = CIRCLE ( 'NONE', #33778, 7.199999999999993072 ) ;
#5623 = DIRECTION ( 'NONE',  ( 0.000000000000000000, -0.6427876096865295930, -0.7660444431189862291 ) ) ;
#5624 = DIRECTION ( 'NONE',  ( -1.000000000000000000, 0.000000000000000000, 0.000000000000000000 ) ) ;
#5625 = CIRCLE ( 'NONE', #442, 13.99999999999999645 ) ;
#5626 = ORIENTED_EDGE ( 'NONE', *, *, #702, .F. ) ;
#5627 = ORIENTED_EDGE ( 'NONE', *, *, #30440, .T. ) ;
#5628 = CARTESIAN_POINT ( 'NONE',  ( -50.00000000000000000, 19.99999999999998934, -25.00000000000000000 ) ) ;
#5629 = DIRECTION ( 'NONE',  ( -1.000000000000000000, 0.000000000000000000, 0.000000000000000000 ) ) ;
#5630 = ORIENTED_EDGE ( 'NONE', *, *, #8997, .F. ) ;
#5631 = CIRCLE ( 'NONE', #25755, 3.799999999999999822 ) ;
#5632 = DIRECTION ( 'NONE',  ( -1.000000000000000000, 0.000000000000000000, 0.000000000000000000 ) ) ;
#5633 = ORIENTED_EDGE ( 'NONE', *, *, #23519, .T. ) ;
#5634 = CARTESIAN_POINT ( 'NONE',  ( -35.50000000000000000, -113.0140978167138712, 0.8752176474016720720 ) ) ;
#5635 = DIRECTION ( 'NONE',  ( -1.000000000000000000, 0.000000000000000000, -0.000000000000000000 ) ) ;
#5636 = CARTESIAN_POINT ( 'NONE',  ( -37.66520193420439000, -113.2509883718312977, 5.441024454178449155 ) ) ;
#5637 = VECTOR ( 'NONE', #29723, 1000.000000000000000 ) ;
#5638 = CARTESIAN_POINT ( 'NONE',  ( 0.000000000000000000, -2.710505431213761085E-17, -30.00000000000000711 ) ) ;
#5639 = ORIENTED_EDGE ( 'NONE', *, *, #25143, .T. ) ;
#5640 = DIRECTION ( 'NONE',  ( -1.000000000000000000, 0.000000000000000000, 0.000000000000000000 ) ) ;
#5641 = CARTESIAN_POINT ( 'NONE',  ( -35.50000000000000000, -117.0140978167138854, -0.3122823525984416149 ) ) ;
#5642 = VERTEX_POINT ( 'NONE', #29493 ) ;
#5643 = ORIENTED_EDGE ( 'NONE', *, *, #2090, .F. ) ;
#5644 = CARTESIAN_POINT ( 'NONE',  ( -35.54388159064475872, -112.6276912846090568, 7.316024454178449155 ) ) ;
#5645 = FILL_AREA_STYLE ('',( #3652 ) ) ;
#5646 = AXIS2_PLACEMENT_3D ( 'NONE', #19663, #6188, #12120 ) ;
#5647 = LINE ( 'NONE', #3478, #11531 ) ;
#5648 = ORIENTED_EDGE ( 'NONE', *, *, #24708, .T. ) ;
#5649 = ORIENTED_EDGE ( 'NONE', *, *, #25316, .F. ) ;
#5650 = CARTESIAN_POINT ( 'NONE',  ( -34.50000000000000000, -112.8356783780338759, 1.859636627348750348 ) ) ;
#5651 = DIRECTION ( 'NONE',  ( 0.000000000000000000, 0.000000000000000000, 1.000000000000000000 ) ) ;
#5652 = EDGE_CURVE ( 'NONE', #28820, #8675, #32488, .T. ) ;
#5653 = CIRCLE ( 'NONE', #32659, 3.799999999999999822 ) ;
#5654 = LINE ( 'NONE', #21657, #2840 ) ;
#5655 = AXIS2_PLACEMENT_3D ( 'NONE', #32548, #15790, #20835 ) ;
#5656 = AXIS2_PLACEMENT_3D ( 'NONE', #3307, #33530, #8323 ) ;
#5657 = CARTESIAN_POINT ( 'NONE',  ( -35.49999931242378182, -113.9929510916434339, 12.61439929482945743 ) ) ;
#5658 = CARTESIAN_POINT ( 'NONE',  ( -4.000000000000000000, 0.000000000000000000, 55.00000000000000000 ) ) ;
#5659 = DIRECTION ( 'NONE',  ( 0.000000000000000000, -0.9510565162951500895, -0.3090169943749581094 ) ) ;
#5660 = CARTESIAN_POINT ( 'NONE',  ( -34.50000000000000000, -111.0140978167138570, 0.7189676474015717078 ) ) ;
#5661 = CARTESIAN_POINT ( 'NONE',  ( -37.54906985245723661, -115.9929510916434481, 14.11777216781844757 ) ) ;
#5662 = LINE ( 'NONE', #33198, #25645 ) ;
#5663 = CARTESIAN_POINT ( 'NONE',  ( 7.999999999999992895, 45.78515115856044559, 12.64416602183680816 ) ) ;
#5664 = DIRECTION ( 'NONE',  ( 1.000000000000000000, 1.734723475976807094E-16, 0.000000000000000000 ) ) ;
#5665 = ORIENTED_EDGE ( 'NONE', *, *, #31919, .F. ) ;
#5666 = CARTESIAN_POINT ( 'NONE',  ( -35.50000000000000711, -114.0928965812550757, 9.511088712577292270 ) ) ;
#5667 = DIRECTION ( 'NONE',  ( -1.174092375852890260E-15, 4.222049128630259891E-16, 1.000000000000000000 ) ) ;
#5668 =( LENGTH_UNIT ( ) NAMED_UNIT ( * ) SI_UNIT ( .MILLI., .METRE. ) );
#5669 = CARTESIAN_POINT ( 'NONE',  ( 0.000000000000000000, 0.000000000000000000, 0.000000000000000000 ) ) ;
#5670 = VERTEX_POINT ( 'NONE', #1768 ) ;
#5671 = CARTESIAN_POINT ( 'NONE',  ( 4.000000000000000000, 4.898587196589412829E-16, 55.00000000000000000 ) ) ;
#5672 = CYLINDRICAL_SURFACE ( 'NONE', #11817, 8.000000000000000000 ) ;
#5673 = CARTESIAN_POINT ( 'NONE',  ( -34.49999999999998579, -37.28532556477448168, 93.25874355921402525 ) ) ;
#5674 = CARTESIAN_POINT ( 'NONE',  ( 8.000000000000007105, 8.725776631572770725, -3.753907720748954180 ) ) ;
#5675 = AXIS2_PLACEMENT_3D ( 'NONE', #24127, #2182, #35118 ) ;
#5676 = AXIS2_PLACEMENT_3D ( 'NONE', #12152, #25489, #11979 ) ;
#5677 = DIRECTION ( 'NONE',  ( 0.000000000000000000, 0.000000000000000000, 1.000000000000000000 ) ) ;
#5678 = DIRECTION ( 'NONE',  ( 0.000000000000000000, 0.8090169943749490056, -0.5877852522924709167 ) ) ;
#5679 = ORIENTED_EDGE ( 'NONE', *, *, #5977, .T. ) ;
#5680 = AXIS2_PLACEMENT_3D ( 'NONE', #11738, #16948, #24905 ) ;
#5681 = SHAPE_REPRESENTATION ( 'shaft2', ( #21307 ), #21360 ) ;
#5682 = LINE ( 'NONE', #11428, #18182 ) ;
#5683 = DIRECTION ( 'NONE',  ( 0.000000000000000000, 0.000000000000000000, 1.000000000000000000 ) ) ;
#5684 = CARTESIAN_POINT ( 'NONE',  ( 0.000000000000000000, 36.05989434073656241, -30.12041790338579261 ) ) ;
#5685 = EDGE_LOOP ( 'NONE', ( #32579, #12274 ) ) ;
#5686 = CARTESIAN_POINT ( 'NONE',  ( -37.35495115944176803, -115.0245472910329880, 4.465225545821550845 ) ) ;
#5687 = ORIENTED_EDGE ( 'NONE', *, *, #32711, .T. ) ;
#5688 = EDGE_LOOP ( 'NONE', ( #24189, #5820, #34328, #22516 ) ) ;
#5689 = EDGE_LOOP ( 'NONE', ( #27939, #30777, #560, #31615 ) ) ;
#5690 = FACE_OUTER_BOUND ( 'NONE', #25878, .T. ) ;
#5691 = EDGE_CURVE ( 'NONE', #2768, #16982, #16386, .T. ) ;
#5692 = DIRECTION ( 'NONE',  ( 1.000000000000000000, 0.000000000000000000, 0.000000000000000000 ) ) ;
#5693 = CARTESIAN_POINT ( 'NONE',  ( -35.50000000000000711, -114.1021862393805577, 9.512197583835053649 ) ) ;
#5694 = LINE ( 'NONE', #31059, #6868 ) ;
#5695 = ADVANCED_FACE ( 'NONE', ( #13120 ), #21003, .T. ) ;
#5696 = DIRECTION ( 'NONE',  ( 0.000000000000000000, 0.000000000000000000, 1.000000000000000000 ) ) ;
#5697 = DIRECTION ( 'NONE',  ( 0.000000000000000000, 0.000000000000000000, -1.000000000000000000 ) ) ;
#5698 = CARTESIAN_POINT ( 'NONE',  ( -5.639656061357301020, -10.48075544252181857, -1.200000000000006617 ) ) ;
#5699 = AXIS2_PLACEMENT_3D ( 'NONE', #26558, #26733, #26016 ) ;
#5700 = DIRECTION ( 'NONE',  ( -1.000000000000000000, 0.000000000000000000, 0.000000000000000000 ) ) ;
#5701 = CARTESIAN_POINT ( 'NONE',  ( -39.00000000000000000, -115.9929510916434481, 12.59102132592609102 ) ) ;
#5702 = DIRECTION ( 'NONE',  ( 0.000000000000000000, -1.000000000000000000, 0.000000000000000000 ) ) ;
#5703 = DIRECTION ( 'NONE',  ( -1.000000000000000000, 0.000000000000000000, 0.000000000000000000 ) ) ;
#5704 = DIRECTION ( 'NONE',  ( -1.000000000000000000, 0.000000000000000000, 0.000000000000000000 ) ) ;
#5705 = CARTESIAN_POINT ( 'NONE',  ( 0.000000000000000000, -14.48509162075970202, 8.733917826871310908 ) ) ;
#5706 = DIRECTION ( 'NONE',  ( 0.000000000000000000, 0.000000000000000000, 1.000000000000000000 ) ) ;
#5707 = DIRECTION ( 'NONE',  ( -1.000000000000000000, -0.000000000000000000, -0.000000000000000000 ) ) ;
#5708 = EDGE_LOOP ( 'NONE', ( #10243, #32904 ) ) ;
#5709 = CARTESIAN_POINT ( 'NONE',  ( -38.45611840935523418, -112.6276912846090568, 7.933975545821552622 ) ) ;
#5710 = DIRECTION ( 'NONE',  ( 1.000000000000000000, -4.524158825347490025E-15, -1.174092375852883357E-15 ) ) ;
#5711 = DIRECTION ( 'NONE',  ( -1.000000000000000000, 0.000000000000000000, 0.000000000000000000 ) ) ;
#5712 = EDGE_CURVE ( 'NONE', #6633, #14626, #35084, .T. ) ;
#5713 = DIRECTION ( 'NONE',  ( -1.000000000000000000, 0.000000000000000000, 0.000000000000000000 ) ) ;
#5714 = ORIENTED_EDGE ( 'NONE', *, *, #22916, .T. ) ;
#5715 = EDGE_LOOP ( 'NONE', ( #13468, #17776, #8108, #12400 ) ) ;
#5716 = UNCERTAINTY_MEASURE_WITH_UNIT (LENGTH_MEASURE( 1.000000000000000082E-05 ), #3302, 'distance_accuracy_value', 'NONE');
#5717 = DIRECTION ( 'NONE',  ( -1.000000000000000000, 0.000000000000000000, 0.000000000000000000 ) ) ;
#5718 = CARTESIAN_POINT ( 'NONE',  ( 7.999999999999992895, 0.000000000000000000, 0.000000000000000000 ) ) ;
#5719 = ORIENTED_EDGE ( 'NONE', *, *, #12415, .F. ) ;
#5720 = CIRCLE ( 'NONE', #25851, 17.49900000000001299 ) ;
#5721 = VERTEX_POINT ( 'NONE', #6053 ) ;
#5722 = VECTOR ( 'NONE', #8326, 1000.000000000000000 ) ;
#5723 = EDGE_CURVE ( 'NONE', #25950, #34599, #1451, .T. ) ;
#5724 = DIRECTION ( 'NONE',  ( 0.000000000000000000, 0.000000000000000000, -1.000000000000000000 ) ) ;
#5725 = ADVANCED_FACE ( 'NONE', ( #24968 ), #21901, .T. ) ;
#5726 = CARTESIAN_POINT ( 'NONE',  ( -34.49999999999998579, -17.68172400785659448, 96.37435565298210349 ) ) ;
#5727 = EDGE_CURVE ( 'NONE', #29093, #34324, #27321, .T. ) ;
#5728 = VECTOR ( 'NONE', #31645, 1000.000000000000000 ) ;
#5729 = SHAPE_DEFINITION_REPRESENTATION ( #11789, #26607 ) ;
#5730 = CARTESIAN_POINT ( 'NONE',  ( -0.2142857142857362840, -10.49781318335649161, -1.200000000000006617 ) ) ;
#5731 = ORIENTED_EDGE ( 'NONE', *, *, #28822, .T. ) ;
#5732 = EDGE_LOOP ( 'NONE', ( #13217, #2590, #11522, #16609 ) ) ;
#5733 = LINE ( 'NONE', #13832, #6493 ) ;
#5734 = EDGE_CURVE ( 'NONE', #5280, #19239, #9485, .T. ) ;
#5735 = DIRECTION ( 'NONE',  ( -1.000000000000000000, -0.000000000000000000, -0.000000000000000000 ) ) ;
#5736 = VERTEX_POINT ( 'NONE', #8919 ) ;
#5737 = DIRECTION ( 'NONE',  ( -1.000000000000000000, 0.000000000000000000, 0.000000000000000000 ) ) ;
#5738 = EDGE_CURVE ( 'NONE', #19012, #12683, #8390, .T. ) ;
#5739 = CARTESIAN_POINT ( 'NONE',  ( -34.50000000000000000, -112.0140978167138712, 0.2502176474015765373 ) ) ;
#5740 = CARTESIAN_POINT ( 'NONE',  ( -37.74437085908087397, -114.9929510916434339, 14.09929883582536903 ) ) ;
#5741 = CARTESIAN_POINT ( 'NONE',  ( -38.00000000000000711, -114.9929510916434339, 12.50851088611646311 ) ) ;
#5742 = DIRECTION ( 'NONE',  ( -1.000000000000000000, 0.000000000000000000, -0.000000000000000000 ) ) ;
#5743 = CARTESIAN_POINT ( 'NONE',  ( -36.12500000000014211, -114.9929510916434339, 14.11852480586264846 ) ) ;
#5744 = CARTESIAN_POINT ( 'NONE',  ( 0.000000000000000000, 0.000000000000000000, -40.00000000000000000 ) ) ;
#5745 = ORIENTED_EDGE ( 'NONE', *, *, #17445, .F. ) ;
#5746 = DIRECTION ( 'NONE',  ( -1.000000000000000000, 0.000000000000000000, 0.000000000000000000 ) ) ;
#5747 = DIRECTION ( 'NONE',  ( -1.000000000000000000, -0.000000000000000000, 0.000000000000000000 ) ) ;
#5748 = CIRCLE ( 'NONE', #30479, 7.199999999999992184 ) ;
#5749 = DIRECTION ( 'NONE',  ( -1.000000000000000000, 0.000000000000000000, 0.000000000000000000 ) ) ;
#5750 = CYLINDRICAL_SURFACE ( 'NONE', #16364, 15.49899999999998457 ) ;
#5751 = VERTEX_POINT ( 'NONE', #5875 ) ;
#5752 = CARTESIAN_POINT ( 'NONE',  ( -1.599999999999990319, 0.000000000000000000, 0.000000000000000000 ) ) ;
#5753 = ORIENTED_EDGE ( 'NONE', *, *, #11324, .F. ) ;
#5754 = CYLINDRICAL_SURFACE ( 'NONE', #16417, 4.000000000000000000 ) ;
#5755 = CARTESIAN_POINT ( 'NONE',  ( -35.69809690994938478, -111.0245472910330022, 4.222274454178449155 ) ) ;
#5756 = AXIS2_PLACEMENT_3D ( 'NONE', #15801, #27178, #16334 ) ;
#5757 = DIRECTION ( 'NONE',  ( -1.783119874454246424E-31, -1.187911941725854497E-31, 1.000000000000000000 ) ) ;
#5758 = EDGE_CURVE ( 'NONE', #16380, #11959, #28488, .T. ) ;
#5759 = CARTESIAN_POINT ( 'NONE',  ( -35.50000000000000711, -112.9813730236132585, -1.624774171495860786 ) ) ;
#5760 = ORIENTED_EDGE ( 'NONE', *, *, #32795, .T. ) ;
#5761 = ORIENTED_EDGE ( 'NONE', *, *, #11732, .T. ) ;
#5762 = CARTESIAN_POINT ( 'NONE',  ( 0.000000000000000000, 16.59870953437685515, -3.253005020243678214 ) ) ;
#5763 = PRODUCT_DEFINITION ( 'UNKNOWN', '', #34518, #1307 ) ;
#5764 = LINE ( 'NONE', #22648, #34171 ) ;
#5765 = ORIENTED_EDGE ( 'NONE', *, *, #3783, .F. ) ;
#5766 =( REPRESENTATION_RELATIONSHIP ('NONE','NONE', #26607, #5681 ) REPRESENTATION_RELATIONSHIP_WITH_TRANSFORMATION ( #28163 )SHAPE_REPRESENTATION_RELATIONSHIP( ) );
#5767 = CARTESIAN_POINT ( 'NONE',  ( 7.999999999999992895, 0.000000000000000000, 0.000000000000000000 ) ) ;
#5768 = ADVANCED_FACE ( 'NONE', ( #14318, #33413 ), #19884, .F. ) ;
#5769 = CYLINDRICAL_SURFACE ( 'NONE', #29225, 4.800000000000000711 ) ;
#5770 = ORIENTED_EDGE ( 'NONE', *, *, #12555, .T. ) ;
#5771 = ORIENTED_EDGE ( 'NONE', *, *, #10603, .T. ) ;
#5772 = EDGE_CURVE ( 'NONE', #32244, #10765, #19268, .T. ) ;
#5773 = LINE ( 'NONE', #8280, #6186 ) ;
#5774 = EDGE_CURVE ( 'NONE', #26460, #223, #27846, .T. ) ;
#5775 = DIRECTION ( 'NONE',  ( 0.000000000000000000, 0.000000000000000000, 1.000000000000000000 ) ) ;
#5776 = ORIENTED_EDGE ( 'NONE', *, *, #33278, .F. ) ;
#5777 = ORIENTED_EDGE ( 'NONE', *, *, #9123, .F. ) ;
#5778 = AXIS2_PLACEMENT_3D ( 'NONE', #20107, #1233, #682 ) ;
#5779 = CARTESIAN_POINT ( 'NONE',  ( -34.50000000000000000, -115.0631849411758196, -2.624765990393648885 ) ) ;
#5780 = DIRECTION ( 'NONE',  ( 0.000000000000000000, 0.000000000000000000, -1.000000000000000000 ) ) ;
#5781 = CIRCLE ( 'NONE', #4073, 22.00000000000000000 ) ;
#5782 = VERTEX_POINT ( 'NONE', #3189 ) ;
#5783 = CARTESIAN_POINT ( 'NONE',  ( -36.03906250000000000, -114.9929510916434339, 13.11852480586264669 ) ) ;
#5784 = EDGE_CURVE ( 'NONE', #34725, #3338, #21549, .T. ) ;
#5785 = CARTESIAN_POINT ( 'NONE',  ( -37.18750000000004974, -113.9929510916434339, 14.11852480586265024 ) ) ;
#5786 = CARTESIAN_POINT ( 'NONE',  ( 4.000000000000003553, -5.871425383721172508, -51.66745943012291065 ) ) ;
#5787 = CARTESIAN_POINT ( 'NONE',  ( 55.00000000000000711, -25.98076211353320986, 84.99999999999994316 ) ) ;
#5788 = CARTESIAN_POINT ( 'NONE',  ( -34.50000000000000000, -113.9929510916434339, 12.17846912687782712 ) ) ;
#5789 = CARTESIAN_POINT ( 'NONE',  ( -38.99518666717493431, -114.9929510916434339, 12.74107470552714716 ) ) ;
#5790 = ADVANCED_FACE ( 'NONE', ( #19538 ), #2667, .T. ) ;
#5791 = CARTESIAN_POINT ( 'NONE',  ( -35.50000000000000711, -114.9656200615856818, 10.26631071845107179 ) ) ;
#5792 = PLANE ( 'NONE',  #29704 ) ;
#5793 = CYLINDRICAL_SURFACE ( 'NONE', #18673, 0.6000000000000028644 ) ;
#5794 = EDGE_LOOP ( 'NONE', ( #5590, #17220, #32767, #5753 ) ) ;
#5795 = VERTEX_POINT ( 'NONE', #30719 ) ;
#5796 = AXIS2_PLACEMENT_3D ( 'NONE', #33814, #3573, #22457 ) ;
#5797 = DIRECTION ( 'NONE',  ( -1.000000000000000000, 0.000000000000000000, 0.000000000000000000 ) ) ;
#5798 = DIRECTION ( 'NONE',  ( -1.000000000000000000, 0.000000000000000000, 0.000000000000000000 ) ) ;
#5799 = EDGE_CURVE ( 'NONE', #35019, #17782, #16665, .T. ) ;
#5800 = ORIENTED_EDGE ( 'NONE', *, *, #16313, .T. ) ;
#5801 = CARTESIAN_POINT ( 'NONE',  ( 0.000000000000000000, -37.91532898920900863, -28.61088654061680359 ) ) ;
#5802 = ORIENTED_EDGE ( 'NONE', *, *, #22179, .F. ) ;
#5803 = CARTESIAN_POINT ( 'NONE',  ( -35.50000000000000711, -115.2732872103912030, -1.592823285204062911 ) ) ;
#5804 = CARTESIAN_POINT ( 'NONE',  ( -0.1085714285714300953, -3.798448662927791819, -0.7999999999999951594 ) ) ;
#5805 = EDGE_CURVE ( 'NONE', #27165, #35019, #33584, .T. ) ;
#5806 = CARTESIAN_POINT ( 'NONE',  ( -37.05926240293131713, -115.9999999999999858, 6.378524454178448266 ) ) ;
#5807 = AXIS2_PLACEMENT_3D ( 'NONE', #14992, #23827, #32105 ) ;
#5808 = AXIS2_PLACEMENT_3D ( 'NONE', #23979, #32605, #32429 ) ;
#5809 = DIRECTION ( 'NONE',  ( 0.000000000000000000, -0.4817536741017223734, 0.8763066800438596982 ) ) ;
#5810 = AXIS2_PLACEMENT_3D ( 'NONE', #15793, #29337, #10428 ) ;
#5811 = ORIENTED_EDGE ( 'NONE', *, *, #17321, .T. ) ;
#5812 = CARTESIAN_POINT ( 'NONE',  ( -35.50000000000000711, -113.8159288351371714, 1.978028123174813802 ) ) ;
#5813 = ORIENTED_EDGE ( 'NONE', *, *, #6, .T. ) ;
#5814 = ORIENTED_EDGE ( 'NONE', *, *, #11013, .T. ) ;
#5815 = ADVANCED_FACE ( 'NONE', ( #473, #30380 ), #13629, .F. ) ;
#5816 = CARTESIAN_POINT ( 'NONE',  ( -36.23083527818512550, -116.0245472910329880, 6.284774454178450043 ) ) ;
#5817 = EDGE_CURVE ( 'NONE', #26586, #31687, #11215, .T. ) ;
#5818 = DIRECTION ( 'NONE',  ( -1.000000000000000000, 0.000000000000000000, 0.000000000000000000 ) ) ;
#5819 = ORIENTED_EDGE ( 'NONE', *, *, #17002, .F. ) ;
#5820 = ORIENTED_EDGE ( 'NONE', *, *, #14778, .T. ) ;
#5821 = CARTESIAN_POINT ( 'NONE',  ( -34.50000000000000000, -112.0250551866464548, 1.025914454044489332 ) ) ;
#5822 = DIRECTION ( 'NONE',  ( -0.000000000000000000, 1.000000000000000000, 0.000000000000000000 ) ) ;
#5823 = CARTESIAN_POINT ( 'NONE',  ( 7.999999999999992895, 32.00046193115148441, 34.40241257139697950 ) ) ;
#5824 = CARTESIAN_POINT ( 'NONE',  ( -35.50000000000000000, -113.9929510916434339, 10.50625754673587409 ) ) ;
#5825 = DIRECTION ( 'NONE',  ( 1.000000000000000000, -5.339440136655842133E-16, -1.047965281155519420E-16 ) ) ;
#5826 = CARTESIAN_POINT ( 'NONE',  ( 0.000000000000000000, -0.3151488735047419665, 11.27190672109269798 ) ) ;
#5827 = AXIS2_PLACEMENT_3D ( 'NONE', #22811, #9319, #30749 ) ;
#5828 = PRESENTATION_LAYER_ASSIGNMENT (  '', '', ( #15570 ) ) ;
#5829 = AXIS2_PLACEMENT_3D ( 'NONE', #3973, #20490, #23023 ) ;
#5830 = CARTESIAN_POINT ( 'NONE',  ( -34.50000000000000000, -112.8115600290184801, 2.865251044451027074 ) ) ;
#5831 = CARTESIAN_POINT ( 'NONE',  ( -35.50000000000000000, -114.1928420708668028, 8.515919878418792166 ) ) ;
#5832 = CARTESIAN_POINT ( 'NONE',  ( 3.799999999999999822, -2.710505431213761085E-17, 38.00000000000000711 ) ) ;
#5833 = LINE ( 'NONE', #5663, #4256 ) ;
#5834 = EDGE_LOOP ( 'NONE', ( #83, #8174, #18060, #17881, #19428, #3557, #27030, #14661, #15332, #645, #11844, #25433, #9520, #3768, #25926, #25396, #29295, #26380, #10502, #12097, #7784, #6404, #17993, #9191, #25074, #25842, #18293, #3839, #17278, #218, #19085, #29667, #24452, #9122, #8662, #25459, #17922, #14908, #10889, #14003, #4855, #5377, #13891, #20708, #17972, #15436, #28649, #5102, #24534, #28308, #23877, #3509, #33834, #8304, #32870, #9883, #13435, #29636, #33881, #23171, #6596, #18198, #4266, #9223, #1277, #17526, #9620, #21158, #29937, #3041, #32080, #8834, #34454, #6032, #5082, #24858, #33609, #34458, #22683, #24574, #17508, #12351, #29908, #4455, #13267, #5387, #944, #27115, #24629, #18273, #19815, #19210, #19384, #35113, #29394, #8368, #3256, #18542, #26415, #18897, #12912, #33159, #35057, #535, #29721, #6506, #30243, #20575, #28627, #18994, #23251, #27304, #6548, #25382, #35615, #5969, #16238, #22183, #21341, #13955, #34702, #31664, #26310, #32032, #12551, #24720, #28746, #18712, #17593, #28646, #17707, #380, #26358, #7658, #13516, #22229, #15831, #6313, #29000, #29420, #29998, #9742, #24143, #10685, #24331, #4024, #11201, #795, #12623, #19013, #29103, #16227, #11567, #16176, #1125, #14541, #27531, #18560, #10906, #23330, #30593, #5941, #25210, #15527, #31492, #2221, #29914, #3257, #13743, #6108, #27158, #22754, #27550, #14903, #28633, #7165, #22276, #24549, #24157, #22357, #28628, #15370, #3439, #32695, #10803, #16311, #24636, #11350, #27689, #2278, #12387, #3088, #12002, #25888, #12584, #22539, #25201, #17725, #21880, #28815, #26299, #12682, #5643 ) ) ;
#5835 = CARTESIAN_POINT ( 'NONE',  ( 8.000000000000000000, 17.47118961583601759, -0.9861715913088253682 ) ) ;
#5836 = CARTESIAN_POINT ( 'NONE',  ( 8.000000000000000000, 14.71414642875954648, 9.471478019455206621 ) ) ;
#5837 = CARTESIAN_POINT ( 'NONE',  ( -39.49999999999999289, -1.387778780781445676E-14, 110.0000000000000000 ) ) ;
#5838 = EDGE_CURVE ( 'NONE', #5458, #4835, #2032, .T. ) ;
#5839 = VERTEX_POINT ( 'NONE', #12337 ) ;
#5840 = DIRECTION ( 'NONE',  ( 0.000000000000000000, 0.000000000000000000, -1.000000000000000000 ) ) ;
#5841 = DIRECTION ( 'NONE',  ( 0.000000000000000000, 0.000000000000000000, 1.000000000000000000 ) ) ;
#5842 = EDGE_CURVE ( 'NONE', #6291, #21409, #31338, .T. ) ;
#5843 = CYLINDRICAL_SURFACE ( 'NONE', #21097, 52.00000000000000711 ) ;
#5844 = LINE ( 'NONE', #5674, #13272 ) ;
#5845 = VECTOR ( 'NONE', #35076, 1000.000000000000000 ) ;
#5846 = ITEM_DEFINED_TRANSFORMATION ( 'NONE', 'NONE', #2947,  #21307 ) ;
#5847 = DIRECTION ( 'NONE',  ( -1.000000000000000000, 0.000000000000000000, 0.000000000000000000 ) ) ;
#5848 = CARTESIAN_POINT ( 'NONE',  ( 0.000000000000000000, 0.000000000000000000, 0.000000000000000000 ) ) ;
#5849 = ORIENTED_EDGE ( 'NONE', *, *, #14083, .T. ) ;
#5850 = DIRECTION ( 'NONE',  ( 0.000000000000000000, 0.000000000000000000, -1.000000000000000000 ) ) ;
#5851 = CYLINDRICAL_SURFACE ( 'NONE', #2505, 19.99999999999998579 ) ;
#5852 = ORIENTED_EDGE ( 'NONE', *, *, #25069, .T. ) ;
#5853 = CARTESIAN_POINT ( 'NONE',  ( -36.02454729103297382, -113.5265240346956261, 3.902725545821552178 ) ) ;
#5854 = VERTEX_POINT ( 'NONE', #17912 ) ;
#5855 = AXIS2_PLACEMENT_3D ( 'NONE', #30451, #16739, #14041 ) ;
#5856 = PRESENTATION_LAYER_ASSIGNMENT (  '', '', ( #32872 ) ) ;
#5857 = CIRCLE ( 'NONE', #13895, 8.000000000000007105 ) ;
#5858 = EDGE_LOOP ( 'NONE', ( #30808, #17885, #18933, #1750 ) ) ;
#5859 = ORIENTED_EDGE ( 'NONE', *, *, #18675, .T. ) ;
#5860 = DIRECTION ( 'NONE',  ( 0.000000000000000000, 0.9980267284282717810, -0.06279051952930997382 ) ) ;
#5861 = CARTESIAN_POINT ( 'NONE',  ( -35.50000000000000711, -116.0140978167138712, -0.5622823525984409487 ) ) ;
#5862 = CARTESIAN_POINT ( 'NONE',  ( 8.000000000000000000, -12.49559743815772528, -9.169462670380713831 ) ) ;
#5863 = TOROIDAL_SURFACE ( 'NONE', #27796, 7.800000000000023803, 0.1999999999999992339 ) ;
#5864 = CARTESIAN_POINT ( 'NONE',  ( -35.50000000000000711, -114.9902084924877954, 10.43071793783961176 ) ) ;
#5865 = DIRECTION ( 'NONE',  ( 0.000000000000000000, -0.1253332335642904638, -0.9921147013144796523 ) ) ;
#5866 = DIRECTION ( 'NONE',  ( -1.174092375852890260E-15, 4.222049128630259891E-16, 1.000000000000000000 ) ) ;
#5867 = CARTESIAN_POINT ( 'NONE',  ( -34.50000000000000000, -114.5636144531578680, 9.676196722963288366 ) ) ;
#5868 = CARTESIAN_POINT ( 'NONE',  ( 0.000000000000000000, 0.000000000000000000, 49.10000000000000142 ) ) ;
#5869 = DIRECTION ( 'NONE',  ( 1.000000000000000000, -0.000000000000000000, -0.000000000000000000 ) ) ;
#5870 = CARTESIAN_POINT ( 'NONE',  ( -37.49023442168701337, -115.9929510916434481, 14.11852773550420359 ) ) ;
#5872 = FACE_OUTER_BOUND ( 'NONE', #11812, .T. ) ;
#5871 = AXIS2_PLACEMENT_3D ( 'NONE', #19524, #27302, #22064 ) ;
#5873 = CYLINDRICAL_SURFACE ( 'NONE', #18776, 4.000000000000000000 ) ;
#5874 = DIRECTION ( 'NONE',  ( 0.000000000000000000, -0.7705132427757817037, -0.6374239897486988493 ) ) ;
#5875 = CARTESIAN_POINT ( 'NONE',  ( 7.999999999999992895, 3.840921266750509488, -47.34345070675166767 ) ) ;
#5876 = ADVANCED_FACE ( 'NONE', ( #31251 ), #14858, .F. ) ;
#5877 = DIRECTION ( 'NONE',  ( 0.000000000000000000, -0.3681245526846653737, -0.9297764858882564543 ) ) ;
#5878 = DIRECTION ( 'NONE',  ( 1.000000000000000000, -5.339440136655842133E-16, -1.047965281155519420E-16 ) ) ;
#5879 = ORIENTED_EDGE ( 'NONE', *, *, #18479, .T. ) ;
#5880 = CARTESIAN_POINT ( 'NONE',  ( -36.11231047232249125, -115.9754527089670262, 8.777725545821555286 ) ) ;
#5881 = DIRECTION ( 'NONE',  ( 0.000000000000000000, 0.000000000000000000, -1.000000000000000000 ) ) ;
#5882 = PLANE ( 'NONE',  #28566 ) ;
#5883 = DIRECTION ( 'NONE',  ( -1.000000000000000000, 0.000000000000000000, 0.000000000000000000 ) ) ;
#5884 = VERTEX_POINT ( 'NONE', #31429 ) ;
#5885 = MECHANICAL_DESIGN_GEOMETRIC_PRESENTATION_REPRESENTATION (  '', ( #8745 ), #32334 ) ;
#5886 = VERTEX_POINT ( 'NONE', #33957 ) ;
#5887 = DIRECTION ( 'NONE',  ( -1.000000000000000000, 0.000000000000000000, 0.000000000000000000 ) ) ;
#5888 = CARTESIAN_POINT ( 'NONE',  ( -42.49999999999999289, -14.67619866229204284, 93.25874355921412473 ) ) ;
#5889 = ORIENTED_EDGE ( 'NONE', *, *, #24415, .T. ) ;
#5890 = CIRCLE ( 'NONE', #4188, 4.872650870659778199 ) ;
#5891 = EDGE_CURVE ( 'NONE', #21028, #35157, #12971, .T. ) ;
#5892 = EDGE_LOOP ( 'NONE', ( #19435, #22716, #25356, #12042 ) ) ;
#5893 = DIRECTION ( 'NONE',  ( 0.000000000000000000, 0.5000000000000012212, -0.8660254037844380415 ) ) ;
#5894 = CIRCLE ( 'NONE', #28930, 17.49900000000001654 ) ;
#5895 = DIRECTION ( 'NONE',  ( -1.000000000000000000, 0.000000000000000000, 0.000000000000000000 ) ) ;
#5896 = VECTOR ( 'NONE', #12868, 1000.000000000000000 ) ;
#5897 = SHAPE_DEFINITION_REPRESENTATION ( #15253, #30285 ) ;
#5898 = DIRECTION ( 'NONE',  ( -1.000000000000000000, -0.000000000000000000, -0.000000000000000000 ) ) ;
#5899 = EDGE_LOOP ( 'NONE', ( #19959, #4466, #24029, #2272 ) ) ;
#5900 = ORIENTED_EDGE ( 'NONE', *, *, #34888, .F. ) ;
#5901 = FACE_OUTER_BOUND ( 'NONE', #2583, .T. ) ;
#5902 = DIRECTION ( 'NONE',  ( 0.000000000000000000, -1.000000000000000000, -1.611597878369477150E-16 ) ) ;
#5903 = VERTEX_POINT ( 'NONE', #17734 ) ;
#5904 = CARTESIAN_POINT ( 'NONE',  ( -50.00000000000000000, 0.000000000000000000, 0.000000000000000000 ) ) ;
#5905 = AXIS2_PLACEMENT_3D ( 'NONE', #5105, #10852, #16398 ) ;
#5906 = CARTESIAN_POINT ( 'NONE',  ( -34.50000000000000000, -116.0140978167138712, 0.0002176474015577116276 ) ) ;
#5907 = UNCERTAINTY_MEASURE_WITH_UNIT (LENGTH_MEASURE( 1.000000000000000082E-05 ), #19257, 'distance_accuracy_value', 'NONE');
#5908 = AXIS2_PLACEMENT_3D ( 'NONE', #14310, #25313, #34304 ) ;
#5909 = CARTESIAN_POINT ( 'NONE',  ( -34.50000000000000000, -115.9929524668003182, 10.51038305125561401 ) ) ;
#5910 = CARTESIAN_POINT ( 'NONE',  ( -38.50000000000000711, -114.9929510916434339, 10.50625754673587231 ) ) ;
#5911 = FACE_OUTER_BOUND ( 'NONE', #7615, .T. ) ;
#5912 = CARTESIAN_POINT ( 'NONE',  ( -34.49999793727135255, -114.9929510916434339, 12.61164896875036590 ) ) ;
#5913 = DIRECTION ( 'NONE',  ( -1.000000000000000000, 0.000000000000000000, 0.000000000000000000 ) ) ;
#5914 = DIRECTION ( 'NONE',  ( -1.783119874454246424E-31, -1.187911941725854497E-31, 1.000000000000000000 ) ) ;
#5915 = FACE_OUTER_BOUND ( 'NONE', #1124, .T. ) ;
#5916 = CARTESIAN_POINT ( 'NONE',  ( 0.000000000000000000, -3.975523202427916125, -13.42368113696676346 ) ) ;
#5917 = CARTESIAN_POINT ( 'NONE',  ( 55.00000000000000000, -2.726571689596996976E-14, 114.0000000000000000 ) ) ;
#5918 = VECTOR ( 'NONE', #21678, 1000.000000000000000 ) ;
#5919 = EDGE_CURVE ( 'NONE', #12842, #23201, #6045, .T. ) ;
#5920 = ORIENTED_EDGE ( 'NONE', *, *, #30074, .T. ) ;
#5921 = AXIS2_PLACEMENT_3D ( 'NONE', #6133, #21976, #13882 ) ;
#5922 = ADVANCED_FACE ( 'NONE', ( #14489 ), #15029, .T. ) ;
#5923 = CARTESIAN_POINT ( 'NONE',  ( 0.000000000000000000, 6.109652351741788223, 46.58570277113510372 ) ) ;
#5924 = ORIENTED_EDGE ( 'NONE', *, *, #14525, .T. ) ;
#5925 = CARTESIAN_POINT ( 'NONE',  ( -35.81662171581204746, -117.0245472910329738, 3.284774454178449155 ) ) ;
#5926 = DIRECTION ( 'NONE',  ( 1.112002228190253556E-16, -6.938893903907203726E-17, -1.000000000000000000 ) ) ;
#5927 = CARTESIAN_POINT ( 'NONE',  ( -35.50000000000000711, -112.0140978167138712, -0.3747823525984256832 ) ) ;
#5928 = ORIENTED_EDGE ( 'NONE', *, *, #8757, .T. ) ;
#5929 = ORIENTED_EDGE ( 'NONE', *, *, #17902, .T. ) ;
#5930 = DIRECTION ( 'NONE',  ( 0.02857142857142376188, 0.9995917534020517525, 3.884870526907702485E-16 ) ) ;
#5931 = DIRECTION ( 'NONE',  ( 0.000000000000000000, 0.000000000000000000, -1.000000000000000000 ) ) ;
#5932 = EDGE_CURVE ( 'NONE', #4250, #28091, #26174, .T. ) ;
#5933 = ORIENTED_EDGE ( 'NONE', *, *, #31405, .F. ) ;
#5934 = EDGE_CURVE ( 'NONE', #26106, #11426, #34221, .T. ) ;
#5935 = CIRCLE ( 'NONE', #19702, 19.99999999999998579 ) ;
#5936 = CIRCLE ( 'NONE', #10542, 8.000000000000001776 ) ;
#5937 = DIRECTION ( 'NONE',  ( 0.000000000000000000, 0.000000000000000000, -1.000000000000000000 ) ) ;
#5938 = DIRECTION ( 'NONE',  ( 0.000000000000000000, 0.000000000000000000, 1.000000000000000000 ) ) ;
#5940 = ORIENTED_EDGE ( 'NONE', *, *, #28004, .F. ) ;
#5939 = AXIS2_PLACEMENT_3D ( 'NONE', #33953, #8915, #34129 ) ;
#5941 = ORIENTED_EDGE ( 'NONE', *, *, #4051, .F. ) ;
#5942 = CARTESIAN_POINT ( 'NONE',  ( 7.999999999999992895, 0.000000000000000000, 0.000000000000000000 ) ) ;
#5943 = DIRECTION ( 'NONE',  ( -0.000000000000000000, 0.000000000000000000, -1.000000000000000000 ) ) ;
#5944 = EDGE_LOOP ( 'NONE', ( #18134, #30778, #21079, #31987 ) ) ;
#5945 = ORIENTED_EDGE ( 'NONE', *, *, #26127, .T. ) ;
#5946 = CARTESIAN_POINT ( 'NONE',  ( -35.50000000000000000, -111.3577635893106361, 2.022004269840791402 ) ) ;
#5947 = AXIS2_PLACEMENT_3D ( 'NONE', #9413, #20739, #34629 ) ;
#5948 = CIRCLE ( 'NONE', #12845, 20.00000000000000711 ) ;
#5949 = AXIS2_PLACEMENT_3D ( 'NONE', #31749, #15706, #20751 ) ;
#5950 = ORIENTED_EDGE ( 'NONE', *, *, #18733, .F. ) ;
#5951 = CARTESIAN_POINT ( 'NONE',  ( -35.50400759022159036, -114.9929510916434339, 12.68378527132497524 ) ) ;
#5952 = EDGE_CURVE ( 'NONE', #14078, #1924, #10657, .T. ) ;
#5953 = CARTESIAN_POINT ( 'NONE',  ( -34.50000000000000000, -113.9929510916434339, 12.50851088611648265 ) ) ;
#5954 = LINE ( 'NONE', #25404, #447 ) ;
#5955 = CARTESIAN_POINT ( 'NONE',  ( 8.000000000000000000, -3.678165988948487009, -15.05623113391071044 ) ) ;
#5956 = CARTESIAN_POINT ( 'NONE',  ( -34.50000000000000000, -113.9929510916436470, 10.50625754673581724 ) ) ;
#5957 = LINE ( 'NONE', #27922, #3312 ) ;
#5958 = CARTESIAN_POINT ( 'NONE',  ( -35.50000000000000711, -114.0743172650041686, 9.508870970061893857 ) ) ;
#5959 = FILL_AREA_STYLE ('',( #30284 ) ) ;
#5960 = CIRCLE ( 'NONE', #12286, 8.000000000000007105 ) ;
#5961 = CYLINDRICAL_SURFACE ( 'NONE', #3757, 20.00000000000000355 ) ;
#5962 = EDGE_CURVE ( 'NONE', #21809, #12683, #34496, .T. ) ;
#5963 = VERTEX_POINT ( 'NONE', #11798 ) ;
#5964 = EDGE_CURVE ( 'NONE', #10090, #24945, #4343, .T. ) ;
#5965 = EDGE_LOOP ( 'NONE', ( #27239, #30604, #8467, #7486 ) ) ;
#5966 = ADVANCED_FACE ( 'NONE', ( #17370 ), #1016, .T. ) ;
#5967 = CARTESIAN_POINT ( 'NONE',  ( -90.00000000000002842, 1.534828951630468922E-15, 8.000000000000058620 ) ) ;
#5968 = CYLINDRICAL_SURFACE ( 'NONE', #31821, 11.00000000000000000 ) ;
#5969 = ORIENTED_EDGE ( 'NONE', *, *, #8709, .F. ) ;
#5970 = CARTESIAN_POINT ( 'NONE',  ( 8.000000000000000000, -13.24207120356975587, 14.98824707027438130 ) ) ;
#5971 = ORIENTED_EDGE ( 'NONE', *, *, #4271, .F. ) ;
#5972 = CIRCLE ( 'NONE', #24952, 14.00000000000000000 ) ;
#5973 = CIRCLE ( 'NONE', #5423, 14.00000000000000000 ) ;
#5974 = CARTESIAN_POINT ( 'NONE',  ( -35.50000000000000000, -114.9932644833805426, -0.6247823525982824089 ) ) ;
#5975 = CARTESIAN_POINT ( 'NONE',  ( 8.000000000000000000, 19.77827456857338007, -2.969824084036535528 ) ) ;
#5976 = CARTESIAN_POINT ( 'NONE',  ( -34.97545270896703329, -113.2308352781851539, 2.909774454178448710 ) ) ;
#5977 = EDGE_CURVE ( 'NONE', #25395, #13426, #33642, .T. ) ;
#5978 = ORIENTED_EDGE ( 'NONE', *, *, #10678, .T. ) ;
#5979 = LINE ( 'NONE', #30476, #18798 ) ;
#5980 = ADVANCED_FACE ( 'NONE', ( #9285 ), #28555, .T. ) ;
#5981 = ORIENTED_EDGE ( 'NONE', *, *, #15173, .T. ) ;
#5982 = FACE_OUTER_BOUND ( 'NONE', #23235, .T. ) ;
#5983 = CARTESIAN_POINT ( 'NONE',  ( -35.50000000000000000, -114.8057644833805853, -2.624782352598442614 ) ) ;
#5984 = VERTEX_POINT ( 'NONE', #26033 ) ;
#5985 = ORIENTED_EDGE ( 'NONE', *, *, #14960, .F. ) ;
#5986 = LINE ( 'NONE', #27948, #19926 ) ;
#5987 = CARTESIAN_POINT ( 'NONE',  ( 39.30000000000000426, 7.219292880973646134E-15, 0.000000000000000000 ) ) ;
#5989 = ORIENTED_EDGE ( 'NONE', *, *, #28611, .F. ) ;
#5988 = AXIS2_PLACEMENT_3D ( 'NONE', #17689, #25986, #20191 ) ;
#5990 = ORIENTED_EDGE ( 'NONE', *, *, #1378, .F. ) ;
#5991 = CARTESIAN_POINT ( 'NONE',  ( -34.50000000000000000, -112.0141053790792114, 0.9054673897245171243 ) ) ;
#5992 = DIRECTION ( 'NONE',  ( -1.000000000000000000, 0.000000000000000000, 0.000000000000000000 ) ) ;
#5993 = ORIENTED_EDGE ( 'NONE', *, *, #2408, .F. ) ;
#5994 = CYLINDRICAL_SURFACE ( 'NONE', #14904, 47.49900000000001654 ) ;
#5995 = ADVANCED_FACE ( 'NONE', ( #816 ), #25868, .T. ) ;
#5996 = CIRCLE ( 'NONE', #22653, 20.00000000000000711 ) ;
#5997 = CARTESIAN_POINT ( 'NONE',  ( -35.50640865667917723, -113.9929510916434339, 12.69998175888958691 ) ) ;
#5998 = AXIS2_PLACEMENT_3D ( 'NONE', #20151, #5140, #16079 ) ;
#5999 = EDGE_CURVE ( 'NONE', #29381, #19471, #27339, .T. ) ;
#6000 = DIRECTION ( 'NONE',  ( 0.000000000000000000, -0.8660254037844368202, -0.5000000000000031086 ) ) ;
#6001 = DIRECTION ( 'NONE',  ( -1.000000000000000000, 0.000000000000000000, 0.000000000000000000 ) ) ;
#6002 = ADVANCED_FACE ( 'NONE', ( #6231, #22779 ), #7114, .T. ) ;
#6003 = CARTESIAN_POINT ( 'NONE',  ( -34.50000000000000000, -113.8814751941374652, 2.992951091643117678 ) ) ;
#6004 = CARTESIAN_POINT ( 'NONE',  ( -35.50000000000000000, -114.2675000158779710, 8.525177020294046670 ) ) ;
#6005 = DIRECTION ( 'NONE',  ( -1.000000000000000000, -0.000000000000000000, 0.000000000000000000 ) ) ;
#6006 = CYLINDRICAL_SURFACE ( 'NONE', #31275, 8.000000000000001776 ) ;
#6007 = EDGE_CURVE ( 'NONE', #15607, #19637, #20404, .T. ) ;
#6008 = ORIENTED_EDGE ( 'NONE', *, *, #14512, .F. ) ;
#6009 = DIRECTION ( 'NONE',  ( 0.000000000000000000, 0.000000000000000000, 1.000000000000000000 ) ) ;
#6010 = CARTESIAN_POINT ( 'NONE',  ( 2.321707774797385326, -4.824281976788927118, -0.7999999999999951594 ) ) ;
#6011 = EDGE_CURVE ( 'NONE', #4002, #26625, #10108, .T. ) ;
#6012 = CARTESIAN_POINT ( 'NONE',  ( 0.000000000000000000, -1.000000000000001554, 38.00000000000000000 ) ) ;
#6013 = ORIENTED_EDGE ( 'NONE', *, *, #14923, .F. ) ;
#6014 = DIRECTION ( 'NONE',  ( 0.000000000000000000, 0.000000000000000000, 1.000000000000000000 ) ) ;
#6015 = CARTESIAN_POINT ( 'NONE',  ( -50.00000000000000000, -25.98076211353320275, 73.99999999999992895 ) ) ;
#6016 = DIRECTION ( 'NONE',  ( -1.000000000000000000, 0.000000000000000000, 0.000000000000000000 ) ) ;
#6017 = DIRECTION ( 'NONE',  ( -1.000000000000000000, 0.000000000000000000, 0.000000000000000000 ) ) ;
#6018 = CONTEXT_DEPENDENT_SHAPE_REPRESENTATION ( #26012, #6929 ) ;
#6019 = CARTESIAN_POINT ( 'NONE',  ( 7.999999999999992895, 14.30000000000000071, 3.000000000000002665 ) ) ;
#6020 = LINE ( 'NONE', #33382, #33730 ) ;
#6021 = EDGE_CURVE ( 'NONE', #34112, #7789, #23304, .T. ) ;
#6022 = ORIENTED_EDGE ( 'NONE', *, *, #14553, .F. ) ;
#6023 = VECTOR ( 'NONE', #31614, 1000.000000000000000 ) ;
#6024 = DIRECTION ( 'NONE',  ( 1.174092375852890260E-15, -4.222049128630259891E-16, -1.000000000000000000 ) ) ;
#6025 = CARTESIAN_POINT ( 'NONE',  ( 55.00000000000000711, -25.98076211353320986, 80.99999999999992895 ) ) ;
#6026 = CARTESIAN_POINT ( 'NONE',  ( 2.000000000000001776, 0.000000000000000000, 0.000000000000000000 ) ) ;
#6027 = ORIENTED_EDGE ( 'NONE', *, *, #4850, .T. ) ;
#6028 = CARTESIAN_POINT ( 'NONE',  ( -35.97545270896705460, -114.3549511594417680, 4.090225545821551734 ) ) ;
#6029 = ORIENTED_EDGE ( 'NONE', *, *, #16523, .T. ) ;
#6030 = AXIS2_PLACEMENT_3D ( 'NONE', #12391, #23193, #6452 ) ;
#6031 = VERTEX_POINT ( 'NONE', #15921 ) ;
#6032 = ORIENTED_EDGE ( 'NONE', *, *, #3653, .F. ) ;
#6033 = FACE_OUTER_BOUND ( 'NONE', #12968, .T. ) ;
#6034 = CARTESIAN_POINT ( 'NONE',  ( -35.50000000000000711, -116.0140978167138712, 0.8752176474015622709 ) ) ;
#6035 = EDGE_CURVE ( 'NONE', #20546, #26137, #26573, .T. ) ;
#6036 = CARTESIAN_POINT ( 'NONE',  ( -1.799999999999996048, 0.000000000000000000, 0.000000000000000000 ) ) ;
#6037 = CIRCLE ( 'NONE', #33084, 7.200000000000000178 ) ;
#6038 = ADVANCED_FACE ( 'NONE', ( #9997 ), #4966, .T. ) ;
#6039 = CARTESIAN_POINT ( 'NONE',  ( -35.50000000000000711, -114.9860996047076895, 10.38555023491505835 ) ) ;
#6040 = FACE_BOUND ( 'NONE', #4646, .T. ) ;
#6041 = DIRECTION ( 'NONE',  ( 0.000000000000000000, 0.000000000000000000, 1.000000000000000000 ) ) ;
#6042 = CARTESIAN_POINT ( 'NONE',  ( -34.50000000000000000, -114.9929510916434339, 10.53376102667243508 ) ) ;
#6043 = CARTESIAN_POINT ( 'NONE',  ( 0.000000000000000000, 14.71414642875953938, 9.471478019455203068 ) ) ;
#6044 = CLOSED_SHELL ( 'NONE', ( #31093, #345, #11165, #5876, #2882, #5301, #31535, #1328, #13097, #434, #30007, #33069, #10334, #20487, #27405, #19750, #19706, #9581, #492, #35008, #17406, #7272, #29548, #4888, #24247, #3355 ) ) ;
#6045 = CIRCLE ( 'NONE', #25021, 22.00000000000000000 ) ;
#6046 = FACE_BOUND ( 'NONE', #24144, .T. ) ;
#6047 = CARTESIAN_POINT ( 'NONE',  ( -35.50000000000000000, -115.9929510916434481, 10.51175824272318415 ) ) ;
#6048 = CARTESIAN_POINT ( 'NONE',  ( -35.50000000000000711, -112.0140978167138712, 0.2502176474015765373 ) ) ;
#6049 = CYLINDRICAL_SURFACE ( 'NONE', #106, 4.000000000000003553 ) ;
#6050 = VECTOR ( 'NONE', #30202, 1000.000000000000000 ) ;
#6051 = PLANE ( 'NONE',  #33149 ) ;
#6052 = DIRECTION ( 'NONE',  ( 1.541976423090495387E-16, -1.000000000000000000, 0.000000000000000000 ) ) ;
#6053 = CARTESIAN_POINT ( 'NONE',  ( 0.000000000000000000, -46.21320724403657465, 10.97699764141937884 ) ) ;
#6054 = CIRCLE ( 'NONE', #12374, 0.2000000000000003164 ) ;
#6055 = CARTESIAN_POINT ( 'NONE',  ( -55.00000000000000000, 10.00000000000000888, 110.0000000000000000 ) ) ;
#6056 = CARTESIAN_POINT ( 'NONE',  ( 4.000000000000003553, 10.46102064772367868, -19.35373470438974053 ) ) ;
#6057 = ORIENTED_EDGE ( 'NONE', *, *, #154, .T. ) ;
#6058 = CARTESIAN_POINT ( 'NONE',  ( -38.02454729103295961, -113.6450488405582462, 3.340225545821551290 ) ) ;
#6059 = DIRECTION ( 'NONE',  ( -0.000000000000000000, 0.000000000000000000, -1.000000000000000000 ) ) ;
#6060 = DIRECTION ( 'NONE',  ( 1.000000000000000000, -4.524158825347490025E-15, -1.169797080839617330E-15 ) ) ;
#6061 = DIRECTION ( 'NONE',  ( 0.000000000000000000, 0.000000000000000000, 1.000000000000000000 ) ) ;
#6062 = ORIENTED_EDGE ( 'NONE', *, *, #724, .T. ) ;
#6063 = AXIS2_PLACEMENT_3D ( 'NONE', #6140, #4166, #11888 ) ;
#6064 = ORIENTED_EDGE ( 'NONE', *, *, #19613, .F. ) ;
#6065 = UNCERTAINTY_MEASURE_WITH_UNIT (LENGTH_MEASURE( 1.000000000000000082E-05 ), #29911, 'distance_accuracy_value', 'NONE');
#6066 = DIRECTION ( 'NONE',  ( -1.000000000000000000, 0.000000000000000000, -0.000000000000000000 ) ) ;
#6067 = CARTESIAN_POINT ( 'NONE',  ( 0.000000000000000000, -8.053585752062238257, 46.81126742072021329 ) ) ;
#6068 = ORIENTED_EDGE ( 'NONE', *, *, #1614, .T. ) ;
#6069 = EDGE_LOOP ( 'NONE', ( #22792, #11645, #3433, #14289 ) ) ;
#6070 = DIRECTION ( 'NONE',  ( 1.000000000000000000, 1.734723475976807094E-16, 0.000000000000000000 ) ) ;
#6071 = CARTESIAN_POINT ( 'NONE',  ( 0.000000000000000000, 0.000000000000000000, -1.200000000000006617 ) ) ;
#6072 = SHAPE_DEFINITION_REPRESENTATION ( #23625, #18063 ) ;
#6073 = VECTOR ( 'NONE', #22215, 1000.000000000000000 ) ;
#6074 = DIRECTION ( 'NONE',  ( 0.000000000000000000, 0.000000000000000000, 1.000000000000000000 ) ) ;
#6075 = ORIENTED_EDGE ( 'NONE', *, *, #22614, .T. ) ;
#6076 = EDGE_LOOP ( 'NONE', ( #9789, #27808 ) ) ;
#6077 = AXIS2_PLACEMENT_3D ( 'NONE', #6163, #17128, #402 ) ;
#6078 = ADVANCED_FACE ( 'NONE', ( #10181 ), #15555, .T. ) ;
#6079 = FACE_OUTER_BOUND ( 'NONE', #30683, .T. ) ;
#6080 = DIRECTION ( 'NONE',  ( 0.000000000000000000, 1.611597878369477150E-16, -1.000000000000000000 ) ) ;
#6081 = ORIENTED_EDGE ( 'NONE', *, *, #19863, .T. ) ;
#6082 = LINE ( 'NONE', #33445, #8029 ) ;
#6083 = AXIS2_PLACEMENT_3D ( 'NONE', #33457, #22635, #20109 ) ;
#6084 = CARTESIAN_POINT ( 'NONE',  ( -34.50000000000000000, -115.0140978167138712, 0.6252176474015650465 ) ) ;
#6085 = LINE ( 'NONE', #31281, #34598 ) ;
#6086 = CARTESIAN_POINT ( 'NONE',  ( 46.00000000000000000, -25.98076211353320275, 84.99999999999992895 ) ) ;
#6087 = CARTESIAN_POINT ( 'NONE',  ( -34.50000000000000000, -114.1371041221139109, 8.509266650872710613 ) ) ;
#6088 = DIRECTION ( 'NONE',  ( 0.9997917317482359900, -0.02040816326530624225, -1.905159032394999552E-31 ) ) ;
#6089 = DIRECTION ( 'NONE',  ( -1.734723475976807094E-16, -2.423959199780483078E-15, 1.000000000000000000 ) ) ;
#6090 = CARTESIAN_POINT ( 'NONE',  ( -39.00000206272865455, -114.9929510916434339, 12.61164896875035701 ) ) ;
#6091 = DIRECTION ( 'NONE',  ( 0.000000000000000000, 0.000000000000000000, 1.000000000000000000 ) ) ;
#6092 = LINE ( 'NONE', #12747, #20705 ) ;
#6093 = CARTESIAN_POINT ( 'NONE',  ( 7.999999999999992895, 32.00046193115196758, -34.40241257139653186 ) ) ;
#6094 = DIRECTION ( 'NONE',  ( -1.000000000000000000, 0.000000000000000000, 0.000000000000000000 ) ) ;
#6095 = AXIS2_PLACEMENT_3D ( 'NONE', #10319, #10493, #15694 ) ;
#6096 = ORIENTED_EDGE ( 'NONE', *, *, #27645, .T. ) ;
#6097 = DIRECTION ( 'NONE',  ( -1.000000000000000000, 0.000000000000000000, 0.000000000000000000 ) ) ;
#6098 = ORIENTED_EDGE ( 'NONE', *, *, #15711, .T. ) ;
#6099 = CARTESIAN_POINT ( 'NONE',  ( -34.83677480945819838, -111.9205845034225462, 4.316024454178448266 ) ) ;
#6100 = CARTESIAN_POINT ( 'NONE',  ( 0.000000000000000000, 13.60411018104320036, 12.96676809804154118 ) ) ;
#6101 = AXIS2_PLACEMENT_3D ( 'NONE', #34463, #28871, #4223 ) ;
#6102 = CARTESIAN_POINT ( 'NONE',  ( -35.50000000000000711, -112.0140978167138712, 0.2502176474015765373 ) ) ;
#6103 = ORIENTED_EDGE ( 'NONE', *, *, #1104, .T. ) ;
#6104 = ORIENTED_EDGE ( 'NONE', *, *, #5734, .T. ) ;
#6105 = CIRCLE ( 'NONE', #3242, 7.199999999999992184 ) ;
#6106 = CARTESIAN_POINT ( 'NONE',  ( 7.999999999999992895, -3.840921266749481422, -47.34345070675177425 ) ) ;
#6107 = LINE ( 'NONE', #33304, #16871 ) ;
#6108 = ORIENTED_EDGE ( 'NONE', *, *, #23790, .F. ) ;
#6109 = AXIS2_PLACEMENT_3D ( 'NONE', #4053, #981, #17703 ) ;
#6110 = DIRECTION ( 'NONE',  ( 0.000000000000000000, 0.000000000000000000, 1.000000000000000000 ) ) ;
#6111 = DIRECTION ( 'NONE',  ( 0.000000000000000000, 0.000000000000000000, 1.000000000000000000 ) ) ;
#6112 = VERTEX_POINT ( 'NONE', #13250 ) ;
#6113 = VERTEX_POINT ( 'NONE', #4621 ) ;
#6114 = CARTESIAN_POINT ( 'NONE',  ( 27.00000000000000355, 45.00000000000000711, 5.510910596163087978E-15 ) ) ;
#6115 = DIRECTION ( 'NONE',  ( 0.000000000000000000, 0.000000000000000000, -1.000000000000000000 ) ) ;
#6116 = AXIS2_PLACEMENT_3D ( 'NONE', #7192, #5230, #32752 ) ;
#6117 = ORIENTED_EDGE ( 'NONE', *, *, #878, .T. ) ;
#6118 = ORIENTED_EDGE ( 'NONE', *, *, #29358, .T. ) ;
#6119 = CARTESIAN_POINT ( 'NONE',  ( -35.50000000000000000, -111.0141129414446652, 0.9205922128478062350 ) ) ;
#6120 = ADVANCED_FACE ( 'NONE', ( #18811 ), #15735, .T. ) ;
#6121 = PRODUCT_DEFINITION_SHAPE ( 'NONE', 'NONE',  #35645 ) ;
#6122 = CIRCLE ( 'NONE', #30295, 47.49900000000002365 ) ;
#6123 = EDGE_CURVE ( 'NONE', #29440, #10721, #2446, .T. ) ;
#6124 = CYLINDRICAL_SURFACE ( 'NONE', #3948, 52.00000000000000711 ) ;
#6125 = ORIENTED_EDGE ( 'NONE', *, *, #8140, .T. ) ;
#6126 = CARTESIAN_POINT ( 'NONE',  ( -35.97955704204053262, -114.9929510916434339, 13.11812344617474579 ) ) ;
#6127 = MECHANICAL_DESIGN_GEOMETRIC_PRESENTATION_REPRESENTATION (  '', ( #20502 ), #12480 ) ;
#6128 = VECTOR ( 'NONE', #33076, 1000.000000000000114 ) ;
#6129 = AXIS2_PLACEMENT_3D ( 'NONE', #1325, #26357, #7077 ) ;
#6130 = CARTESIAN_POINT ( 'NONE',  ( -38.99924736195577424, -113.9929510916434339, 12.66759465831984599 ) ) ;
#6131 = CIRCLE ( 'NONE', #21670, 20.00000000000000711 ) ;
#6132 = FACE_OUTER_BOUND ( 'NONE', #18192, .T. ) ;
#6133 = CARTESIAN_POINT ( 'NONE',  ( -21.15833593587365513, -33.18172400785640264, 69.52756813566438154 ) ) ;
#6134 = EDGE_CURVE ( 'NONE', #11194, #12842, #18269, .T. ) ;
#6135 = CARTESIAN_POINT ( 'NONE',  ( -34.50000000000000000, -113.9929510916434339, 10.50625754673609258 ) ) ;
#6136 = CARTESIAN_POINT ( 'NONE',  ( -39.00000000000000711, -114.9929510916434339, 11.73841344789285657 ) ) ;
#6137 = AXIS2_PLACEMENT_3D ( 'NONE', #2949, #16938, #3470 ) ;
#6138 = CARTESIAN_POINT ( 'NONE',  ( -35.50000000000000711, -114.9819937217110635, 10.35556074009299188 ) ) ;
#6139 = CARTESIAN_POINT ( 'NONE',  ( 0.000000000000000000, -46.19362259308839214, 8.585149169758333088 ) ) ;
#6140 = CARTESIAN_POINT ( 'NONE',  ( 0.000000000000000000, 0.000000000000000000, 65.00000000000000000 ) ) ;
#6141 = EDGE_LOOP ( 'NONE', ( #34222, #8828, #24679, #1220 ) ) ;
#6142 = VERTEX_POINT ( 'NONE', #7822 ) ;
#6143 = DIRECTION ( 'NONE',  ( 0.000000000000000000, 0.000000000000000000, 1.000000000000000000 ) ) ;
#6144 = DIRECTION ( 'NONE',  ( 0.000000000000000000, 0.5000000000000011102, -0.8660254037844379305 ) ) ;
#6145 = ORIENTED_EDGE ( 'NONE', *, *, #14083, .F. ) ;
#6146 = CARTESIAN_POINT ( 'NONE',  ( 1.799999999999996936, -5.551115123125799465E-16, -8.000000000000051514 ) ) ;
#6147 = ORIENTED_EDGE ( 'NONE', *, *, #34625, .F. ) ;
#6148 = VECTOR ( 'NONE', #16787, 1000.000000000000000 ) ;
#6149 = CARTESIAN_POINT ( 'NONE',  ( -35.50000000000000000, -115.0140978167139707, -0.6091573525984161908 ) ) ;
#6150 = CARTESIAN_POINT ( 'NONE',  ( -37.49999999999999289, -9.059673409587547965, 113.4689433211305811 ) ) ;
#6151 = CARTESIAN_POINT ( 'NONE',  ( -38.97545270896704039, -113.1123104723225197, 5.347274454178449155 ) ) ;
#6152 = ORIENTED_EDGE ( 'NONE', *, *, #13220, .T. ) ;
#6153 = LINE ( 'NONE', #3467, #8439 ) ;
#6154 = EDGE_CURVE ( 'NONE', #708, #12699, #9517, .T. ) ;
#6155 = VECTOR ( 'NONE', #21324, 1000.000000000000000 ) ;
#6156 = ORIENTED_EDGE ( 'NONE', *, *, #4523, .F. ) ;
#6157 = CARTESIAN_POINT ( 'NONE',  ( -35.50000000000000000, -116.7615919857705080, -1.632210089000343700 ) ) ;
#6158 = ORIENTED_EDGE ( 'NONE', *, *, #10194, .T. ) ;
#6159 = ORIENTED_EDGE ( 'NONE', *, *, #3389, .F. ) ;
#6160 = CIRCLE ( 'NONE', #26290, 8.000000000000001776 ) ;
#6161 = CARTESIAN_POINT ( 'NONE',  ( -35.02454729103298803, -114.8876895276775087, 7.597274454178450931 ) ) ;
#6162 = CIRCLE ( 'NONE', #10175, 52.00000000000000711 ) ;
#6163 = CARTESIAN_POINT ( 'NONE',  ( 8.000000000000000000, 0.000000000000000000, 0.000000000000000000 ) ) ;
#6164 = ORIENTED_EDGE ( 'NONE', *, *, #14417, .T. ) ;
#6165 = EDGE_LOOP ( 'NONE', ( #3297, #7262 ) ) ;
#6166 = CARTESIAN_POINT ( 'NONE',  ( -34.50000000000000000, -112.0140978167138712, -0.3747823525984256832 ) ) ;
#6167 = CARTESIAN_POINT ( 'NONE',  ( 50.00000000000000000, 20.00000000000001776, 110.0000000000000000 ) ) ;
#6168 = EDGE_CURVE ( 'NONE', #7646, #22338, #7296, .T. ) ;
#6169 = EDGE_CURVE ( 'NONE', #4346, #14835, #10682, .T. ) ;
#6170 = EDGE_CURVE ( 'NONE', #6280, #10552, #29448, .T. ) ;
#6171 = VERTEX_POINT ( 'NONE', #24058 ) ;
#6172 = VERTEX_POINT ( 'NONE', #29627 ) ;
#6173 = FACE_OUTER_BOUND ( 'NONE', #17130, .T. ) ;
#6174 = CIRCLE ( 'NONE', #14801, 20.00000000000000711 ) ;
#6175 = AXIS2_PLACEMENT_3D ( 'NONE', #18840, #24427, #8378 ) ;
#6176 = CARTESIAN_POINT ( 'NONE',  ( -37.99959864031216483, -113.9929510916434339, 12.63896776382213538 ) ) ;
#6177 = DIRECTION ( 'NONE',  ( -1.000000000000000000, 0.000000000000000000, -0.000000000000000000 ) ) ;
#6178 = LINE ( 'NONE', #17141, #5034 ) ;
#6179 = EDGE_CURVE ( 'NONE', #28842, #26596, #17565, .T. ) ;
#6180 = CARTESIAN_POINT ( 'NONE',  ( -34.50000000000000000, -111.0168437565048691, 0.9961850632443862708 ) ) ;
#6181 = CIRCLE ( 'NONE', #10224, 17.49900000000001654 ) ;
#6182 = VECTOR ( 'NONE', #32423, 1000.000000000000000 ) ;
#6183 = EDGE_CURVE ( 'NONE', #20524, #2111, #29076, .T. ) ;
#6184 = CARTESIAN_POINT ( 'NONE',  ( -38.81062062679291813, -115.9929510916434481, 13.37409560816442244 ) ) ;
#6185 = CARTESIAN_POINT ( 'NONE',  ( 0.000000000000000000, -2.710505431213761085E-17, 45.10000000000000142 ) ) ;
#6186 = VECTOR ( 'NONE', #19769, 1000.000000000000000 ) ;
#6187 = FACE_BOUND ( 'NONE', #11736, .T. ) ;
#6188 = DIRECTION ( 'NONE',  ( -1.000000000000000000, 0.000000000000000000, 0.000000000000000000 ) ) ;
#6189 = DIRECTION ( 'NONE',  ( 0.000000000000000000, 1.000000000000000000, 0.000000000000000000 ) ) ;
#6190 = DIRECTION ( 'NONE',  ( -1.000000000000000000, 0.000000000000000000, 0.000000000000000000 ) ) ;
#6191 = ORIENTED_EDGE ( 'NONE', *, *, #10844, .F. ) ;
#6192 = DIRECTION ( 'NONE',  ( -1.000000000000000000, 0.000000000000000000, 0.000000000000000000 ) ) ;
#6193 = FACE_OUTER_BOUND ( 'NONE', #7487, .T. ) ;
#6194 = CARTESIAN_POINT ( 'NONE',  ( 7.999999999999992895, 13.56094713063641599, -50.20060470671727870 ) ) ;
#6195 = DIRECTION ( 'NONE',  ( -1.000000000000000000, 0.000000000000000000, 0.000000000000000000 ) ) ;
#6196 = PLANE ( 'NONE',  #25071 ) ;
#6197 = DIRECTION ( 'NONE',  ( 0.000000000000000000, 0.000000000000000000, 1.000000000000000000 ) ) ;
#6198 = ADVANCED_FACE ( 'NONE', ( #16090, #27108 ), #26392, .F. ) ;
#6199 = AXIS2_PLACEMENT_3D ( 'NONE', #4385, #9411, #7427 ) ;
#6200 = ORIENTED_EDGE ( 'NONE', *, *, #25729, .T. ) ;
#6201 = FACE_BOUND ( 'NONE', #13504, .T. ) ;
#6202 = CARTESIAN_POINT ( 'NONE',  ( 8.000000000000007105, 13.42368113696682030, 3.975523202428055125 ) ) ;
#6203 = CARTESIAN_POINT ( 'NONE',  ( 65.00000000000001421, 49.63000703270403591, 62.56502393413636298 ) ) ;
#6204 = ORIENTED_EDGE ( 'NONE', *, *, #6168, .T. ) ;
#6205 = CARTESIAN_POINT ( 'NONE',  ( -37.74901162816868805, -113.3347980657955958, 6.433975545821551734 ) ) ;
#6206 = ORIENTED_EDGE ( 'NONE', *, *, #6179, .F. ) ;
#6207 = EDGE_CURVE ( 'NONE', #19338, #1815, #1476, .T. ) ;
#6208 = VECTOR ( 'NONE', #31660, 1000.000000000000000 ) ;
#6209 = ORIENTED_EDGE ( 'NONE', *, *, #8034, .F. ) ;
#6210 = EDGE_LOOP ( 'NONE', ( #13811, #34698, #5055, #32166 ) ) ;
#6211 = VECTOR ( 'NONE', #10954, 1000.000000000000000 ) ;
#6212 = LINE ( 'NONE', #6383, #3420 ) ;
#6213 = EDGE_CURVE ( 'NONE', #7819, #17248, #15255, .T. ) ;
#6214 = EDGE_CURVE ( 'NONE', #6339, #17196, #14686, .T. ) ;
#6215 = AXIS2_PLACEMENT_3D ( 'NONE', #694, #19592, #14728 ) ;
#6216 = CARTESIAN_POINT ( 'NONE',  ( -35.50000000000000711, -115.9630435732166518, -0.9469505670456015434 ) ) ;
#6217 = FACE_OUTER_BOUND ( 'NONE', #13998, .T. ) ;
#6218 = CARTESIAN_POINT ( 'NONE',  ( -35.50000000000000711, -114.1712995509219724, 9.522174004479579068 ) ) ;
#6219 = DIRECTION ( 'NONE',  ( -1.000000000000000000, 0.000000000000000000, 0.000000000000000000 ) ) ;
#6220 = DIRECTION ( 'NONE',  ( 0.000000000000000000, -0.2538061376417682924, -0.9672551082808338307 ) ) ;
#6221 = ADVANCED_FACE ( 'NONE', ( #18989 ), #16802, .T. ) ;
#6222 = CARTESIAN_POINT ( 'NONE',  ( -34.50000000000000000, -114.0882517521923489, 9.510534276948430232 ) ) ;
#6223 = DIRECTION ( 'NONE',  ( 0.000000000000000000, 0.000000000000000000, -1.000000000000000000 ) ) ;
#6224 = CARTESIAN_POINT ( 'NONE',  ( -21.15833593587365513, -30.19486372867095980, 84.29903810567654432 ) ) ;
#6225 = CARTESIAN_POINT ( 'NONE',  ( -35.50000000000000000, -114.2207110452431635, 8.519246492191951958 ) ) ;
#6226 = CARTESIAN_POINT ( 'NONE',  ( -35.50000000000000711, -113.2637153405686519, 1.912112492696748989 ) ) ;
#6227 = FACE_OUTER_BOUND ( 'NONE', #34921, .T. ) ;
#6228 = CARTESIAN_POINT ( 'NONE',  ( 8.000000000000000000, 8.931325931664597206, 16.53603053422209612 ) ) ;
#6229 = CIRCLE ( 'NONE', #5656, 52.00000000000000711 ) ;
#6230 = LINE ( 'NONE', #1191, #23965 ) ;
#6231 = FACE_BOUND ( 'NONE', #11676, .T. ) ;
#6232 =( REPRESENTATION_RELATIONSHIP ('NONE','NONE', #26607, #31430 ) REPRESENTATION_RELATIONSHIP_WITH_TRANSFORMATION ( #24934 )SHAPE_REPRESENTATION_RELATIONSHIP( ) );
#6233 = DIRECTION ( 'NONE',  ( 0.000000000000000000, 0.4999999999999948930, 0.8660254037844415942 ) ) ;
#6234 = DIRECTION ( 'NONE',  ( 0.000000000000000000, -0.9822872507286904975, 0.1873813145857149698 ) ) ;
#6235 = VERTEX_POINT ( 'NONE', #27644 ) ;
#6236 = CARTESIAN_POINT ( 'NONE',  ( -37.05926240293131713, -113.0000000000000000, 5.121475545821551734 ) ) ;
#6237 = DIRECTION ( 'NONE',  ( 1.000000000000000000, 0.000000000000000000, 0.000000000000000000 ) ) ;
#6238 = DIRECTION ( 'NONE',  ( 0.000000000000000000, 0.6845471059286846183, 0.7289686274214154382 ) ) ;
#6239 = EDGE_CURVE ( 'NONE', #13527, #8697, #34844, .T. ) ;
#6240 = VERTEX_POINT ( 'NONE', #6015 ) ;
#6241 = ORIENTED_EDGE ( 'NONE', *, *, #22646, .F. ) ;
#6242 = EDGE_CURVE ( 'NONE', #10299, #7183, #31366, .T. ) ;
#6243 = CARTESIAN_POINT ( 'NONE',  ( 8.000000000000000000, 0.000000000000000000, 17.49900000000000233 ) ) ;
#6244 = ADVANCED_FACE ( 'NONE', ( #8176 ), #5672, .F. ) ;
#6245 = CYLINDRICAL_SURFACE ( 'NONE', #7171, 47.49900000000001654 ) ;
#6246 = VERTEX_POINT ( 'NONE', #32857 ) ;
#6247 = CARTESIAN_POINT ( 'NONE',  ( -39.97545270896702618, -112.6980969099493990, 8.347274454178448266 ) ) ;
#6248 = ORIENTED_EDGE ( 'NONE', *, *, #32571, .T. ) ;
#6249 = CARTESIAN_POINT ( 'NONE',  ( 8.000000000000000000, 16.53603053422208902, -8.931325931664652273 ) ) ;
#6250 = DIRECTION ( 'NONE',  ( 1.000000000000000000, 0.000000000000000000, 0.000000000000000000 ) ) ;
#6251 = EDGE_CURVE ( 'NONE', #28225, #14425, #2982, .T. ) ;
#6252 = AXIS2_PLACEMENT_3D ( 'NONE', #3169, #30703, #3520 ) ;
#6253 = ADVANCED_FACE ( 'NONE', ( #33378 ), #430, .T. ) ;
#6254 = APPLICATION_PROTOCOL_DEFINITION ( 'draft international standard', 'automotive_design', 1998, #8498 ) ;
#6255 = DIRECTION ( 'NONE',  ( 0.000000000000000000, 0.000000000000000000, 1.000000000000000000 ) ) ;
#6256 = EDGE_LOOP ( 'NONE', ( #24084, #14496, #10962, #18442 ) ) ;
#6257 = VERTEX_POINT ( 'NONE', #3150 ) ;
#6258 = CARTESIAN_POINT ( 'NONE',  ( 0.000000000000000000, 46.90537658765334328, -2.727856614653800804 ) ) ;
#6259 = ORIENTED_EDGE ( 'NONE', *, *, #18052, .F. ) ;
#6260 = DIRECTION ( 'NONE',  ( -1.000000000000000000, 0.000000000000000000, 0.000000000000000000 ) ) ;
#6261 = CARTESIAN_POINT ( 'NONE',  ( -34.50000000000000000, -113.6318576702834804, 1.956056246348823580 ) ) ;
#6262 = CARTESIAN_POINT ( 'NONE',  ( 8.000000000000007105, 9.604183132802452505, 5.908880290975567995 ) ) ;
#6263 = PLANE ( 'NONE',  #25922 ) ;
#6264 = CARTESIAN_POINT ( 'NONE',  ( -39.00000000000000711, -114.9929510916434339, 12.44250253426874941 ) ) ;
#6265 = CARTESIAN_POINT ( 'NONE',  ( -4.000000000000000000, -2.710505431213761085E-17, 55.00000000000000000 ) ) ;
#6266 = DIRECTION ( 'NONE',  ( 0.000000000000000000, -0.3090169943749545567, 0.9510565162951513107 ) ) ;
#6267 = CARTESIAN_POINT ( 'NONE',  ( -34.50000000000000000, -114.1928420708668028, 8.515919878418792166 ) ) ;
#6268 = DIRECTION ( 'NONE',  ( -1.000000000000000000, 0.000000000000000000, 0.000000000000000000 ) ) ;
#6269 = DIRECTION ( 'NONE',  ( -1.000000000000000000, -0.000000000000000000, 0.000000000000000000 ) ) ;
#6270 = CARTESIAN_POINT ( 'NONE',  ( 4.000000000000000000, 4.627536653468036720E-16, 38.90000000000000568 ) ) ;
#6271 = DIRECTION ( 'NONE',  ( 0.000000000000000000, 0.6845471059286899473, -0.7289686274214103312 ) ) ;
#6272 = ORIENTED_EDGE ( 'NONE', *, *, #28436, .T. ) ;
#6273 = DIRECTION ( 'NONE',  ( -1.000000000000000000, 0.000000000000000000, 0.000000000000000000 ) ) ;
#6274 = ORIENTED_EDGE ( 'NONE', *, *, #15016, .T. ) ;
#6275 = AXIS2_PLACEMENT_3D ( 'NONE', #18654, #24609, #35596 ) ;
#6276 = CARTESIAN_POINT ( 'NONE',  ( -39.99999999999999289, -113.9407375970686758, 8.253524454178448266 ) ) ;
#6277 = CARTESIAN_POINT ( 'NONE',  ( 0.000000000000000000, 0.000000000000000000, 0.000000000000000000 ) ) ;
#6278 = CARTESIAN_POINT ( 'NONE',  ( -35.50000000000000711, -115.1770117227680998, -1.611965039240062181 ) ) ;
#6279 = EDGE_CURVE ( 'NONE', #2211, #7746, #22738, .T. ) ;
#6280 = VERTEX_POINT ( 'NONE', #24931 ) ;
#6281 = VECTOR ( 'NONE', #13921, 1000.000000000000000 ) ;
#6282 = EDGE_LOOP ( 'NONE', ( #15476, #24782 ) ) ;
#6283 = ADVANCED_FACE ( 'NONE', ( #22208 ), #19158, .T. ) ;
#6284 = CYLINDRICAL_SURFACE ( 'NONE', #30360, 4.000000000000000000 ) ;
#6285 = CARTESIAN_POINT ( 'NONE',  ( 0.000000000000000000, 0.000000000000000000, 0.000000000000000000 ) ) ;
#6286 = ORIENTED_EDGE ( 'NONE', *, *, #2219, .F. ) ;
#6287 = VERTEX_POINT ( 'NONE', #13590 ) ;
#6288 =( GEOMETRIC_REPRESENTATION_CONTEXT ( 3 ) GLOBAL_UNCERTAINTY_ASSIGNED_CONTEXT ( ( #20405 ) ) GLOBAL_UNIT_ASSIGNED_CONTEXT ( ( #18133, #24101, #7159 ) ) REPRESENTATION_CONTEXT ( 'NONE', 'WORKASPACE' ) );
#6289 = CARTESIAN_POINT ( 'NONE',  ( 7.999999999999992895, -11.90021268425521939, -45.45261810511225065 ) ) ;
#6290 = ORIENTED_EDGE ( 'NONE', *, *, #2985, .F. ) ;
#6291 = VERTEX_POINT ( 'NONE', #2814 ) ;
#6292 = CARTESIAN_POINT ( 'NONE',  ( -38.97545270896704039, -114.8876895276775087, 3.152725545821551290 ) ) ;
#6293 = DIRECTION ( 'NONE',  ( 0.000000000000000000, 0.000000000000000000, 1.000000000000000000 ) ) ;
#6294 = CARTESIAN_POINT ( 'NONE',  ( 38.00000000000000000, 10.50000000000000355, 1.285879139104720436E-15 ) ) ;
#6295 = ORIENTED_EDGE ( 'NONE', *, *, #26286, .F. ) ;
#6296 = ORIENTED_EDGE ( 'NONE', *, *, #9986, .F. ) ;
#6297 = CARTESIAN_POINT ( 'NONE',  ( -35.50000000000000000, -111.0140978167138570, 0.3752176474015639918 ) ) ;
#6298 = DIRECTION ( 'NONE',  ( -1.000000000000000000, 0.000000000000000000, 0.000000000000000000 ) ) ;
#6299 = ORIENTED_EDGE ( 'NONE', *, *, #34445, .F. ) ;
#6300 = CARTESIAN_POINT ( 'NONE',  ( -35.50000000000000711, -114.9929510916434339, 11.73841344789270202 ) ) ;
#6301 = AXIS2_PLACEMENT_3D ( 'NONE', #32743, #13319, #34936 ) ;
#6302 = CARTESIAN_POINT ( 'NONE',  ( -37.51022648969539119, -113.9929510916434339, 14.11852173794918563 ) ) ;
#6303 = CARTESIAN_POINT ( 'NONE',  ( 0.000000000000000000, 0.000000000000000000, 65.00000000000000000 ) ) ;
#6304 = DIRECTION ( 'NONE',  ( 0.000000000000000000, 0.000000000000000000, 1.000000000000000000 ) ) ;
#6305 = AXIS2_PLACEMENT_3D ( 'NONE', #8571, #33415, #27152 ) ;
#6306 = ADVANCED_FACE ( 'NONE', ( #32160 ), #7316, .T. ) ;
#6307 = CARTESIAN_POINT ( 'NONE',  ( -35.75562914091914024, -113.9929510916434339, 14.09929883582542409 ) ) ;
#6309 = CARTESIAN_POINT ( 'NONE',  ( 8.000000000000000000, 6.336799421339808447, 16.31134495048485533 ) ) ;
#6308 = VECTOR ( 'NONE', #19220, 1000.000000000000000 ) ;
#6310 = CARTESIAN_POINT ( 'NONE',  ( -35.50000000000000711, -114.9929510916434339, 12.50851088611648088 ) ) ;
#6311 = DIRECTION ( 'NONE',  ( -1.000000000000000000, 0.000000000000000000, 0.000000000000000000 ) ) ;
#6312 = DIRECTION ( 'NONE',  ( -1.000000000000000000, 0.000000000000000000, 0.000000000000000000 ) ) ;
#6313 = ORIENTED_EDGE ( 'NONE', *, *, #32391, .F. ) ;
#6314 = CARTESIAN_POINT ( 'NONE',  ( -35.50000000000000711, -114.0000000000003411, 9.500000000000035527 ) ) ;
#6315 = ORIENTED_EDGE ( 'NONE', *, *, #25365, .T. ) ;
#6316 = DIRECTION ( 'NONE',  ( -8.708451184622495809E-17, 6.938893903907203726E-17, 1.000000000000000000 ) ) ;
#6317 = DIRECTION ( 'NONE',  ( 0.000000000000000000, 0.000000000000000000, -1.000000000000000000 ) ) ;
#6318 = ORIENTED_EDGE ( 'NONE', *, *, #6213, .T. ) ;
#6319 = DIRECTION ( 'NONE',  ( -0.9995917534020514195, -0.02857142857143298367, 1.161550059124387962E-15 ) ) ;
#6320 = ORIENTED_EDGE ( 'NONE', *, *, #23648, .F. ) ;
#6321 = EDGE_CURVE ( 'NONE', #28112, #10384, #3795, .T. ) ;
#6322 = CARTESIAN_POINT ( 'NONE',  ( -35.50000000000000000, -113.0140978167137860, -0.6247823525984055326 ) ) ;
#6323 = CARTESIAN_POINT ( 'NONE',  ( -9.999999999999994671, 0.000000000000000000, 0.000000000000000000 ) ) ;
#6324 = CARTESIAN_POINT ( 'NONE',  ( -37.66520193420439000, -113.2509883718312977, 8.441024454178448266 ) ) ;
#6325 = AXIS2_PLACEMENT_3D ( 'NONE', #7279, #29072, #31235 ) ;
#6326 = EDGE_LOOP ( 'NONE', ( #7978, #10210, #21172, #28261 ) ) ;
#6327 = CARTESIAN_POINT ( 'NONE',  ( -35.62769128460905677, -115.4561184093552413, 4.691024454178448266 ) ) ;
#6328 = VECTOR ( 'NONE', #18358, 1000.000000000000000 ) ;
#6329 = DIRECTION ( 'NONE',  ( -0.000000000000000000, 1.611597878369477150E-16, -1.000000000000000000 ) ) ;
#6330 = CARTESIAN_POINT ( 'NONE',  ( -35.50000000000000000, -117.0140978167138854, 0.6252176474015650465 ) ) ;
#6331 = ORIENTED_EDGE ( 'NONE', *, *, #5103, .T. ) ;
#6332 = ORIENTED_EDGE ( 'NONE', *, *, #11686, .T. ) ;
#6333 = DIRECTION ( 'NONE',  ( -1.000000000000000000, 0.000000000000000000, 0.000000000000000000 ) ) ;
#6334 = EDGE_CURVE ( 'NONE', #26981, #19072, #16411, .T. ) ;
#6335 = AXIS2_PLACEMENT_3D ( 'NONE', #26756, #13076, #9818 ) ;
#6336 = AXIS2_PLACEMENT_3D ( 'NONE', #19763, #28926, #26223 ) ;
#6337 = DIRECTION ( 'NONE',  ( 0.000000000000000000, 0.1253332335642974305, 0.9921147013144787641 ) ) ;
#6338 = ORIENTED_EDGE ( 'NONE', *, *, #9978, .T. ) ;
#6339 = VERTEX_POINT ( 'NONE', #11419 ) ;
#6340 = CARTESIAN_POINT ( 'NONE',  ( -34.50000000000000000, -115.0140978167138712, 0.6252176474015650465 ) ) ;
#6341 = DIRECTION ( 'NONE',  ( 0.000000000000000000, 0.000000000000000000, -1.000000000000000000 ) ) ;
#6342 = PRODUCT ( 'shaft 3', 'shaft 3', '', ( #30737 ) ) ;
#6343 = VERTEX_POINT ( 'NONE', #24759 ) ;
#6344 = ORIENTED_EDGE ( 'NONE', *, *, #18491, .T. ) ;
#6345 = DIRECTION ( 'NONE',  ( 0.000000000000000000, 0.000000000000000000, -1.000000000000000000 ) ) ;
#6346 = CARTESIAN_POINT ( 'NONE',  ( -35.91854304697312728, -113.9929510916434339, 13.11211614918345703 ) ) ;
#6347 = CARTESIAN_POINT ( 'NONE',  ( 0.000000000000000000, 51.19683565102457834, -9.104066087302935983 ) ) ;
#6348 = AXIS2_PLACEMENT_3D ( 'NONE', #26650, #26824, #951 ) ;
#6349 = CARTESIAN_POINT ( 'NONE',  ( 7.999999999999992895, 17.08890430202814059, -43.76671000081924490 ) ) ;
#6350 = CARTESIAN_POINT ( 'NONE',  ( -35.52552712174883709, -113.9929510916434339, 12.77960891308624625 ) ) ;
#6351 = CARTESIAN_POINT ( 'NONE',  ( -35.50000000000000000, -115.9929510916434481, 10.68227981832981044 ) ) ;
#6352 = CARTESIAN_POINT ( 'NONE',  ( 0.000000000000000000, 0.000000000000000000, -1.200000000000006617 ) ) ;
#6353 = AXIS2_PLACEMENT_3D ( 'NONE', #28242, #6269, #23184 ) ;
#6354 = DIRECTION ( 'NONE',  ( -1.000000000000000000, -0.000000000000000000, 0.000000000000000000 ) ) ;
#6355 = VECTOR ( 'NONE', #20571, 1000.000000000000000 ) ;
#6356 = DIRECTION ( 'NONE',  ( 1.000000000000000000, 0.000000000000000000, 0.000000000000000000 ) ) ;
#6357 = CARTESIAN_POINT ( 'NONE',  ( -44.00000000000000000, 0.000000000000000000, 0.000000000000000000 ) ) ;
#6358 = CIRCLE ( 'NONE', #5808, 8.000000000000015987 ) ;
#6359 = CARTESIAN_POINT ( 'NONE',  ( 0.000000000000000000, -2.710505431213761085E-17, -21.89999999999999858 ) ) ;
#6360 = ORIENTED_EDGE ( 'NONE', *, *, #29391, .F. ) ;
#6361 = CARTESIAN_POINT ( 'NONE',  ( 5.400000000000015454, -1.000000000000002220, -22.00000000000000000 ) ) ;
#6362 = CARTESIAN_POINT ( 'NONE',  ( 7.999999999999992895, 44.47301969247445896, 16.68249143361927267 ) ) ;
#6363 = ADVANCED_FACE ( 'NONE', ( #22383 ), #25281, .T. ) ;
#6364 = CARTESIAN_POINT ( 'NONE',  ( -35.50000000000000711, -114.0000000000000853, 2.000000000000001776 ) ) ;
#6365 = DIRECTION ( 'NONE',  ( 4.662936703425629071E-15, -1.000000000000000000, 4.222049128630314618E-16 ) ) ;
#6366 = EDGE_CURVE ( 'NONE', #11436, #13129, #18144, .T. ) ;
#6367 = ITEM_DEFINED_TRANSFORMATION ( 'NONE', 'NONE', #27096,  #21307 ) ;
#6368 = DIRECTION ( 'NONE',  ( -1.000000000000000000, 0.000000000000000000, 0.000000000000000000 ) ) ;
#6369 = DIRECTION ( 'NONE',  ( -1.000000000000000000, 0.000000000000000000, 0.000000000000000000 ) ) ;
#6370 = ORIENTED_EDGE ( 'NONE', *, *, #16733, .F. ) ;
#6371 = DIRECTION ( 'NONE',  ( 0.000000000000000000, 0.9510565162951544194, -0.3090169943749447867 ) ) ;
#6372 = DIRECTION ( 'NONE',  ( 0.000000000000000000, 0.000000000000000000, 1.000000000000000000 ) ) ;
#6373 = PLANE ( 'NONE',  #1323 ) ;
#6374 = ORIENTED_EDGE ( 'NONE', *, *, #3742, .T. ) ;
#6375 = ORIENTED_EDGE ( 'NONE', *, *, #1207, .F. ) ;
#6376 = VECTOR ( 'NONE', #9493, 1000.000000000000000 ) ;
#6377 = CARTESIAN_POINT ( 'NONE',  ( -37.66520193420439711, -114.7490116281687023, 6.058975545821550845 ) ) ;
#6378 = EDGE_CURVE ( 'NONE', #20170, #32626, #6535, .T. ) ;
#6379 = ORIENTED_EDGE ( 'NONE', *, *, #34167, .T. ) ;
#6380 = EDGE_CURVE ( 'NONE', #6623, #17782, #28158, .T. ) ;
#6381 = ORIENTED_EDGE ( 'NONE', *, *, #1344, .T. ) ;
#6382 = VERTEX_POINT ( 'NONE', #6362 ) ;
#6383 = CARTESIAN_POINT ( 'NONE',  ( 4.000000000000003553, -0.6505223195686533622, 51.99593080916758936 ) ) ;
#6384 = VECTOR ( 'NONE', #11832, 1000.000000000000000 ) ;
#6385 = COLOUR_RGB ( '', 0.08235294, 0.09019608, 0.10196078) ;
#6386 = CARTESIAN_POINT ( 'NONE',  ( -42.49999999999999289, -25.98076211353322051, 84.99999999999992895 ) ) ;
#6387 = CARTESIAN_POINT ( 'NONE',  ( 0.000000000000000000, 0.000000000000000000, -43.60000000000000142 ) ) ;
#6388 = CARTESIAN_POINT ( 'NONE',  ( -35.50000000000000711, -114.9929510916434339, 12.56351784598954424 ) ) ;
#6389 = DIRECTION ( 'NONE',  ( -1.000000000000000000, 0.000000000000000000, 0.000000000000000000 ) ) ;
#6390 = DIRECTION ( 'NONE',  ( 0.000000000000000000, 0.2486898871648482723, 0.9685831611286327414 ) ) ;
#6391 = EDGE_CURVE ( 'NONE', #1617, #15604, #23922, .T. ) ;
#6392 = CARTESIAN_POINT ( 'NONE',  ( -34.50000000000000000, -114.1068310684433129, 9.512752019463897923 ) ) ;
#6393 = LINE ( 'NONE', #33769, #7622 ) ;
#6394 = DIRECTION ( 'NONE',  ( 0.000000000000000000, 0.000000000000000000, -1.000000000000000000 ) ) ;
#6395 = EDGE_LOOP ( 'NONE', ( #22688, #31988, #1697, #34465 ) ) ;
#6396 = CARTESIAN_POINT ( 'NONE',  ( -35.50000000000000000, -115.9792481177720731, 10.26484292309424795 ) ) ;
#6397 = DIRECTION ( 'NONE',  ( 0.000000000000000000, 0.000000000000000000, 1.000000000000000000 ) ) ;
#6398 = DIRECTION ( 'NONE',  ( 0.000000000000000000, 0.000000000000000000, -1.000000000000000000 ) ) ;
#6399 = DIRECTION ( 'NONE',  ( 0.000000000000000000, 0.000000000000000000, 1.000000000000000000 ) ) ;
#6400 = DIRECTION ( 'NONE',  ( 0.000000000000000000, 0.000000000000000000, -1.000000000000000000 ) ) ;
#6401 = EDGE_CURVE ( 'NONE', #15022, #9129, #28508, .T. ) ;
#6402 = DIRECTION ( 'NONE',  ( 1.000000000000000000, -1.110223024625156540E-16, 0.000000000000000000 ) ) ;
#6403 = FACE_OUTER_BOUND ( 'NONE', #3552, .T. ) ;
#6404 = ORIENTED_EDGE ( 'NONE', *, *, #7552, .F. ) ;
#6405 = EDGE_CURVE ( 'NONE', #9040, #12726, #2083, .T. ) ;
#6406 = EDGE_CURVE ( 'NONE', #7746, #13301, #28332, .T. ) ;
#6407 = AXIS2_PLACEMENT_3D ( 'NONE', #10651, #10836, #16572 ) ;
#6408 = CARTESIAN_POINT ( 'NONE',  ( -37.99999999999998579, -114.0592624029313242, 9.246475545821549957 ) ) ;
#6409 = AXIS2_PLACEMENT_3D ( 'NONE', #7493, #29294, #29648 ) ;
#6410 = DIRECTION ( 'NONE',  ( 0.000000000000000000, -1.000000000000000000, 0.000000000000000000 ) ) ;
#6411 = CARTESIAN_POINT ( 'NONE',  ( 8.000000000000007105, -9.919332006307138627, -5.363026430117212584 ) ) ;
#6412 = ORIENTED_EDGE ( 'NONE', *, *, #25778, .T. ) ;
#6413 = VERTEX_POINT ( 'NONE', #9246 ) ;
#6414 = CYLINDRICAL_SURFACE ( 'NONE', #11406, 20.00000000000000355 ) ;
#6415 = CARTESIAN_POINT ( 'NONE',  ( 0.000000000000000000, -2.710505431213761085E-17, -45.10000000000000142 ) ) ;
#6416 = ORIENTED_EDGE ( 'NONE', *, *, #26210, .T. ) ;
#6417 = CARTESIAN_POINT ( 'NONE',  ( -39.07941549657748936, -111.8367748094582055, 8.441024454178448266 ) ) ;
#6418 = ORIENTED_EDGE ( 'NONE', *, *, #5774, .T. ) ;
#6419 = EDGE_CURVE ( 'NONE', #529, #334, #20198, .T. ) ;
#6420 = DIRECTION ( 'NONE',  ( 0.000000000000000000, 0.000000000000000000, 1.000000000000000000 ) ) ;
#6421 = PLANE ( 'NONE',  #28630 ) ;
#6422 = SHAPE_DEFINITION_REPRESENTATION ( #4370, #22901 ) ;
#6423 = DIRECTION ( 'NONE',  ( 9.266685234918781277E-17, -6.938893903907202493E-17, -1.000000000000000000 ) ) ;
#6424 = ORIENTED_EDGE ( 'NONE', *, *, #16067, .F. ) ;
#6425 = VERTEX_POINT ( 'NONE', #12299 ) ;
#6426 = CARTESIAN_POINT ( 'NONE',  ( 0.000000000000000000, -16.53603053422215297, 8.931325931664547468 ) ) ;
#6427 = CARTESIAN_POINT ( 'NONE',  ( 4.747884751462025044, -5.143694235356003119, 0.000000000000000000 ) ) ;
#6428 = AXIS2_PLACEMENT_3D ( 'NONE', #3087, #2916, #191 ) ;
#6429 = ORIENTED_EDGE ( 'NONE', *, *, #23019, .F. ) ;
#6430 = CIRCLE ( 'NONE', #20805, 52.00000000000000711 ) ;
#6431 = CARTESIAN_POINT ( 'NONE',  ( -55.00000000000000000, -2.775557561562891351E-14, 106.0000000000000000 ) ) ;
#6432 = EDGE_CURVE ( 'NONE', #7164, #4091, #15276, .T. ) ;
#6433 = CARTESIAN_POINT ( 'NONE',  ( -34.50000000000000000, -115.0140978167138712, -0.6247823525984408377 ) ) ;
#6434 = LINE ( 'NONE', #14519, #6384 ) ;
#6435 = FACE_OUTER_BOUND ( 'NONE', #6469, .T. ) ;
#6436 = CARTESIAN_POINT ( 'NONE',  ( -34.50000000000000000, -115.9929510916434481, 10.56126450660895699 ) ) ;
#6437 = ADVANCED_FACE ( 'NONE', ( #6193, #34268 ), #25825, .T. ) ;
#6438 = DIRECTION ( 'NONE',  ( 0.000000000000000000, 0.000000000000000000, 1.000000000000000000 ) ) ;
#6439 = CARTESIAN_POINT ( 'NONE',  ( -44.00000000000000000, 4.000000000000000000, 4.898587196589411843E-16 ) ) ;
#6440 = CARTESIAN_POINT ( 'NONE',  ( -38.92341863475394348, -114.9929510916434339, 13.10177712753322155 ) ) ;
#6441 = DIRECTION ( 'NONE',  ( -1.783119874454246424E-31, -1.187911941725854497E-31, 1.000000000000000000 ) ) ;
#6442 = CARTESIAN_POINT ( 'NONE',  ( -35.00000000000000000, -116.0140978167138712, 0.8752176474015622709 ) ) ;
#6443 = AXIS2_PLACEMENT_3D ( 'NONE', #18806, #29806, #8171 ) ;
#6444 = DIRECTION ( 'NONE',  ( 1.000000000000000000, -1.110223024625156540E-16, 0.000000000000000000 ) ) ;
#6445 = CARTESIAN_POINT ( 'NONE',  ( 23.00000000000000711, -3.999999999999980904, 0.000000000000000000 ) ) ;
#6446 = ORIENTED_EDGE ( 'NONE', *, *, #14515, .T. ) ;
#6447 = DIRECTION ( 'NONE',  ( -1.000000000000000000, 0.000000000000000000, -0.000000000000000000 ) ) ;
#6448 = ORIENTED_EDGE ( 'NONE', *, *, #25788, .F. ) ;
#6449 = EDGE_CURVE ( 'NONE', #25742, #3119, #9602, .T. ) ;
#6450 = CARTESIAN_POINT ( 'NONE',  ( -37.05926240293131713, -111.0000000000000284, 3.621475545821551734 ) ) ;
#6451 = EDGE_CURVE ( 'NONE', #26552, #17521, #22199, .T. ) ;
#6452 = DIRECTION ( 'NONE',  ( -1.000000000000000000, 0.000000000000000000, 0.000000000000000000 ) ) ;
#6453 = CARTESIAN_POINT ( 'NONE',  ( -35.50000000000000711, -114.3474311500471430, -1.624782352598427959 ) ) ;
#6454 = ORIENTED_EDGE ( 'NONE', *, *, #14256, .T. ) ;
#6455 = EDGE_LOOP ( 'NONE', ( #8898, #4356 ) ) ;
#6456 = LINE ( 'NONE', #33468, #28071 ) ;
#6457 = VECTOR ( 'NONE', #22153, 1000.000000000000000 ) ;
#6458 = CARTESIAN_POINT ( 'NONE',  ( 7.999999999999992895, -37.91532898920900863, -28.61088654061680359 ) ) ;
#6459 = ORIENTED_EDGE ( 'NONE', *, *, #29262, .F. ) ;
#6460 = CIRCLE ( 'NONE', #26601, 4.000000000000000000 ) ;
#6461 = EDGE_LOOP ( 'NONE', ( #31695, #27909, #33772, #3960 ) ) ;
#6462 = CIRCLE ( 'NONE', #26028, 20.00000000000000355 ) ;
#6463 = CARTESIAN_POINT ( 'NONE',  ( -34.49999999999998579, -15.39406523420380069, 82.16330312067053399 ) ) ;
#6464 = VERTEX_POINT ( 'NONE', #9415 ) ;
#6465 = ORIENTED_EDGE ( 'NONE', *, *, #29013, .T. ) ;
#6466 = CARTESIAN_POINT ( 'NONE',  ( -35.02454729103298092, -113.1123104723225055, 3.902725545821551290 ) ) ;
#6467 = FILL_AREA_STYLE_COLOUR ( '', #550 ) ;
#6468 = LINE ( 'NONE', #26098, #20166 ) ;
#6469 = EDGE_LOOP ( 'NONE', ( #11084, #10812 ) ) ;
#6470 = ORIENTED_EDGE ( 'NONE', *, *, #15880, .F. ) ;
#6471 = CARTESIAN_POINT ( 'NONE',  ( -35.50000000000000000, -111.0140978167138570, -0.3122823525984338988 ) ) ;
#6472 = CARTESIAN_POINT ( 'NONE',  ( 70.00000000000001421, -24.67840078103129997, 92.38605814759151258 ) ) ;
#6473 = ORIENTED_EDGE ( 'NONE', *, *, #2901, .T. ) ;
#6474 = DIRECTION ( 'NONE',  ( 1.000000000000000000, 0.000000000000000000, -1.691777834109591502E-31 ) ) ;
#6475 = EDGE_CURVE ( 'NONE', #21098, #19242, #1498, .T. ) ;
#6476 = ADVANCED_FACE ( 'NONE', ( #28695 ), #28867, .F. ) ;
#6477 = CIRCLE ( 'NONE', #28929, 6.765000000000044977 ) ;
#6478 = CARTESIAN_POINT ( 'NONE',  ( -39.00000000000000000, -113.9929510916434339, 12.50851088611646311 ) ) ;
#6479 = AXIS2_PLACEMENT_3D ( 'NONE', #13154, #16168, #5050 ) ;
#6480 = DIRECTION ( 'NONE',  ( -1.000000000000000000, 0.000000000000000000, 0.000000000000000000 ) ) ;
#6481 = DIRECTION ( 'NONE',  ( -1.000000000000000000, -0.000000000000000000, 0.000000000000000000 ) ) ;
#6482 = CARTESIAN_POINT ( 'NONE',  ( -37.46093750000000711, -113.9929510916434339, 14.11852480586265024 ) ) ;
#6483 = CARTESIAN_POINT ( 'NONE',  ( 7.999999999999992895, -36.34385289850609979, 29.77717097092063980 ) ) ;
#6484 = CARTESIAN_POINT ( 'NONE',  ( -35.74814306589956914, -114.9929510916434339, 13.05539834812772781 ) ) ;
#6485 = ORIENTED_EDGE ( 'NONE', *, *, #11730, .T. ) ;
#6486 = CARTESIAN_POINT ( 'NONE',  ( -23.00000000000000355, -3.999999999999993339, 0.000000000000000000 ) ) ;
#6487 = DIRECTION ( 'NONE',  ( -1.000000000000000000, 0.000000000000000000, 0.000000000000000000 ) ) ;
#6488 = ORIENTED_EDGE ( 'NONE', *, *, #11988, .T. ) ;
#6489 = CARTESIAN_POINT ( 'NONE',  ( -35.50000000000000711, -114.9929510916434339, 10.85830208992344303 ) ) ;
#6490 = EDGE_LOOP ( 'NONE', ( #23871, #9576 ) ) ;
#6491 = DIRECTION ( 'NONE',  ( -1.000000000000000000, 0.000000000000000000, 0.000000000000000000 ) ) ;
#6492 = ORIENTED_EDGE ( 'NONE', *, *, #27324, .T. ) ;
#6493 = VECTOR ( 'NONE', #2695, 1000.000000000000000 ) ;
#6494 = DIRECTION ( 'NONE',  ( 1.000000000000000000, -5.339440136655853966E-16, 0.000000000000000000 ) ) ;
#6495 = VERTEX_POINT ( 'NONE', #11951 ) ;
#6496 = VECTOR ( 'NONE', #6192, 1000.000000000000000 ) ;
#6497 = CARTESIAN_POINT ( 'NONE',  ( -35.50000000000000000, -114.8474311500471572, -0.6247823525984269599 ) ) ;
#6498 = CARTESIAN_POINT ( 'NONE',  ( 1.600000000000004086, -12.74999999999999822, -1.200000000000006617 ) ) ;
#6499 = CARTESIAN_POINT ( 'NONE',  ( -38.99999999999999289, -113.9407375970686900, 3.753524454178449155 ) ) ;
#6500 = VERTEX_POINT ( 'NONE', #25638 ) ;
#6501 = CARTESIAN_POINT ( 'NONE',  ( -36.94073759706868287, -112.0000000000000142, 2.628524454178448710 ) ) ;
#6502 = DIRECTION ( 'NONE',  ( 0.000000000000000000, 0.000000000000000000, 1.000000000000000000 ) ) ;
#6503 = CARTESIAN_POINT ( 'NONE',  ( -35.50000000000000711, -116.0141056290913610, -0.5935324770972248976 ) ) ;
#6504 = AXIS2_PLACEMENT_3D ( 'NONE', #30058, #28068, #19416 ) ;
#6505 = ORIENTED_EDGE ( 'NONE', *, *, #13879, .T. ) ;
#6506 = ORIENTED_EDGE ( 'NONE', *, *, #29728, .F. ) ;
#6507 = DIRECTION ( 'NONE',  ( 1.000000000000000000, 1.387778780781445922E-16, 0.000000000000000000 ) ) ;
#6508 = AXIS2_PLACEMENT_3D ( 'NONE', #5684, #16642, #14293 ) ;
#6509 = LINE ( 'NONE', #29016, #31671 ) ;
#6510 = EDGE_LOOP ( 'NONE', ( #14551, #19859, #15639, #28204, #10827, #22176 ) ) ;
#6511 = ORIENTED_EDGE ( 'NONE', *, *, #28401, .T. ) ;
#6512 = CARTESIAN_POINT ( 'NONE',  ( -34.50000000000000000, -116.0141056290913610, -0.5935324770972248976 ) ) ;
#6513 = CARTESIAN_POINT ( 'NONE',  ( -35.50000000000000711, -112.0414288467712112, 1.115164475686276191 ) ) ;
#6514 = ORIENTED_EDGE ( 'NONE', *, *, #35277, .T. ) ;
#6515 = PRODUCT_DEFINITION_CONTEXT ( 'detailed design', #19717, 'design' ) ;
#6516 = ORIENTED_EDGE ( 'NONE', *, *, #1405, .T. ) ;
#6517 = DIRECTION ( 'NONE',  ( -1.000000000000000000, 0.000000000000000000, 0.000000000000000000 ) ) ;
#6518 = CIRCLE ( 'NONE', #1362, 8.000000000000001776 ) ;
#6519 = VECTOR ( 'NONE', #24387, 1000.000000000000000 ) ;
#6520 = ADVANCED_FACE ( 'NONE', ( #22737, #33732 ), #4042, .T. ) ;
#6521 = CARTESIAN_POINT ( 'NONE',  ( -37.89983305244309264, -113.9929510916434339, 12.92579853460519423 ) ) ;
#6522 = CARTESIAN_POINT ( 'NONE',  ( 4.000000000000003553, -10.46102064772325413, -19.35373470438994659 ) ) ;
#6523 = CARTESIAN_POINT ( 'NONE',  ( -35.50000000000000000, -113.9929510916434339, 10.72628538622835670 ) ) ;
#6524 = CARTESIAN_POINT ( 'NONE',  ( -35.50025087934803736, -115.9929510916434481, 12.63488142334835196 ) ) ;
#6525 = CARTESIAN_POINT ( 'NONE',  ( 5.400000000000085620, -1.000000000000049516, -40.00000000000000000 ) ) ;
#6527 = AXIS2_PLACEMENT_3D ( 'NONE', #9907, #6491, #12075 ) ;
#6526 = DIRECTION ( 'NONE',  ( 1.000000000000000000, 1.734723475976807094E-16, 0.000000000000000000 ) ) ;
#6528 = CIRCLE ( 'NONE', #9410, 8.000000000000007105 ) ;
#6529 = EDGE_CURVE ( 'NONE', #15756, #27135, #31981, .T. ) ;
#6530 = DIRECTION ( 'NONE',  ( -1.000000000000000000, -0.000000000000000000, -0.000000000000000000 ) ) ;
#6531 = CARTESIAN_POINT ( 'NONE',  ( -42.49999999999999289, -25.98076211353322051, 84.99999999999992895 ) ) ;
#6532 = CARTESIAN_POINT ( 'NONE',  ( -10.00000000000000178, 0.000000000000000000, 0.000000000000000000 ) ) ;
#6533 = VERTEX_POINT ( 'NONE', #22919 ) ;
#6534 = CARTESIAN_POINT ( 'NONE',  ( -55.00000000000000000, 19.99999999999998934, -15.00000000000001421 ) ) ;
#6535 = LINE ( 'NONE', #8879, #898 ) ;
#6536 = DIRECTION ( 'NONE',  ( 0.000000000000000000, 0.000000000000000000, -1.000000000000000000 ) ) ;
#6537 = DIRECTION ( 'NONE',  ( 1.000000000000000000, -0.000000000000000000, -0.000000000000000000 ) ) ;
#6538 = LINE ( 'NONE', #28512, #26808 ) ;
#6539 = FACE_OUTER_BOUND ( 'NONE', #6461, .T. ) ;
#6540 = CIRCLE ( 'NONE', #26671, 4.000000000000014211 ) ;
#6541 = EDGE_LOOP ( 'NONE', ( #26232, #26171, #9011, #1156 ) ) ;
#6542 = DIRECTION ( 'NONE',  ( 1.000000000000000000, -0.000000000000000000, -0.000000000000000000 ) ) ;
#6543 = CARTESIAN_POINT ( 'NONE',  ( -34.50000000000000000, -111.2666036476567655, -1.632210088999287212 ) ) ;
#6544 = DIRECTION ( 'NONE',  ( -1.000000000000000000, 0.000000000000000000, 0.000000000000000000 ) ) ;
#6545 = VERTEX_POINT ( 'NONE', #33912 ) ;
#6546 = VERTEX_POINT ( 'NONE', #7431 ) ;
#6547 = CARTESIAN_POINT ( 'NONE',  ( -35.99999999999999289, -113.9407375970686758, 8.496475545821549957 ) ) ;
#6548 = ORIENTED_EDGE ( 'NONE', *, *, #20713, .F. ) ;
#6549 = ORIENTED_EDGE ( 'NONE', *, *, #16114, .T. ) ;
#6550 = ORIENTED_EDGE ( 'NONE', *, *, #29747, .T. ) ;
#6551 = CARTESIAN_POINT ( 'NONE',  ( -34.50000000000000000, -113.0140978167136581, 0.8752176474015604946 ) ) ;
#6552 = VECTOR ( 'NONE', #18363, 1000.000000000000000 ) ;
#6553 = CARTESIAN_POINT ( 'NONE',  ( 70.00000000000001421, 58.35354061212520804, 76.25822877525452270 ) ) ;
#6554 = DIRECTION ( 'NONE',  ( 0.000000000000000000, 1.000000000000000000, 0.000000000000000000 ) ) ;
#6555 = EDGE_CURVE ( 'NONE', #33826, #7350, #3823, .T. ) ;
#6556 = CARTESIAN_POINT ( 'NONE',  ( -36.03906250000000000, -114.9929510916434339, 13.11852480586264669 ) ) ;
#6557 = CARTESIAN_POINT ( 'NONE',  ( 0.000000000000000000, -34.03046037009280411, 33.13733193845794034 ) ) ;
#6558 = EDGE_CURVE ( 'NONE', #29784, #1742, #16999, .T. ) ;
#6559 = CARTESIAN_POINT ( 'NONE',  ( 8.000000000000007105, 0.000000000000000000, 0.000000000000000000 ) ) ;
#6560 = CARTESIAN_POINT ( 'NONE',  ( -34.50000000000000000, -114.9929510916434339, 11.38636890470581164 ) ) ;
#6561 = DIRECTION ( 'NONE',  ( 0.000000000000000000, 0.000000000000000000, 1.000000000000000000 ) ) ;
#6562 = DIRECTION ( 'NONE',  ( 0.000000000000000000, 0.000000000000000000, 1.000000000000000000 ) ) ;
#6563 = ORIENTED_EDGE ( 'NONE', *, *, #13484, .F. ) ;
#6564 = EDGE_CURVE ( 'NONE', #4061, #169, #35437, .T. ) ;
#6565 = CARTESIAN_POINT ( 'NONE',  ( -39.00000000000000000, -115.9929510916434481, 12.39849696637031151 ) ) ;
#6566 = CARTESIAN_POINT ( 'NONE',  ( -35.50000000000000711, -112.7472371723319355, 1.839427296857320648 ) ) ;
#6567 = CARTESIAN_POINT ( 'NONE',  ( 8.000000000000000000, 14.48509162075973755, -8.733917826871222090 ) ) ;
#6568 = CARTESIAN_POINT ( 'NONE',  ( 0.000000000000000000, 0.000000000000000000, 0.000000000000000000 ) ) ;
#6569 = LINE ( 'NONE', #17546, #6695 ) ;
#6570 = EDGE_CURVE ( 'NONE', #22667, #29876, #26226, .T. ) ;
#6571 = FACE_OUTER_BOUND ( 'NONE', #883, .T. ) ;
#6572 = CARTESIAN_POINT ( 'NONE',  ( 0.000000000000000000, 0.000000000000000000, 0.000000000000000000 ) ) ;
#6573 = CIRCLE ( 'NONE', #16362, 8.000000000000003553 ) ;
#6574 = CIRCLE ( 'NONE', #27869, 20.00000000000000711 ) ;
#6575 = DIRECTION ( 'NONE',  ( -1.000000000000000000, -0.000000000000000000, -0.000000000000000000 ) ) ;
#6576 = CYLINDRICAL_SURFACE ( 'NONE', #34517, 9.499000000000000554 ) ;
#6577 = ORIENTED_EDGE ( 'NONE', *, *, #31132, .T. ) ;
#6578 = CARTESIAN_POINT ( 'NONE',  ( -36.94073759706868287, -115.0000000000000000, 8.871475545821548181 ) ) ;
#6579 = DIRECTION ( 'NONE',  ( 1.000000000000000000, 0.000000000000000000, 0.000000000000000000 ) ) ;
#6580 = CARTESIAN_POINT ( 'NONE',  ( 7.999999999999992895, 0.000000000000000000, 0.000000000000000000 ) ) ;
#6581 = CIRCLE ( 'NONE', #23261, 20.00000000000000711 ) ;
#6582 = EDGE_LOOP ( 'NONE', ( #23195, #14934, #21784, #17958 ) ) ;
#6583 = VERTEX_POINT ( 'NONE', #18588 ) ;
#6584 = DIRECTION ( 'NONE',  ( 1.000000000000000000, 0.000000000000000000, 0.000000000000000000 ) ) ;
#6585 = DIRECTION ( 'NONE',  ( 0.000000000000000000, -0.9848077530122063550, -0.1736481776669404342 ) ) ;
#6586 = ORIENTED_EDGE ( 'NONE', *, *, #29021, .T. ) ;
#6587 = CARTESIAN_POINT ( 'NONE',  ( -37.05926240293131713, -112.0000000000000142, 3.621475545821551290 ) ) ;
#6588 = ORIENTED_EDGE ( 'NONE', *, *, #14355, .F. ) ;
#6589 = ADVANCED_FACE ( 'NONE', ( #13024, #24013 ), #18409, .F. ) ;
#6590 = AXIS2_PLACEMENT_3D ( 'NONE', #11942, #3851, #4383 ) ;
#6591 = CARTESIAN_POINT ( 'NONE',  ( 4.000000000000000000, 4.898587196589412829E-16, -34.40000000000000568 ) ) ;
#6592 = CARTESIAN_POINT ( 'NONE',  ( 0.000000000000000000, 0.000000000000000000, 0.000000000000000000 ) ) ;
#6593 = SHAPE_DEFINITION_REPRESENTATION ( #20122, #5681 ) ;
#6594 = PLANE ( 'NONE',  #19626 ) ;
#6595 = ORIENTED_EDGE ( 'NONE', *, *, #35267, .T. ) ;
#6596 = ORIENTED_EDGE ( 'NONE', *, *, #16924, .F. ) ;
#6597 = CIRCLE ( 'NONE', #12941, 20.00000000000000000 ) ;
#6598 = EDGE_CURVE ( 'NONE', #33486, #13700, #14130, .T. ) ;
#6599 = AXIS2_PLACEMENT_3D ( 'NONE', #2846, #10935, #8218 ) ;
#6600 = DIRECTION ( 'NONE',  ( 0.000000000000000000, 0.000000000000000000, -1.000000000000000000 ) ) ;
#6601 = CARTESIAN_POINT ( 'NONE',  ( 46.00000000000000000, 0.000000000000000000, 59.00000000000000000 ) ) ;
#6602 = ADVANCED_FACE ( 'NONE', ( #7247 ), #4754, .T. ) ;
#6603 = EDGE_CURVE ( 'NONE', #8203, #32783, #33693, .T. ) ;
#6604 = ORIENTED_EDGE ( 'NONE', *, *, #29132, .T. ) ;
#6605 = CARTESIAN_POINT ( 'NONE',  ( -1.799999999999995604, -2.914335439641035426E-16, -4.200000000000014388 ) ) ;
#6606 = AXIS2_PLACEMENT_3D ( 'NONE', #33080, #32532, #5710 ) ;
#6607 = CARTESIAN_POINT ( 'NONE',  ( -34.50000000000000000, -113.6807644833805995, -0.6247823525984269599 ) ) ;
#6608 = FACE_OUTER_BOUND ( 'NONE', #29501, .T. ) ;
#6609 = FACE_OUTER_BOUND ( 'NONE', #20831, .T. ) ;
#6610 = CIRCLE ( 'NONE', #20968, 47.49900000000000944 ) ;
#6611 = CARTESIAN_POINT ( 'NONE',  ( -34.50000000000000000, -114.2183886307118428, 8.518969274377507617 ) ) ;
#6612 = DIRECTION ( 'NONE',  ( 0.000000000000000000, 0.000000000000000000, 1.000000000000000000 ) ) ;
#6613 = DIRECTION ( 'NONE',  ( -1.000000000000000000, 0.000000000000000000, 0.000000000000000000 ) ) ;
#6614 = EDGE_CURVE ( 'NONE', #8976, #12699, #21282, .T. ) ;
#6615 = CARTESIAN_POINT ( 'NONE',  ( -39.00000000000000711, -114.9929510916434339, 12.60752341388803721 ) ) ;
#6616 = CARTESIAN_POINT ( 'NONE',  ( 4.000000000000000000, 4.898587196589412829E-16, -40.40000000000000568 ) ) ;
#6617 = EDGE_CURVE ( 'NONE', #20180, #15866, #9539, .T. ) ;
#6618 = DIRECTION ( 'NONE',  ( -1.047965281155519913E-16, -6.938893903907192632E-17, -1.000000000000000000 ) ) ;
#6619 = VECTOR ( 'NONE', #22508, 1000.000000000000000 ) ;
#6620 = DIRECTION ( 'NONE',  ( 0.000000000000000000, 0.000000000000000000, 1.000000000000000000 ) ) ;
#6621 = FACE_OUTER_BOUND ( 'NONE', #22618, .T. ) ;
#6622 = DIRECTION ( 'NONE',  ( -1.000000000000000000, 0.000000000000000000, 0.000000000000000000 ) ) ;
#6623 = VERTEX_POINT ( 'NONE', #23466 ) ;
#6624 = CARTESIAN_POINT ( 'NONE',  ( -39.99999999999999289, -114.0592624029313242, 3.246475545821551734 ) ) ;
#6625 = CARTESIAN_POINT ( 'NONE',  ( 8.000000000000000000, 16.94522934049215124, 8.128228055638924587 ) ) ;
#6626 = CARTESIAN_POINT ( 'NONE',  ( -35.50000000000000000, -113.7503824761461004, 0.9631051547057219997 ) ) ;
#6627 = VERTEX_POINT ( 'NONE', #23647 ) ;
#6628 = ORIENTED_EDGE ( 'NONE', *, *, #13462, .F. ) ;
#6630 = CARTESIAN_POINT ( 'NONE',  ( -9.999999999999994671, 0.000000000000000000, 0.000000000000000000 ) ) ;
#6629 = PRODUCT_DEFINITION_SHAPE ( 'NONE', 'NONE',  #35635 ) ;
#6631 = VECTOR ( 'NONE', #20373, 1000.000000000000000 ) ;
#6632 = CARTESIAN_POINT ( 'NONE',  ( -1.599999999999990319, 0.000000000000000000, 0.000000000000000000 ) ) ;
#6633 = VERTEX_POINT ( 'NONE', #26896 ) ;
#6634 = ORIENTED_EDGE ( 'NONE', *, *, #9173, .T. ) ;
#6635 = EDGE_CURVE ( 'NONE', #25674, #1552, #35001, .T. ) ;
#6636 = AXIS2_PLACEMENT_3D ( 'NONE', #32322, #23874, #34501 ) ;
#6637 = LINE ( 'NONE', #6463, #16528 ) ;
#6639 = ORIENTED_EDGE ( 'NONE', *, *, #25303, .F. ) ;
#6638 = EDGE_CURVE ( 'NONE', #2406, #22936, #7071, .T. ) ;
#6640 = CARTESIAN_POINT ( 'NONE',  ( -38.37230871539094323, -115.4561184093552413, 3.058975545821551290 ) ) ;
#6641 = EDGE_CURVE ( 'NONE', #9660, #1640, #19866, .T. ) ;
#6642 = DIRECTION ( 'NONE',  ( -1.000000000000000000, 0.000000000000000000, 0.000000000000000000 ) ) ;
#6643 = DIRECTION ( 'NONE',  ( 0.000000000000000000, 0.000000000000000000, -1.000000000000000000 ) ) ;
#6645 = ORIENTED_EDGE ( 'NONE', *, *, #28721, .F. ) ;
#6644 = AXIS2_PLACEMENT_3D ( 'NONE', #8440, #33291, #8609 ) ;
#6646 = EDGE_LOOP ( 'NONE', ( #7286, #1200 ) ) ;
#6647 = CARTESIAN_POINT ( 'NONE',  ( -35.50000000000000000, -112.9650106922503170, -2.624765990393421955 ) ) ;
#6648 = EDGE_CURVE ( 'NONE', #7361, #16353, #29410, .T. ) ;
#6649 = EDGE_CURVE ( 'NONE', #19114, #20656, #17591, .T. ) ;
#6650 = CARTESIAN_POINT ( 'NONE',  ( 8.000000000000000000, -11.06713717293229138, -13.55483219355740765 ) ) ;
#6651 = ORIENTED_EDGE ( 'NONE', *, *, #28678, .F. ) ;
#6652 = CARTESIAN_POINT ( 'NONE',  ( -38.00000000000000711, -114.9929510916434339, 12.44250253426874941 ) ) ;
#6653 = CARTESIAN_POINT ( 'NONE',  ( -34.50000000000000000, -114.0928965812550757, 9.511088712577292270 ) ) ;
#6654 = FACE_OUTER_BOUND ( 'NONE', #162, .T. ) ;
#6655 = DIRECTION ( 'NONE',  ( 0.000000000000000000, 0.000000000000000000, 1.000000000000000000 ) ) ;
#6656 = CARTESIAN_POINT ( 'NONE',  ( -38.98077402996267438, -113.9929510916434339, 12.86289566494346204 ) ) ;
#6657 = DIRECTION ( 'NONE',  ( 0.000000000000000000, -0.3681245526846654292, -0.9297764858882562322 ) ) ;
#6658 = AXIS2_PLACEMENT_3D ( 'NONE', #12488, #1689, #17874 ) ;
#6659 = EDGE_CURVE ( 'NONE', #6941, #2467, #8961, .T. ) ;
#6660 = CARTESIAN_POINT ( 'NONE',  ( -36.99999999999989342, -114.9929510916434339, 13.11852480586264669 ) ) ;
#6661 = DIRECTION ( 'NONE',  ( 0.000000000000000000, 0.000000000000000000, 1.000000000000000000 ) ) ;
#6662 = ORIENTED_EDGE ( 'NONE', *, *, #30229, .F. ) ;
#6663 = AXIS2_PLACEMENT_3D ( 'NONE', #33594, #8927, #9115 ) ;
#6664 = DIRECTION ( 'NONE',  ( 0.000000000000000000, 0.000000000000000000, -1.000000000000000000 ) ) ;
#6665 = CARTESIAN_POINT ( 'NONE',  ( 0.000000000000000000, 0.2227391519123156360, -46.98410307550729215 ) ) ;
#6666 = ORIENTED_EDGE ( 'NONE', *, *, #3131, .F. ) ;
#6667 = CARTESIAN_POINT ( 'NONE',  ( -35.50000000000000711, -114.9927795562974069, 10.48735431211914815 ) ) ;
#6668 = ORIENTED_EDGE ( 'NONE', *, *, #7227, .T. ) ;
#6669 = FACE_OUTER_BOUND ( 'NONE', #9469, .T. ) ;
#6670 = STYLED_ITEM ( 'NONE', ( #789 ), #34526 ) ;
#6671 = ORIENTED_EDGE ( 'NONE', *, *, #10411, .T. ) ;
#6672 = CARTESIAN_POINT ( 'NONE',  ( 0.000000000000000000, 9.433698091065215507, 1.111908866155128628 ) ) ;
#6673 = EDGE_LOOP ( 'NONE', ( #6459, #28530, #2256, #34420 ) ) ;
#6674 = CARTESIAN_POINT ( 'NONE',  ( -35.50000000000000000, -114.6807644833805000, -0.6247823525984269599 ) ) ;
#6675 = PLANE ( 'NONE',  #19605 ) ;
#6676 = DIRECTION ( 'NONE',  ( -0.9997917317482359900, -0.02040816326530611735, 3.453951567998058470E-31 ) ) ;
#6677 = EDGE_LOOP ( 'NONE', ( #31133, #10041, #15314, #20296 ) ) ;
#6678 = CARTESIAN_POINT ( 'NONE',  ( -34.97545270896703329, -113.2308352781851539, 4.409774454178448266 ) ) ;
#6679 = EDGE_CURVE ( 'NONE', #21338, #18999, #13578, .T. ) ;
#6680 = EDGE_CURVE ( 'NONE', #16000, #2330, #2240, .T. ) ;
#6681 = CARTESIAN_POINT ( 'NONE',  ( 3.239593890920905217, -13.56862304811760822, -1.200000000000006617 ) ) ;
#6682 = VECTOR ( 'NONE', #35175, 1000.000000000000000 ) ;
#6683 = CARTESIAN_POINT ( 'NONE',  ( -35.50000000000000711, -112.0140978167138712, -0.4997823525984337878 ) ) ;
#6684 = VERTEX_POINT ( 'NONE', #5801 ) ;
#6685 = VERTEX_POINT ( 'NONE', #5970 ) ;
#6686 = DIRECTION ( 'NONE',  ( 0.000000000000000000, 0.000000000000000000, 1.000000000000000000 ) ) ;
#6687 = AXIS2_PLACEMENT_3D ( 'NONE', #21446, #13723, #2573 ) ;
#6688 = CIRCLE ( 'NONE', #20471, 4.800000000000005151 ) ;
#6689 = DIRECTION ( 'NONE',  ( -1.000000000000000000, 0.000000000000000000, 0.000000000000000000 ) ) ;
#6690 = VERTEX_POINT ( 'NONE', #27420 ) ;
#6691 = VERTEX_POINT ( 'NONE', #19113 ) ;
#6692 = CARTESIAN_POINT ( 'NONE',  ( -34.50000000000000000, -116.0140978167138712, -0.1247823525984439463 ) ) ;
#6693 = CIRCLE ( 'NONE', #26837, 47.49900000000001654 ) ;
#6694 = CARTESIAN_POINT ( 'NONE',  ( -35.50000000000000711, -113.2637153405686519, 1.912112492696748989 ) ) ;
#6695 = VECTOR ( 'NONE', #28552, 1000.000000000000000 ) ;
#6696 = EDGE_CURVE ( 'NONE', #19390, #24892, #11029, .T. ) ;
#6697 = VERTEX_POINT ( 'NONE', #22166 ) ;
#6698 = ORIENTED_EDGE ( 'NONE', *, *, #24435, .T. ) ;
#6699 = EDGE_CURVE ( 'NONE', #6952, #33344, #32540, .T. ) ;
#6700 = AXIS2_PLACEMENT_3D ( 'NONE', #29243, #21109, #29416 ) ;
#6701 = DIRECTION ( 'NONE',  ( 0.000000000000000000, 0.000000000000000000, 1.000000000000000000 ) ) ;
#6702 = CARTESIAN_POINT ( 'NONE',  ( -35.56312645773537895, -113.9929510916434339, 12.87038173996308998 ) ) ;
#6703 = CARTESIAN_POINT ( 'NONE',  ( 0.000000000000000000, -24.72041153920704915, -40.55929306992714345 ) ) ;
#6704 = CARTESIAN_POINT ( 'NONE',  ( -35.50000000000000000, -113.9929510916434339, 12.39849696637031684 ) ) ;
#6705 = CARTESIAN_POINT ( 'NONE',  ( -35.50000000000000000, -115.9929510916434481, 11.38636890470581164 ) ) ;
#6706 = UNCERTAINTY_MEASURE_WITH_UNIT (LENGTH_MEASURE( 1.000000000000000082E-05 ), #29466, 'distance_accuracy_value', 'NONE');
#6707 = CARTESIAN_POINT ( 'NONE',  ( 112.0000000000000000, 81.48267994499606459, 22.65054357219659664 ) ) ;
#6708 = FACE_OUTER_BOUND ( 'NONE', #7538, .T. ) ;
#6709 = AXIS2_PLACEMENT_3D ( 'NONE', #13898, #24886, #8661 ) ;
#6710 = FACE_OUTER_BOUND ( 'NONE', #1735, .T. ) ;
#6711 = DIRECTION ( 'NONE',  ( 0.000000000000000000, -0.9510565162951500895, -0.3090169943749579429 ) ) ;
#6712 = FACE_OUTER_BOUND ( 'NONE', #31261, .T. ) ;
#6713 = AXIS2_PLACEMENT_3D ( 'NONE', #1018, #30898, #34136 ) ;
#6714 = ORIENTED_EDGE ( 'NONE', *, *, #22194, .T. ) ;
#6715 = AXIS2_PLACEMENT_3D ( 'NONE', #22348, #33343, #568 ) ;
#6716 = CARTESIAN_POINT ( 'NONE',  ( 7.999999999999992895, 36.05989434073656241, -30.12041790338579261 ) ) ;
#6717 = DIRECTION ( 'NONE',  ( 0.000000000000000000, 0.3681245526846718685, 0.9297764858882537897 ) ) ;
#6718 = LINE ( 'NONE', #971, #2355 ) ;
#6719 = CIRCLE ( 'NONE', #26869, 20.00000000000000711 ) ;
#6720 = AXIS2_PLACEMENT_3D ( 'NONE', #19550, #33793, #11466 ) ;
#6721 = CIRCLE ( 'NONE', #11337, 7.199999999999998401 ) ;
#6722 = CARTESIAN_POINT ( 'NONE',  ( 0.000000000000000000, -18.62763138773852134, 10.49404041845529001 ) ) ;
#6723 = DIRECTION ( 'NONE',  ( -1.000000000000000000, 0.000000000000000000, 0.000000000000000000 ) ) ;
#6724 = AXIS2_PLACEMENT_3D ( 'NONE', #30154, #27468, #7640 ) ;
#6725 = ORIENTED_EDGE ( 'NONE', *, *, #12153, .T. ) ;
#6726 = ADVANCED_FACE ( 'NONE', ( #40 ), #5450, .T. ) ;
#6727 = FACE_OUTER_BOUND ( 'NONE', #914, .T. ) ;
#6728 = CARTESIAN_POINT ( 'NONE',  ( -34.50000000000000000, -114.9515981487115823, -2.624803185604625000 ) ) ;
#6729 = CARTESIAN_POINT ( 'NONE',  ( 0.000000000000000000, 17.08890430202814059, -43.76671000081924490 ) ) ;
#6730 = ORIENTED_EDGE ( 'NONE', *, *, #10860, .T. ) ;
#6731 = EDGE_LOOP ( 'NONE', ( #19453, #23229, #34731, #21837 ) ) ;
#6732 = CARTESIAN_POINT ( 'NONE',  ( -37.47347596530441649, -114.9754527089670262, 1.972274454178448932 ) ) ;
#6733 = ORIENTED_EDGE ( 'NONE', *, *, #16996, .T. ) ;
#6734 = AXIS2_PLACEMENT_3D ( 'NONE', #8385, #19368, #5702 ) ;
#6735 = ORIENTED_EDGE ( 'NONE', *, *, #11682, .F. ) ;
#6736 = ORIENTED_EDGE ( 'NONE', *, *, #26085, .T. ) ;
#6737 = CARTESIAN_POINT ( 'NONE',  ( -35.50000000000000000, -113.0349311500474982, -0.6247823525985715110 ) ) ;
#6738 = AXIS2_PLACEMENT_3D ( 'NONE', #5136, #10518, #21480 ) ;
#6739 = LINE ( 'NONE', #29429, #30431 ) ;
#6740 = AXIS2_PLACEMENT_3D ( 'NONE', #34703, #24254, #1939 ) ;
#6741 = VECTOR ( 'NONE', #27815, 1000.000000000000000 ) ;
#6742 = VECTOR ( 'NONE', #16901, 1000.000000000000000 ) ;
#6743 = CARTESIAN_POINT ( 'NONE',  ( -35.50000000000000711, -114.9929510916434339, 11.21034663311131929 ) ) ;
#6744 = CARTESIAN_POINT ( 'NONE',  ( 0.000000000000000000, 47.32430374665932504, 21.55018039121545215 ) ) ;
#6745 = AXIS2_PLACEMENT_3D ( 'NONE', #33258, #14495, #28209 ) ;
#6746 = CYLINDRICAL_SURFACE ( 'NONE', #6819, 9.499000000000000554 ) ;
#6747 = CARTESIAN_POINT ( 'NONE',  ( -37.46874999999996447, -114.9929510916434339, 14.11852480586264846 ) ) ;
#6748 = FACE_OUTER_BOUND ( 'NONE', #14259, .T. ) ;
#6749 = DIRECTION ( 'NONE',  ( -1.000000000000000000, 0.000000000000000000, 0.000000000000000000 ) ) ;
#6750 = ORIENTED_EDGE ( 'NONE', *, *, #29774, .T. ) ;
#6751 = CARTESIAN_POINT ( 'NONE',  ( -35.50000000000000000, -115.9929510916434481, 10.85830208992344303 ) ) ;
#6752 = CARTESIAN_POINT ( 'NONE',  ( -35.50000000000000711, -112.0140978167138712, -0.4685323525984295134 ) ) ;
#6753 = DIRECTION ( 'NONE',  ( 0.000000000000000000, 0.000000000000000000, 1.000000000000000000 ) ) ;
#6754 = CARTESIAN_POINT ( 'NONE',  ( 0.000000000000000000, -6.860320204751236162, 13.89802171851381551 ) ) ;
#6755 = LINE ( 'NONE', #34131, #17037 ) ;
#6756 = VECTOR ( 'NONE', #8698, 1000.000000000000000 ) ;
#6757 = DIRECTION ( 'NONE',  ( 0.000000000000000000, -6.938893903907202493E-17, -1.000000000000000000 ) ) ;
#6758 = DIRECTION ( 'NONE',  ( 0.000000000000000000, -0.4999999999999888978, -0.8660254037844450359 ) ) ;
#6759 = CIRCLE ( 'NONE', #21692, 0.7500000000000006661 ) ;
#6760 = DIRECTION ( 'NONE',  ( 0.000000000000000000, -1.000000000000000000, 0.000000000000000000 ) ) ;
#6761 = DIRECTION ( 'NONE',  ( 1.000000000000000000, 0.000000000000000000, 0.000000000000000000 ) ) ;
#6762 = ORIENTED_EDGE ( 'NONE', *, *, #3308, .T. ) ;
#6763 = CARTESIAN_POINT ( 'NONE',  ( -36.02454729103297382, -113.5265240346956261, 6.902725545821551734 ) ) ;
#6764 = AXIS2_PLACEMENT_3D ( 'NONE', #15950, #13279, #21519 ) ;
#6765 = DIRECTION ( 'NONE',  ( 0.000000000000000000, 0.000000000000000000, -1.000000000000000000 ) ) ;
#6766 = CIRCLE ( 'NONE', #24617, 22.00000000000000000 ) ;
#6767 = CARTESIAN_POINT ( 'NONE',  ( 1.599999999999990319, 0.000000000000000000, 0.000000000000000000 ) ) ;
#6768 = ORIENTED_EDGE ( 'NONE', *, *, #13286, .F. ) ;
#6769 = ORIENTED_EDGE ( 'NONE', *, *, #33030, .F. ) ;
#6770 = VECTOR ( 'NONE', #32379, 1000.000000000000000 ) ;
#6771 = EDGE_CURVE ( 'NONE', #31595, #26460, #27065, .T. ) ;
#6772 = FILL_AREA_STYLE ('',( #18098 ) ) ;
#6773 = CARTESIAN_POINT ( 'NONE',  ( 0.000000000000000000, 0.000000000000000000, 0.000000000000000000 ) ) ;
#6774 = EDGE_LOOP ( 'NONE', ( #2512, #3235, #14123, #24497 ) ) ;
#6775 = CARTESIAN_POINT ( 'NONE',  ( -34.92058450342249643, -111.8367748094582197, 5.308975545821551734 ) ) ;
#6776 = ORIENTED_EDGE ( 'NONE', *, *, #11610, .T. ) ;
#6777 = CIRCLE ( 'NONE', #11388, 6.000000000000005329 ) ;
#6778 = DIRECTION ( 'NONE',  ( -1.000000000000000000, 0.000000000000000000, 0.000000000000000000 ) ) ;
#6779 = DIRECTION ( 'NONE',  ( 0.000000000000000000, 0.000000000000000000, -1.000000000000000000 ) ) ;
#6780 = DIRECTION ( 'NONE',  ( -1.000000000000000000, -0.000000000000000000, -0.000000000000000000 ) ) ;
#6781 = EDGE_CURVE ( 'NONE', #2812, #32201, #27240, .T. ) ;
#6782 = SHAPE_DEFINITION_REPRESENTATION ( #23303, #33958 ) ;
#6783 = DIRECTION ( 'NONE',  ( -1.000000000000000000, 0.000000000000000000, -0.000000000000000000 ) ) ;
#6784 = VERTEX_POINT ( 'NONE', #21815 ) ;
#6785 = ORIENTED_EDGE ( 'NONE', *, *, #32376, .F. ) ;
#6786 = CARTESIAN_POINT ( 'NONE',  ( 0.000000000000000000, 5.400000000000000355, 0.9999999999999985567 ) ) ;
#6787 = DIRECTION ( 'NONE',  ( -1.000000000000000000, 0.000000000000000000, -0.000000000000000000 ) ) ;
#6788 = EDGE_LOOP ( 'NONE', ( #16668, #27613, #31091, #16967 ) ) ;
#6789 = DIRECTION ( 'NONE',  ( 0.000000000000000000, 0.000000000000000000, 1.000000000000000000 ) ) ;
#6790 = CARTESIAN_POINT ( 'NONE',  ( -34.50000000000000000, -112.6043641208289188, 1.789429170677330649 ) ) ;
#6791 = CARTESIAN_POINT ( 'NONE',  ( -3.799999999999999822, 4.382607293638566128E-16, -30.00000000000000711 ) ) ;
#6792 = FACE_OUTER_BOUND ( 'NONE', #32560, .T. ) ;
#6793 = VECTOR ( 'NONE', #25345, 1000.000000000000000 ) ;
#6794 = CARTESIAN_POINT ( 'NONE',  ( -36.03906250000000000, -115.9929510916434481, 14.11852480586265024 ) ) ;
#6795 = CYLINDRICAL_SURFACE ( 'NONE', #11706, 4.000000000000000000 ) ;
#6796 = DIRECTION ( 'NONE',  ( 0.000000000000000000, 0.000000000000000000, -1.000000000000000000 ) ) ;
#6797 = CARTESIAN_POINT ( 'NONE',  ( -34.50000000000000000, -114.2207110452431635, 8.519246492191951958 ) ) ;
#6798 = DIRECTION ( 'NONE',  ( -1.000000000000000000, 0.000000000000000000, 0.000000000000000000 ) ) ;
#6799 = CIRCLE ( 'NONE', #31537, 20.00000000000000711 ) ;
#6800 = EDGE_CURVE ( 'NONE', #7480, #4435, #25664, .T. ) ;
#6801 = DIRECTION ( 'NONE',  ( -1.000000000000000000, 0.000000000000000000, 0.000000000000000000 ) ) ;
#6802 = CARTESIAN_POINT ( 'NONE',  ( -21.15833593587365513, -37.35511776651544125, 93.29903810567650169 ) ) ;
#6803 = CYLINDRICAL_SURFACE ( 'NONE', #22103, 4.000000000000003553 ) ;
#6804 = PLANE ( 'NONE',  #19326 ) ;
#6805 = ORIENTED_EDGE ( 'NONE', *, *, #20272, .T. ) ;
#6806 = CARTESIAN_POINT ( 'NONE',  ( -34.83677480945821259, -116.0794154965774965, 4.183975545821551734 ) ) ;
#6807 = CARTESIAN_POINT ( 'NONE',  ( 0.000000000000000000, -2.710505431213761085E-17, 45.99999999999998579 ) ) ;
#6808 = CARTESIAN_POINT ( 'NONE',  ( -35.50000000000000000, -112.9990795116828650, 0.8734249692896993711 ) ) ;
#6809 = ORIENTED_EDGE ( 'NONE', *, *, #25817, .T. ) ;
#6810 = ORIENTED_EDGE ( 'NONE', *, *, #1121, .F. ) ;
#6811 = EDGE_CURVE ( 'NONE', #4231, #34564, #23945, .T. ) ;
#6812 = DIRECTION ( 'NONE',  ( 0.000000000000000000, 0.000000000000000000, -1.000000000000000000 ) ) ;
#6813 = CARTESIAN_POINT ( 'NONE',  ( 70.00000000000001421, 45.53424681125909501, 59.69714175238111409 ) ) ;
#6814 = ORIENTED_EDGE ( 'NONE', *, *, #20259, .F. ) ;
#6815 = EDGE_CURVE ( 'NONE', #20492, #13488, #8405, .T. ) ;
#6816 = EDGE_CURVE ( 'NONE', #26672, #8935, #2938, .T. ) ;
#6817 = ORIENTED_EDGE ( 'NONE', *, *, #13105, .T. ) ;
#6818 = ORIENTED_EDGE ( 'NONE', *, *, #4238, .F. ) ;
#6819 = AXIS2_PLACEMENT_3D ( 'NONE', #6559, #17534, #3889 ) ;
#6820 = AXIS2_PLACEMENT_3D ( 'NONE', #1520, #2071, #7273 ) ;
#6821 = DIRECTION ( 'NONE',  ( -1.000000000000000000, -0.000000000000000000, -0.000000000000000000 ) ) ;
#6822 = CARTESIAN_POINT ( 'NONE',  ( -39.02454729103295961, -113.2308352781851397, 7.840225545821551734 ) ) ;
#6823 = EDGE_CURVE ( 'NONE', #31834, #19156, #19284, .T. ) ;
#6824 = CARTESIAN_POINT ( 'NONE',  ( 0.000000000000000000, 0.000000000000000000, 0.000000000000000000 ) ) ;
#6825 = EDGE_CURVE ( 'NONE', #20308, #27386, #13025, .T. ) ;
#6826 = LINE ( 'NONE', #9350, #31114 ) ;
#6827 = ORIENTED_EDGE ( 'NONE', *, *, #23440, .T. ) ;
#6828 = ORIENTED_EDGE ( 'NONE', *, *, #26966, .T. ) ;
#6829 = CARTESIAN_POINT ( 'NONE',  ( -35.50000000000000000, -112.4957190293567066, -2.560864217808777266 ) ) ;
#6830 = DIRECTION ( 'NONE',  ( -1.000000000000000000, 0.000000000000000000, 0.000000000000000000 ) ) ;
#6831 = CARTESIAN_POINT ( 'NONE',  ( 7.999999999999992895, 6.109652351741788223, 46.58570277113510372 ) ) ;
#6832 = ORIENTED_EDGE ( 'NONE', *, *, #9532, .F. ) ;
#6833 = LINE ( 'NONE', #26469, #12038 ) ;
#6834 = CARTESIAN_POINT ( 'NONE',  ( -37.43749999999998579, -113.9929510916434339, 14.11852480586265024 ) ) ;
#6835 = DIRECTION ( 'NONE',  ( -1.000000000000000000, 5.339440136655842133E-16, -1.047965281155515476E-16 ) ) ;
#6836 = AXIS2_PLACEMENT_3D ( 'NONE', #22756, #28002, #33754 ) ;
#6837 = DIRECTION ( 'NONE',  ( -1.000000000000000000, -0.000000000000000000, -0.000000000000000000 ) ) ;
#6838 = CARTESIAN_POINT ( 'NONE',  ( -39.00000000000000000, -113.9929510916434339, 12.59652202191340820 ) ) ;
#6839 = DIRECTION ( 'NONE',  ( -1.000000000000000000, 0.000000000000000000, -0.000000000000000000 ) ) ;
#6840 = EDGE_CURVE ( 'NONE', #22842, #3725, #15846, .T. ) ;
#6841 = CARTESIAN_POINT ( 'NONE',  ( -35.51597953369718397, -114.9929510916434339, 12.74811950270164473 ) ) ;
#6842 = CYLINDRICAL_SURFACE ( 'NONE', #17058, 8.000000000000000000 ) ;
#6843 = ORIENTED_EDGE ( 'NONE', *, *, #21312, .T. ) ;
#6844 = CARTESIAN_POINT ( 'NONE',  ( -35.00000000000000000, -113.9407375970690310, 9.996475545821589037 ) ) ;
#6845 = DIRECTION ( 'NONE',  ( -1.000000000000000000, 0.000000000000000000, 0.000000000000000000 ) ) ;
#6846 = ORIENTED_EDGE ( 'NONE', *, *, #33935, .F. ) ;
#6847 = PRODUCT_DEFINITION ( 'UNKNOWN', '', #18955, #6515 ) ;
#6848 = CARTESIAN_POINT ( 'NONE',  ( -35.50000000000000711, -114.9929510916434339, 11.73841344789270202 ) ) ;
#6849 = VERTEX_POINT ( 'NONE', #30293 ) ;
#6850 = CARTESIAN_POINT ( 'NONE',  ( -38.37230871539094323, -112.5438815906447729, 2.441024454178448710 ) ) ;
#6851 = VERTEX_POINT ( 'NONE', #32812 ) ;
#6852 = CARTESIAN_POINT ( 'NONE',  ( 7.999999999999992895, 3.840921266749832252, 47.34345070675172451 ) ) ;
#6853 = ORIENTED_EDGE ( 'NONE', *, *, #14960, .T. ) ;
#6854 = ADVANCED_FACE ( 'NONE', ( #11382 ), #30636, .T. ) ;
#6855 = CARTESIAN_POINT ( 'NONE',  ( -34.50000000000000000, -113.0140978167138712, 0.8752176474015934682 ) ) ;
#6856 = DIRECTION ( 'NONE',  ( -1.783119874454246424E-31, -1.187911941725854497E-31, 1.000000000000000000 ) ) ;
#6857 = CARTESIAN_POINT ( 'NONE',  ( -38.97545270896704039, -113.1123104723225197, 6.847274454178450931 ) ) ;
#6858 = EDGE_CURVE ( 'NONE', #15170, #3677, #4955, .T. ) ;
#6859 = EDGE_CURVE ( 'NONE', #30484, #20884, #22790, .T. ) ;
#6860 = VERTEX_POINT ( 'NONE', #13548 ) ;
#6861 = CARTESIAN_POINT ( 'NONE',  ( -35.62769128460905677, -115.4561184093552413, 3.191024454178449155 ) ) ;
#6862 = APPLICATION_CONTEXT ( 'automotive_design' ) ;
#6863 = CARTESIAN_POINT ( 'NONE',  ( 0.000000000000000000, 0.000000000000000000, 0.000000000000000000 ) ) ;
#6864 = CARTESIAN_POINT ( 'NONE',  ( -35.50000000000000711, -112.3995503592287690, -1.424448457485529618 ) ) ;
#6865 = EDGE_LOOP ( 'NONE', ( #29214, #1596, #391, #13334 ) ) ;
#6866 = EDGE_LOOP ( 'NONE', ( #3485, #23747, #12315, #18680 ) ) ;
#6867 = FACE_OUTER_BOUND ( 'NONE', #11907, .T. ) ;
#6868 = VECTOR ( 'NONE', #999, 1000.000000000000000 ) ;
#6869 = EDGE_CURVE ( 'NONE', #34870, #7845, #35527, .T. ) ;
#6870 = DIRECTION ( 'NONE',  ( -1.000000000000000000, 0.000000000000000000, -0.000000000000000000 ) ) ;
#6871 = ORIENTED_EDGE ( 'NONE', *, *, #13263, .T. ) ;
#6872 = ORIENTED_EDGE ( 'NONE', *, *, #10606, .T. ) ;
#6873 = CIRCLE ( 'NONE', #32196, 47.49900000000001654 ) ;
#6874 = CARTESIAN_POINT ( 'NONE',  ( -34.50000000000000000, -116.0012805033554883, -0.7876962586524312027 ) ) ;
#6875 = CARTESIAN_POINT ( 'NONE',  ( -34.49999999999998579, -4.676198662292047281, 104.0227405789415798 ) ) ;
#6876 = AXIS2_PLACEMENT_3D ( 'NONE', #10315, #27059, #27236 ) ;
#6877 = AXIS2_PLACEMENT_3D ( 'NONE', #21215, #5214, #32380 ) ;
#6878 = ORIENTED_EDGE ( 'NONE', *, *, #22301, .T. ) ;
#6879 = VERTEX_POINT ( 'NONE', #10855 ) ;
#6880 = CIRCLE ( 'NONE', #27024, 2.999999999999988898 ) ;
#6881 = CARTESIAN_POINT ( 'NONE',  ( 0.000000000000000000, 0.000000000000000000, 0.000000000000000000 ) ) ;
#6882 = CARTESIAN_POINT ( 'NONE',  ( -35.95915003344518368, -113.9929510916434339, 13.11692036158763308 ) ) ;
#6883 = CARTESIAN_POINT ( 'NONE',  ( 8.000000000000000000, -14.48509162075970202, 8.733917826871310908 ) ) ;
#6884 = CARTESIAN_POINT ( 'NONE',  ( -35.50400759022158326, -113.9929510916434339, 12.68378527132497524 ) ) ;
#6885 = EDGE_CURVE ( 'NONE', #31265, #6533, #8133, .T. ) ;
#6886 = CARTESIAN_POINT ( 'NONE',  ( -35.50000000000000000, -115.3279708130221479, 8.997521329298534098 ) ) ;
#6887 = DIRECTION ( 'NONE',  ( 0.000000000000000000, 0.000000000000000000, 1.000000000000000000 ) ) ;
#6888 = DIRECTION ( 'NONE',  ( -1.174092375852890260E-15, 4.222049128630259891E-16, 1.000000000000000000 ) ) ;
#6889 = ADVANCED_FACE ( 'NONE', ( #16929 ), #735, .T. ) ;
#6890 = CYLINDRICAL_SURFACE ( 'NONE', #24611, 20.00000000000000711 ) ;
#6891 = DIRECTION ( 'NONE',  ( 0.000000000000000000, 0.000000000000000000, -1.000000000000000000 ) ) ;
#6892 = CARTESIAN_POINT ( 'NONE',  ( 0.000000000000000000, 14.30000000000000071, -3.000000000000002665 ) ) ;
#6893 = ORIENTED_EDGE ( 'NONE', *, *, #22907, .F. ) ;
#6894 = AXIS2_PLACEMENT_3D ( 'NONE', #32573, #32753, #5231 ) ;
#6895 = CARTESIAN_POINT ( 'NONE',  ( 4.000000000000000000, -17.06000345190446055, 10.43821259704015603 ) ) ;
#6896 = CARTESIAN_POINT ( 'NONE',  ( -35.50000000000000711, -113.2224311500466030, -1.624782352598427959 ) ) ;
#6897 = CARTESIAN_POINT ( 'NONE',  ( -34.49999999999998579, -29.98076211353321341, 84.99999999999994316 ) ) ;
#6898 = EDGE_CURVE ( 'NONE', #3192, #1965, #7277, .T. ) ;
#6899 = CONTEXT_DEPENDENT_SHAPE_REPRESENTATION ( #20454, #35155 ) ;
#6900 = CIRCLE ( 'NONE', #18388, 47.49900000000003075 ) ;
#6901 = EDGE_LOOP ( 'NONE', ( #17611, #4639, #24134, #32203 ) ) ;
#6902 = EDGE_CURVE ( 'NONE', #12983, #5428, #26856, .T. ) ;
#6903 = AXIS2_PLACEMENT_3D ( 'NONE', #23940, #5389, #2517 ) ;
#6904 = CARTESIAN_POINT ( 'NONE',  ( -1.799999999999996936, 1.496458227839707357E-15, 7.800000000000051337 ) ) ;
#6905 = CARTESIAN_POINT ( 'NONE',  ( -39.49999999999999289, -12.79398423610758684, 91.86693750936007064 ) ) ;
#6906 = ORIENTED_EDGE ( 'NONE', *, *, #28725, .F. ) ;
#6907 = CARTESIAN_POINT ( 'NONE',  ( 7.999999999999992895, 0.000000000000000000, 0.000000000000000000 ) ) ;
#6908 = CARTESIAN_POINT ( 'NONE',  ( -34.50000000000000000, -115.1449503510569059, -2.621568770093253953 ) ) ;
#6909 = CARTESIAN_POINT ( 'NONE',  ( 8.000000000000000000, 0.000000000000000000, 0.000000000000000000 ) ) ;
#6910 = EDGE_LOOP ( 'NONE', ( #24221, #6805, #4135, #5086 ) ) ;
#6911 = ORIENTED_EDGE ( 'NONE', *, *, #29058, .T. ) ;
#6912 = CARTESIAN_POINT ( 'NONE',  ( -35.97545270896705460, -114.3549511594417680, 8.590225545821549957 ) ) ;
#6913 = ORIENTED_EDGE ( 'NONE', *, *, #19760, .F. ) ;
#6914 = VERTEX_POINT ( 'NONE', #20334 ) ;
#6915 = VERTEX_POINT ( 'NONE', #28294 ) ;
#6916 = CARTESIAN_POINT ( 'NONE',  ( -35.50000000000000000, -115.0140978167138428, -0.6247823525986679893 ) ) ;
#6917 =( REPRESENTATION_RELATIONSHIP ('NONE','NONE', #26607, #2005 ) REPRESENTATION_RELATIONSHIP_WITH_TRANSFORMATION ( #4222 )SHAPE_REPRESENTATION_RELATIONSHIP( ) );
#6918 = CARTESIAN_POINT ( 'NONE',  ( 8.000000000000000000, 12.46108038583314936, 15.64357617739001860 ) ) ;
#6919 = CARTESIAN_POINT ( 'NONE',  ( 7.999999999999992895, 12.30077720129168384, -50.52416135122070528 ) ) ;
#6920 = AXIS2_PLACEMENT_3D ( 'NONE', #31117, #6801, #30937 ) ;
#6921 = ADVANCED_BREP_SHAPE_REPRESENTATION ( '', ( #10310, #21307 ), #32275 ) ;
#6922 = CARTESIAN_POINT ( 'NONE',  ( -35.50000000000000711, -114.9929510916434339, 12.50851088611648088 ) ) ;
#6923 = DIRECTION ( 'NONE',  ( 1.000000000000000000, 0.000000000000000000, 0.000000000000000000 ) ) ;
#6924 = VECTOR ( 'NONE', #35577, 1000.000000000000000 ) ;
#6925 = ADVANCED_FACE ( 'NONE', ( #9018 ), #33871, .T. ) ;
#6926 = CARTESIAN_POINT ( 'NONE',  ( -37.51022648969539119, -114.9929510916434339, 14.11852173794918386 ) ) ;
#6927 = DIRECTION ( 'NONE',  ( 0.000000000000000000, 0.9672551082808338307, -0.2538061376417690695 ) ) ;
#6928 = EDGE_CURVE ( 'NONE', #24111, #20033, #9197, .T. ) ;
#6929 = PRODUCT_DEFINITION_SHAPE ( 'NONE', 'NONE',  #35621 ) ;
#6930 = DIRECTION ( 'NONE',  ( 1.000000000000000000, 0.000000000000000000, 0.000000000000000000 ) ) ;
#6931 = ORIENTED_EDGE ( 'NONE', *, *, #22741, .F. ) ;
#6932 = CARTESIAN_POINT ( 'NONE',  ( -36.01562499999997158, -115.9929510916434481, 13.11852480586264846 ) ) ;
#6933 = CARTESIAN_POINT ( 'NONE',  ( -35.50000000000000711, -116.0012805033554883, -0.7876962586524312027 ) ) ;
#6934 = DIRECTION ( 'NONE',  ( 1.000000000000000000, -5.339440136655842133E-16, -1.047965281155519420E-16 ) ) ;
#6935 = DIRECTION ( 'NONE',  ( 0.000000000000000000, -1.000000000000000000, -1.040834085586082363E-14 ) ) ;
#6936 = FACE_OUTER_BOUND ( 'NONE', #21499, .T. ) ;
#6937 = CARTESIAN_POINT ( 'NONE',  ( -6.938893903907228378E-15, 0.7408941433508786645, -1.200000000000006617 ) ) ;
#6938 = DIRECTION ( 'NONE',  ( -1.000000000000000000, 0.000000000000000000, 0.000000000000000000 ) ) ;
#6939 = DIRECTION ( 'NONE',  ( -1.000000000000000000, 0.000000000000000000, 0.000000000000000000 ) ) ;
#6940 = DIRECTION ( 'NONE',  ( -1.000000000000000000, 0.000000000000000000, 0.000000000000000000 ) ) ;
#6941 = VERTEX_POINT ( 'NONE', #3637 ) ;
#6942 = CIRCLE ( 'NONE', #31662, 52.00000000000000711 ) ;
#6943 = CARTESIAN_POINT ( 'NONE',  ( -37.74901162816868805, -113.3347980657955958, 4.933975545821551734 ) ) ;
#6944 = DIRECTION ( 'NONE',  ( -1.000000000000000000, 0.000000000000000000, -0.000000000000000000 ) ) ;
#6945 = DIRECTION ( 'NONE',  ( -0.000000000000000000, 0.000000000000000000, -1.000000000000000000 ) ) ;
#6946 = ORIENTED_EDGE ( 'NONE', *, *, #34786, .F. ) ;
#6947 = ORIENTED_EDGE ( 'NONE', *, *, #18970, .F. ) ;
#6948 = LINE ( 'NONE', #9656, #13649 ) ;
#6949 = CARTESIAN_POINT ( 'NONE',  ( 0.000000000000000000, -11.11653975335798528, 12.74840161668727134 ) ) ;
#6950 = VERTEX_POINT ( 'NONE', #28117 ) ;
#6951 = CARTESIAN_POINT ( 'NONE',  ( -34.92058450342249643, -111.8367748094582197, 9.808975545821553510 ) ) ;
#6952 = VERTEX_POINT ( 'NONE', #6672 ) ;
#6953 = AXIS2_PLACEMENT_3D ( 'NONE', #12486, #31571, #29238 ) ;
#6954 =( GEOMETRIC_REPRESENTATION_CONTEXT ( 3 ) GLOBAL_UNCERTAINTY_ASSIGNED_CONTEXT ( ( #28323 ) ) GLOBAL_UNIT_ASSIGNED_CONTEXT ( ( #3166, #22227, #24947 ) ) REPRESENTATION_CONTEXT ( 'NONE', 'WORKASPACE' ) );
#6955 =( NAMED_UNIT ( * ) SI_UNIT ( $, .STERADIAN. ) SOLID_ANGLE_UNIT ( ) );
#6956 = AXIS2_PLACEMENT_3D ( 'NONE', #34926, #24458, #7367 ) ;
#6957 = CARTESIAN_POINT ( 'NONE',  ( 50.00000000000000711, 7.347880794884119736E-16, 76.00000000000001421 ) ) ;
#6958 = DIRECTION ( 'NONE',  ( 1.000000000000000000, -0.000000000000000000, -0.000000000000000000 ) ) ;
#6959 = LINE ( 'NONE', #28933, #7570 ) ;
#6960 = ORIENTED_EDGE ( 'NONE', *, *, #7245, .F. ) ;
#6961 = VERTEX_POINT ( 'NONE', #3461 ) ;
#6962 = CARTESIAN_POINT ( 'NONE',  ( 70.00001200000002655, -27.02775365097034310, 88.89589070667321380 ) ) ;
#6963 = FACE_OUTER_BOUND ( 'NONE', #10244, .T. ) ;
#6964 = ORIENTED_EDGE ( 'NONE', *, *, #4954, .F. ) ;
#6965 = CARTESIAN_POINT ( 'NONE',  ( 55.00000000000000000, 7.347880794884119736E-16, 76.00000000000001421 ) ) ;
#6966 = DIRECTION ( 'NONE',  ( 1.000000000000000000, -0.000000000000000000, 0.000000000000000000 ) ) ;
#6967 = CARTESIAN_POINT ( 'NONE',  ( 7.999999999999992895, 0.000000000000000000, 0.000000000000000000 ) ) ;
#6968 = EDGE_CURVE ( 'NONE', #3997, #31797, #8989, .T. ) ;
#6969 = CARTESIAN_POINT ( 'NONE',  ( -34.80050084267116972, -115.9929510916434481, 13.54034599209289347 ) ) ;
#6970 = DIRECTION ( 'NONE',  ( -1.000000000000000000, 0.000000000000000000, 0.000000000000000000 ) ) ;
#6971 = CARTESIAN_POINT ( 'NONE',  ( -35.02454729103298092, -114.8876895276775087, 1.597274454178448932 ) ) ;
#6972 = CIRCLE ( 'NONE', #3546, 47.49900000000003075 ) ;
#6973 = CARTESIAN_POINT ( 'NONE',  ( -34.50000000000000000, -115.9929510916434481, 12.59652202191340464 ) ) ;
#6975 = LINE ( 'NONE', #26248, #3848 ) ;
#6974 = AXIS2_PLACEMENT_3D ( 'NONE', #21555, #34927, #10253 ) ;
#6976 = FACE_OUTER_BOUND ( 'NONE', #14018, .T. ) ;
#6977 = DIRECTION ( 'NONE',  ( -1.000000000000000000, 5.339440136655842133E-16, 1.047965281155519420E-16 ) ) ;
#6978 = DIRECTION ( 'NONE',  ( 0.000000000000000000, 1.000000000000000000, 0.000000000000000000 ) ) ;
#6979 = CARTESIAN_POINT ( 'NONE',  ( 7.999999999999992895, 0.000000000000000000, 0.000000000000000000 ) ) ;
#6980 = CARTESIAN_POINT ( 'NONE',  ( 7.999999999999992895, 0.000000000000000000, 4.000000000000000000 ) ) ;
#6981 = EDGE_LOOP ( 'NONE', ( #33654, #10938, #19775, #35610 ) ) ;
#6982 = ADVANCED_FACE ( 'NONE', ( #14585 ), #28654, .T. ) ;
#6983 = CARTESIAN_POINT ( 'NONE',  ( -39.97545270896702618, -115.3019030900506152, 4.652725545821551734 ) ) ;
#6984 = LINE ( 'NONE', #4837, #16954 ) ;
#6985 = CARTESIAN_POINT ( 'NONE',  ( -35.50000000000000000, -113.1061333991432321, 0.8862035858144284850 ) ) ;
#6986 = ORIENTED_EDGE ( 'NONE', *, *, #10768, .F. ) ;
#6987 = EDGE_LOOP ( 'NONE', ( #30402, #3907, #15269, #25509 ) ) ;
#6988 = CARTESIAN_POINT ( 'NONE',  ( 0.2142857142857085284, -10.49781318335649161, -1.200000000000006617 ) ) ;
#6989 = ORIENTED_EDGE ( 'NONE', *, *, #34831, .F. ) ;
#6990 = ORIENTED_EDGE ( 'NONE', *, *, #27868, .T. ) ;
#6991 = ORIENTED_EDGE ( 'NONE', *, *, #12379, .T. ) ;
#6992 = DIRECTION ( 'NONE',  ( 0.000000000000000000, 0.000000000000000000, -1.000000000000000000 ) ) ;
#6993 = CARTESIAN_POINT ( 'NONE',  ( -37.05926240293131713, -112.0000000000000142, 8.121475545821549957 ) ) ;
#6994 = AXIS2_PLACEMENT_3D ( 'NONE', #13711, #8112, #5263 ) ;
#6995 = MECHANICAL_DESIGN_GEOMETRIC_PRESENTATION_REPRESENTATION (  '', ( #32297 ), #16755 ) ;
#6996 = AXIS2_PLACEMENT_3D ( 'NONE', #35067, #15403, #18833 ) ;
#6997 =( LENGTH_UNIT ( ) NAMED_UNIT ( * ) SI_UNIT ( .MILLI., .METRE. ) );
#6998 = CARTESIAN_POINT ( 'NONE',  ( 0.000000000000000000, 0.000000000000000000, 0.000000000000000000 ) ) ;
#6999 = VERTEX_POINT ( 'NONE', #25599 ) ;
#7000 = ORIENTED_EDGE ( 'NONE', *, *, #20746, .T. ) ;
#7001 = CARTESIAN_POINT ( 'NONE',  ( -35.50000000000000000, -117.0140814545088688, -0.6738694770610542673 ) ) ;
#7002 = CARTESIAN_POINT ( 'NONE',  ( 3.239593890920905217, -13.56862304811760822, 0.000000000000000000 ) ) ;
#7003 = LINE ( 'NONE', #14746, #27589 ) ;
#7004 = VERTEX_POINT ( 'NONE', #33682 ) ;
#7005 = CARTESIAN_POINT ( 'NONE',  ( -37.75185693410092824, -114.9929510916434339, 13.05539834812634581 ) ) ;
#7006 = TOROIDAL_SURFACE ( 'NONE', #13355, 7.800000000000023803, 0.1999999999999992339 ) ;
#7007 = ADVANCED_FACE ( 'NONE', ( #22689 ), #3283, .T. ) ;
#7008 = CARTESIAN_POINT ( 'NONE',  ( -34.50000000000000000, -114.8211182053456838, 9.932864235516914775 ) ) ;
#7009 = EDGE_CURVE ( 'NONE', #1934, #13123, #31166, .T. ) ;
#7010 = DIRECTION ( 'NONE',  ( -1.000000000000000000, 0.000000000000000000, 0.000000000000000000 ) ) ;
#7011 = CARTESIAN_POINT ( 'NONE',  ( -36.31249999999995026, -114.9929510916434339, 13.11852480586264669 ) ) ;
#7012 = DIRECTION ( 'NONE',  ( -1.000000000000000000, 0.000000000000000000, 0.000000000000000000 ) ) ;
#7013 = CARTESIAN_POINT ( 'NONE',  ( -36.31249999999994316, -113.9929510916434339, 14.11852480586265024 ) ) ;
#7014 = DIRECTION ( 'NONE',  ( -1.000000000000000000, -1.836970198721029934E-16, -0.000000000000000000 ) ) ;
#7015 = CARTESIAN_POINT ( 'NONE',  ( -37.93687354226506869, -114.9929510916434339, 12.87038173996323565 ) ) ;
#7016 = DIRECTION ( 'NONE',  ( -0.000000000000000000, 0.2538061376417689585, 0.9672551082808338307 ) ) ;
#7017 = ORIENTED_EDGE ( 'NONE', *, *, #4914, .T. ) ;
#7018 = CARTESIAN_POINT ( 'NONE',  ( -34.49999999999998579, -28.81745899286270074, 95.58669687932930970 ) ) ;
#7019 = CARTESIAN_POINT ( 'NONE',  ( 7.999999999999992895, 42.60732521687599217, -19.80331771201615609 ) ) ;
#7020 = ORIENTED_EDGE ( 'NONE', *, *, #17193, .F. ) ;
#7021 = CARTESIAN_POINT ( 'NONE',  ( -35.50000000000000711, -114.9929510916434339, 12.57451923796416082 ) ) ;
#7022 = ORIENTED_EDGE ( 'NONE', *, *, #21144, .F. ) ;
#7023 = ADVANCED_FACE ( 'NONE', ( #25421 ), #920, .T. ) ;
#7024 = VECTOR ( 'NONE', #26418, 1000.000000000000000 ) ;
#7025 = AXIS2_PLACEMENT_3D ( 'NONE', #8370, #24606, #5692 ) ;
#7026 = CARTESIAN_POINT ( 'NONE',  ( -34.49999999999998579, -25.98076211353322051, 84.99999999999992895 ) ) ;
#7027 = EDGE_LOOP ( 'NONE', ( #15396, #22436, #15486, #19299 ) ) ;
#7028 = CARTESIAN_POINT ( 'NONE',  ( -36.49999999999999289, -11.52052244843579309, 115.1848168619253698 ) ) ;
#7029 = EDGE_LOOP ( 'NONE', ( #22265, #30490, #5233, #33520 ) ) ;
#7030 = CARTESIAN_POINT ( 'NONE',  ( -34.50000000000000000, -113.0140978167138712, 0.8752176474015154195 ) ) ;
#7031 = CARTESIAN_POINT ( 'NONE',  ( 4.000000000000003553, -51.93417535146743802, 2.615612846549014492 ) ) ;
#7032 = CARTESIAN_POINT ( 'NONE',  ( -39.02454729103295961, -114.7691647218148745, 8.159774454178448266 ) ) ;
#7033 = ORIENTED_EDGE ( 'NONE', *, *, #12221, .F. ) ;
#7034 = CARTESIAN_POINT ( 'NONE',  ( -39.02454729103295961, -114.7691647218148745, 5.159774454178448266 ) ) ;
#7035 = CIRCLE ( 'NONE', #31761, 20.00000000000000355 ) ;
#7036 = DIRECTION ( 'NONE',  ( -1.000000000000000000, 0.000000000000000000, 0.000000000000000000 ) ) ;
#7037 = CARTESIAN_POINT ( 'NONE',  ( -35.50000000000000711, -115.9821387493194891, -0.8839717462762166633 ) ) ;
#7038 = ORIENTED_EDGE ( 'NONE', *, *, #16599, .F. ) ;
#7039 = EDGE_LOOP ( 'NONE', ( #1927, #21556, #20255, #30611 ) ) ;
#7040 = LINE ( 'NONE', #23437, #10203 ) ;
#7041 = EDGE_CURVE ( 'NONE', #10764, #11716, #24537, .T. ) ;
#7042 = CARTESIAN_POINT ( 'NONE',  ( 7.999999999999992895, 19.44205635905603202, -43.33776004284589334 ) ) ;
#7043 = ORIENTED_EDGE ( 'NONE', *, *, #8952, .F. ) ;
#7044 = EDGE_LOOP ( 'NONE', ( #32899, #16237, #5879, #692 ) ) ;
#7045 = CARTESIAN_POINT ( 'NONE',  ( -34.50000000000000000, -113.0974311500471714, -1.624782352598427959 ) ) ;
#7046 = CARTESIAN_POINT ( 'NONE',  ( -35.50000000000000711, -112.9185811467682754, 1.870920967077121411 ) ) ;
#7047 = AXIS2_PLACEMENT_3D ( 'NONE', #25978, #15146, #7056 ) ;
#7048 = DIRECTION ( 'NONE',  ( 1.084202172485497408E-16, -6.938893903907204958E-17, -1.000000000000000000 ) ) ;
#7049 = ORIENTED_EDGE ( 'NONE', *, *, #3009, .F. ) ;
#7050 = AXIS2_PLACEMENT_3D ( 'NONE', #20137, #33013, #24560 ) ;
#7051 = ORIENTED_EDGE ( 'NONE', *, *, #2860, .T. ) ;
#7052 = LINE ( 'NONE', #9586, #9726 ) ;
#7053 = ADVANCED_FACE ( 'NONE', ( #14771 ), #1276, .T. ) ;
#7054 = CARTESIAN_POINT ( 'NONE',  ( -34.50000000000000000, -113.9929510916434339, 10.50625754673586876 ) ) ;
#7055 = EDGE_CURVE ( 'NONE', #3424, #7407, #1108, .T. ) ;
#7056 = DIRECTION ( 'NONE',  ( 0.000000000000000000, 0.000000000000000000, 1.000000000000000000 ) ) ;
#7057 = EDGE_CURVE ( 'NONE', #21218, #27996, #9376, .T. ) ;
#7058 = CARTESIAN_POINT ( 'NONE',  ( -35.50000000000000000, -113.9929510916434339, 12.53051367006571581 ) ) ;
#7059 = CARTESIAN_POINT ( 'NONE',  ( -35.50000000000000000, -115.1342778146718473, 8.846135899190283425 ) ) ;
#7060 = FACE_OUTER_BOUND ( 'NONE', #22430, .T. ) ;
#7061 = VECTOR ( 'NONE', #35344, 1000.000000000000000 ) ;
#7062 = DIRECTION ( 'NONE',  ( 1.000000000000000000, -4.524158825347490025E-15, -1.169797080839617330E-15 ) ) ;
#7063 = VECTOR ( 'NONE', #16180, 1000.000000000000114 ) ;
#7064 = VERTEX_POINT ( 'NONE', #6146 ) ;
#7065 = ADVANCED_FACE ( 'NONE', ( #24276 ), #18186, .T. ) ;
#7066 = DIRECTION ( 'NONE',  ( 0.000000000000000000, 0.000000000000000000, -1.000000000000000000 ) ) ;
#7067 = CARTESIAN_POINT ( 'NONE',  ( 8.000000000000007105, 0.000000000000000000, 0.000000000000000000 ) ) ;
#7068 = LINE ( 'NONE', #9774, #17415 ) ;
#7069 = ADVANCED_FACE ( 'NONE', ( #35431 ), #21535, .F. ) ;
#7070 = ORIENTED_EDGE ( 'NONE', *, *, #435, .F. ) ;
#7071 = LINE ( 'NONE', #2051, #27396 ) ;
#7072 = CIRCLE ( 'NONE', #6479, 4.800000000000002487 ) ;
#7073 = CARTESIAN_POINT ( 'NONE',  ( -35.50000000000000711, -112.2144317118258527, -1.239329810084414341 ) ) ;
#7074 = DIRECTION ( 'NONE',  ( -1.000000000000000000, 0.000000000000000000, 0.000000000000000000 ) ) ;
#7075 = CIRCLE ( 'NONE', #31236, 6.765000000000044977 ) ;
#7076 = DIRECTION ( 'NONE',  ( 0.000000000000000000, 0.9048270524660205760, -0.4257792915650702170 ) ) ;
#7077 = DIRECTION ( 'NONE',  ( 0.000000000000000000, 1.000000000000000000, 0.000000000000000000 ) ) ;
#7078 = VERTEX_POINT ( 'NONE', #19032 ) ;
#7079 = DIRECTION ( 'NONE',  ( -1.000000000000000000, 0.000000000000000000, 0.000000000000000000 ) ) ;
#7080 = CARTESIAN_POINT ( 'NONE',  ( -35.50000000000000000, -113.6974040292745656, 2.970979214817929481 ) ) ;
#7081 = CARTESIAN_POINT ( 'NONE',  ( 8.000000000000000000, -2.494040418455483188, 18.62763138773849292 ) ) ;
#7082 = ORIENTED_EDGE ( 'NONE', *, *, #32457, .T. ) ;
#7083 = ORIENTED_EDGE ( 'NONE', *, *, #2944, .T. ) ;
#7084 = CARTESIAN_POINT ( 'NONE',  ( -38.02454729103296671, -114.3549511594417396, 5.159774454178449155 ) ) ;
#7085 = EDGE_CURVE ( 'NONE', #7361, #13238, #14160, .T. ) ;
#7087 = ORIENTED_EDGE ( 'NONE', *, *, #22857, .F. ) ;
#7086 = AXIS2_PLACEMENT_3D ( 'NONE', #31849, #12598, #9881 ) ;
#7088 = ORIENTED_EDGE ( 'NONE', *, *, #13862, .F. ) ;
#7089 = CARTESIAN_POINT ( 'NONE',  ( -35.50000000000000000, -113.6807644833805995, -0.6247823525984269599 ) ) ;
#7090 = EDGE_CURVE ( 'NONE', #24162, #17966, #7204, .T. ) ;
#7091 = EDGE_CURVE ( 'NONE', #32201, #21788, #2704, .T. ) ;
#7092 = CARTESIAN_POINT ( 'NONE',  ( 7.999999999999992895, 36.05989434073613609, 30.12041790338630776 ) ) ;
#7093 = CARTESIAN_POINT ( 'NONE',  ( 7.999999999999992895, -38.92705108641750655, 27.21837053747785973 ) ) ;
#7094 = AXIS2_PLACEMENT_3D ( 'NONE', #13729, #24008, #32808 ) ;
#7095 = CARTESIAN_POINT ( 'NONE',  ( -36.99999999999989342, -114.9929510916434339, 13.11852480586264669 ) ) ;
#7096 = CIRCLE ( 'NONE', #2526, 47.49900000000000944 ) ;
#7097 = CARTESIAN_POINT ( 'NONE',  ( 55.00000000000000000, 0.000000000000000000, 0.000000000000000000 ) ) ;
#7098 = EDGE_CURVE ( 'NONE', #33174, #21242, #27422, .T. ) ;
#7099 = AXIS2_PLACEMENT_3D ( 'NONE', #791, #30867, #20579 ) ;
#7100 = EDGE_CURVE ( 'NONE', #27258, #29830, #3259, .T. ) ;
#7101 = CARTESIAN_POINT ( 'NONE',  ( -34.68937937320795584, -114.9929510916434339, 13.37409560816408671 ) ) ;
#7102 = CARTESIAN_POINT ( 'NONE',  ( 63.00000000000001421, -26.94801722181409431, 85.25380613764163229 ) ) ;
#7103 = CARTESIAN_POINT ( 'NONE',  ( -39.49999999999999289, -1.387778780781445676E-14, 106.0000000000000000 ) ) ;
#7104 = ORIENTED_EDGE ( 'NONE', *, *, #33042, .T. ) ;
#7105 = CARTESIAN_POINT ( 'NONE',  ( -35.96730626674924025, -115.9929510916434481, 13.11752178341330222 ) ) ;
#7106 = CARTESIAN_POINT ( 'NONE',  ( -35.50000000000000711, -113.2224311500466030, -1.624782352598427959 ) ) ;
#7107 = LINE ( 'NONE', #29269, #7857 ) ;
#7108 = DIRECTION ( 'NONE',  ( -1.000000000000000000, 0.000000000000000000, 0.000000000000000000 ) ) ;
#7109 = EDGE_CURVE ( 'NONE', #23379, #28580, #5198, .T. ) ;
#7110 = CIRCLE ( 'NONE', #9400, 8.000000000000010658 ) ;
#7111 = ORIENTED_EDGE ( 'NONE', *, *, #17035, .F. ) ;
#7112 = AXIS2_PLACEMENT_3D ( 'NONE', #27097, #21311, #15907 ) ;
#7113 = DIRECTION ( 'NONE',  ( -1.000000000000000000, 0.000000000000000000, 0.000000000000000000 ) ) ;
#7114 = PLANE ( 'NONE',  #33118 ) ;
#7115 = CARTESIAN_POINT ( 'NONE',  ( 8.000000000000000000, -1.693188892523842082, 15.40623615209871566 ) ) ;
#7116 = CARTESIAN_POINT ( 'NONE',  ( 2.600000000000004974, -12.74999999999999822, -1.200000000000006617 ) ) ;
#7117 = VERTEX_POINT ( 'NONE', #20695 ) ;
#7118 = CARTESIAN_POINT ( 'NONE',  ( -35.97545270896702618, -113.6450488405582604, 5.909774454178450931 ) ) ;
#7119 = CARTESIAN_POINT ( 'NONE',  ( 7.999999999999992895, -17.50309955389642269, 43.60271849949356948 ) ) ;
#7120 = DIRECTION ( 'NONE',  ( -9.178431089824344374E-17, 6.938893903907203726E-17, 1.000000000000000000 ) ) ;
#7121 = ORIENTED_EDGE ( 'NONE', *, *, #32873, .T. ) ;
#7122 = ORIENTED_EDGE ( 'NONE', *, *, #34922, .T. ) ;
#7123 = APPLICATION_CONTEXT ( 'automotive_design' ) ;
#7124 = AXIS2_PLACEMENT_3D ( 'NONE', #5592, #11511, #30772 ) ;
#7125 = DIRECTION ( 'NONE',  ( 0.000000000000000000, -1.000000000000000000, 0.000000000000000000 ) ) ;
#7126 = VECTOR ( 'NONE', #18441, 1000.000000000000000 ) ;
#7127 = CARTESIAN_POINT ( 'NONE',  ( 7.999999999999992895, -51.93417535146744513, 2.615612846549014492 ) ) ;
#7128 = ORIENTED_EDGE ( 'NONE', *, *, #5712, .T. ) ;
#7129 = CARTESIAN_POINT ( 'NONE',  ( -35.69809690994941320, -116.9754527089670546, 7.277725545821552622 ) ) ;
#7130 = ORIENTED_EDGE ( 'NONE', *, *, #21777, .T. ) ;
#7131 = ADVANCED_FACE ( 'NONE', ( #1457 ), #16316, .T. ) ;
#7132 = CARTESIAN_POINT ( 'NONE',  ( 8.000000000000000000, 0.000000000000000000, 0.000000000000000000 ) ) ;
#7133 = ORIENTED_EDGE ( 'NONE', *, *, #28721, .T. ) ;
#7134 = DIRECTION ( 'NONE',  ( -1.000000000000000000, 0.000000000000000000, 0.000000000000000000 ) ) ;
#7135 = EDGE_CURVE ( 'NONE', #27859, #28824, #2673, .T. ) ;
#7136 = CARTESIAN_POINT ( 'NONE',  ( 7.999999999999992895, -32.00046193115124282, -34.40241257139719977 ) ) ;
#7137 = CARTESIAN_POINT ( 'NONE',  ( 0.000000000000000000, 29.60891106212789126, 37.14118181634776050 ) ) ;
#7138 = ORIENTED_EDGE ( 'NONE', *, *, #9094, .T. ) ;
#7139 = EDGE_LOOP ( 'NONE', ( #28135, #14330 ) ) ;
#7140 = CARTESIAN_POINT ( 'NONE',  ( 46.00000000000000000, 1.347111479062090180E-15, 81.00000000000001421 ) ) ;
#7141 = CARTESIAN_POINT ( 'NONE',  ( 7.999999999999992895, -11.90021268425521939, -45.45261810511225065 ) ) ;
#7142 = EDGE_CURVE ( 'NONE', #26801, #24996, #1826, .T. ) ;
#7143 = ORIENTED_EDGE ( 'NONE', *, *, #9438, .T. ) ;
#7144 = CARTESIAN_POINT ( 'NONE',  ( 38.00000000000000000, 6.980486755139912911E-15, 0.000000000000000000 ) ) ;
#7145 = CARTESIAN_POINT ( 'NONE',  ( -1.599999999999990763, 9.554310223899640008E-16, 4.980000000000017302 ) ) ;
#7146 = DIRECTION ( 'NONE',  ( 0.000000000000000000, 0.000000000000000000, -1.000000000000000000 ) ) ;
#7147 = AXIS2_PLACEMENT_3D ( 'NONE', #28964, #9867, #20476 ) ;
#7148 = CARTESIAN_POINT ( 'NONE',  ( -36.50000000000010658, -115.9929510916434481, 14.11852480586265024 ) ) ;
#7149 = CIRCLE ( 'NONE', #15746, 4.000000000000000000 ) ;
#7150 = DIRECTION ( 'NONE',  ( -1.000000000000000000, 0.000000000000000000, 0.000000000000000000 ) ) ;
#7151 = CARTESIAN_POINT ( 'NONE',  ( -36.11231047232249836, -112.0245472910329880, 7.222274454178450043 ) ) ;
#7152 = CARTESIAN_POINT ( 'NONE',  ( -34.50000000000000000, -115.9929510916434481, 10.72628538622835670 ) ) ;
#7153 = CARTESIAN_POINT ( 'NONE',  ( 0.000000000000000000, 0.000000000000000000, -1.200000000000006617 ) ) ;
#7154 = CIRCLE ( 'NONE', #28440, 4.000000000000000000 ) ;
#7155 = CARTESIAN_POINT ( 'NONE',  ( 2.141980652367342586, -6.189445006155629869, -0.7999999999999951594 ) ) ;
#7156 = CARTESIAN_POINT ( 'NONE',  ( -3.799999999999999822, 4.653657836759942730E-16, -32.00000000000000000 ) ) ;
#7157 = CARTESIAN_POINT ( 'NONE',  ( 8.000000000000000000, 3.968388925835109049, -21.63912866391136447 ) ) ;
#7158 = LINE ( 'NONE', #23728, #363 ) ;
#7159 =( NAMED_UNIT ( * ) SI_UNIT ( $, .STERADIAN. ) SOLID_ANGLE_UNIT ( ) );
#7160 = VERTEX_POINT ( 'NONE', #12624 ) ;
#7161 = CARTESIAN_POINT ( 'NONE',  ( -34.92058450342249643, -111.8367748094582197, 5.308975545821551734 ) ) ;
#7162 = DIRECTION ( 'NONE',  ( 1.000000000000000000, -0.000000000000000000, -0.000000000000000000 ) ) ;
#7163 = CARTESIAN_POINT ( 'NONE',  ( -35.50000000000000000, -113.1981689815712997, 0.8971895242272823756 ) ) ;
#7164 = VERTEX_POINT ( 'NONE', #24627 ) ;
#7165 = ORIENTED_EDGE ( 'NONE', *, *, #15653, .F. ) ;
#7166 =( LENGTH_UNIT ( ) NAMED_UNIT ( * ) SI_UNIT ( .MILLI., .METRE. ) );
#7167 = CARTESIAN_POINT ( 'NONE',  ( 8.000000000000000000, 9.471478019455140895, 14.71414642875960332 ) ) ;
#7168 = ORIENTED_EDGE ( 'NONE', *, *, #6239, .T. ) ;
#7169 = EDGE_LOOP ( 'NONE', ( #12979, #6872 ) ) ;
#7170 = ORIENTED_EDGE ( 'NONE', *, *, #28176, .T. ) ;
#7171 = AXIS2_PLACEMENT_3D ( 'NONE', #5718, #17205, #16856 ) ;
#7172 = EDGE_CURVE ( 'NONE', #11290, #11685, #13465, .T. ) ;
#7173 = DIRECTION ( 'NONE',  ( -1.000000000000000000, 0.000000000000000000, 0.000000000000000000 ) ) ;
#7174 = CIRCLE ( 'NONE', #19246, 6.765000000000044977 ) ;
#7175 = CARTESIAN_POINT ( 'NONE',  ( 7.999999999999992895, 0.6505223195690454929, -51.99593080916758936 ) ) ;
#7176 = CARTESIAN_POINT ( 'NONE',  ( -49.09999999999999432, -1.219727444046192488E-14, 110.0000000000000000 ) ) ;
#7177 = DIRECTION ( 'NONE',  ( 0.000000000000000000, 0.000000000000000000, 1.000000000000000000 ) ) ;
#7178 = ORIENTED_EDGE ( 'NONE', *, *, #7952, .T. ) ;
#7179 = ORIENTED_EDGE ( 'NONE', *, *, #7522, .F. ) ;
#7180 = CARTESIAN_POINT ( 'NONE',  ( -35.50000000000000711, -112.9813730236132585, -1.624774171495860786 ) ) ;
#7181 = CARTESIAN_POINT ( 'NONE',  ( 0.000000000000000000, -51.85248208264521708, 3.914090171286008335 ) ) ;
#7182 = DIRECTION ( 'NONE',  ( -1.000000000000000000, 0.000000000000000000, -0.000000000000000000 ) ) ;
#7183 = VERTEX_POINT ( 'NONE', #35613 ) ;
#7184 = CARTESIAN_POINT ( 'NONE',  ( -37.99839555572501837, -114.9929510916434339, 12.65937477241748965 ) ) ;
#7185 = AXIS2_PLACEMENT_3D ( 'NONE', #18038, #6354, #26156 ) ;
#7186 = LINE ( 'NONE', #6522, #3514 ) ;
#7187 = CARTESIAN_POINT ( 'NONE',  ( -34.50000000000000000, -114.9902084924877954, 10.43071793783961176 ) ) ;
#7188 = DIRECTION ( 'NONE',  ( -1.000000000000000000, 0.000000000000000000, 0.000000000000000000 ) ) ;
#7189 = CARTESIAN_POINT ( 'NONE',  ( -35.96730626674924025, -114.9929510916434339, 13.11752178341330044 ) ) ;
#7190 = DIRECTION ( 'NONE',  ( -1.000000000000000000, 0.000000000000000000, 0.000000000000000000 ) ) ;
#7191 = CARTESIAN_POINT ( 'NONE',  ( -34.50000000000000000, -114.9929501463477663, 10.50247632894551231 ) ) ;
#7192 = CARTESIAN_POINT ( 'NONE',  ( -9.999999999999994671, 0.000000000000000000, 0.000000000000000000 ) ) ;
#7193 = CARTESIAN_POINT ( 'NONE',  ( -37.66108410722335265, -114.9929510916434339, 13.09299768411426790 ) ) ;
#7194 = ORIENTED_EDGE ( 'NONE', *, *, #33012, .T. ) ;
#7195 = CARTESIAN_POINT ( 'NONE',  ( 7.999999999999992895, 46.11014828289831513, 9.022736828081523441 ) ) ;
#7196 = DIRECTION ( 'NONE',  ( 0.000000000000000000, 0.000000000000000000, 1.000000000000000000 ) ) ;
#7197 = ORIENTED_EDGE ( 'NONE', *, *, #1207, .T. ) ;
#7198 = CARTESIAN_POINT ( 'NONE',  ( -36.99999999999989342, -114.9929510916434339, 13.11852480586264669 ) ) ;
#7199 = VERTEX_POINT ( 'NONE', #34419 ) ;
#7200 = CARTESIAN_POINT ( 'NONE',  ( -37.76916472181487450, -111.9754527089670404, 2.534774454178448710 ) ) ;
#7201 = LINE ( 'NONE', #13168, #33051 ) ;
#7202 = AXIS2_PLACEMENT_3D ( 'NONE', #15924, #24063, #23322 ) ;
#7203 = ORIENTED_EDGE ( 'NONE', *, *, #32332, .F. ) ;
#7204 = LINE ( 'NONE', #32533, #21066 ) ;
#7205 = VERTEX_POINT ( 'NONE', #21910 ) ;
#7206 = CIRCLE ( 'NONE', #2634, 19.99999999999999289 ) ;
#7207 = CARTESIAN_POINT ( 'NONE',  ( -34.50000000000000000, -113.0140978167136581, 0.8752176474015690433 ) ) ;
#7208 = CARTESIAN_POINT ( 'NONE',  ( 8.000000000000007105, 0.000000000000000000, 9.499000000000000554 ) ) ;
#7209 = CARTESIAN_POINT ( 'NONE',  ( -38.45611840935523418, -115.3723087153909432, 6.566024454178448266 ) ) ;
#7210 = EDGE_LOOP ( 'NONE', ( #13587, #2343, #21836, #15938 ) ) ;
#7211 = CARTESIAN_POINT ( 'NONE',  ( -34.83677480945819838, -111.9205845034225462, 5.816024454178450043 ) ) ;
#7212 = CIRCLE ( 'NONE', #14095, 20.00000000000000711 ) ;
#7213 = CARTESIAN_POINT ( 'NONE',  ( 0.000000000000000000, 0.000000000000000000, 0.000000000000000000 ) ) ;
#7214 = EDGE_CURVE ( 'NONE', #25525, #3192, #10942, .T. ) ;
#7215 = CARTESIAN_POINT ( 'NONE',  ( -35.50000000000000711, -112.0157046079661995, -0.6902086197697556713 ) ) ;
#7216 = EDGE_LOOP ( 'NONE', ( #2726, #13340, #28095, #8363 ) ) ;
#7217 = ORIENTED_EDGE ( 'NONE', *, *, #2084, .F. ) ;
#7218 = EDGE_CURVE ( 'NONE', #27160, #9066, #6122, .T. ) ;
#7219 = CARTESIAN_POINT ( 'NONE',  ( 3.872983346207416133, 1.000000000000001110, 30.00000000000000000 ) ) ;
#7220 = SURFACE_STYLE_FILL_AREA ( #12453 ) ;
#7221 = LINE ( 'NONE', #7042, #4671 ) ;
#7222 = ORIENTED_EDGE ( 'NONE', *, *, #17374, .F. ) ;
#7223 = ORIENTED_EDGE ( 'NONE', *, *, #24381, .F. ) ;
#7224 = CARTESIAN_POINT ( 'NONE',  ( -34.50000000000000000, -113.3474311500483935, -1.624782352598427959 ) ) ;
#7225 = PRODUCT_DEFINITION_SHAPE ( 'NONE', 'NONE',  #33925 ) ;
#7226 = AXIS2_PLACEMENT_3D ( 'NONE', #10899, #30341, #29985 ) ;
#7227 = EDGE_CURVE ( 'NONE', #7877, #20597, #4175, .T. ) ;
#7228 = DIRECTION ( 'NONE',  ( -1.000000000000000000, 0.000000000000000000, 0.000000000000000000 ) ) ;
#7229 = ORIENTED_EDGE ( 'NONE', *, *, #15016, .F. ) ;
#7230 = ORIENTED_EDGE ( 'NONE', *, *, #24239, .F. ) ;
#7231 = CARTESIAN_POINT ( 'NONE',  ( 0.000000000000000000, -2.710505431213761085E-17, 38.00000000000000711 ) ) ;
#7232 = AXIS2_PLACEMENT_3D ( 'NONE', #20366, #4573, #20905 ) ;
#7233 = AXIS2_PLACEMENT_3D ( 'NONE', #33381, #27987, #20376 ) ;
#7234 = CARTESIAN_POINT ( 'NONE',  ( -34.50000000000000000, -113.9836614335179377, 10.50514867547815534 ) ) ;
#7235 = DIRECTION ( 'NONE',  ( 0.000000000000000000, -0.6427876096865456912, 0.7660444431189726844 ) ) ;
#7236 = CARTESIAN_POINT ( 'NONE',  ( -38.00000000000000711, -113.9929510916434339, 11.91443571948719615 ) ) ;
#7237 = CARTESIAN_POINT ( 'NONE',  ( -38.00000000000000711, -115.9929510916434481, 12.44250253426875119 ) ) ;
#7238 = CIRCLE ( 'NONE', #23326, 4.000000000000000000 ) ;
#7239 = CARTESIAN_POINT ( 'NONE',  ( 0.000000000000000000, 3.968388925834817282, 21.63912866391139289 ) ) ;
#7240 = DIRECTION ( 'NONE',  ( -1.783119874454246424E-31, -1.187911941725854497E-31, 1.000000000000000000 ) ) ;
#7241 = ORIENTED_EDGE ( 'NONE', *, *, #3374, .F. ) ;
#7242 = FACE_OUTER_BOUND ( 'NONE', #4147, .T. ) ;
#7243 = CARTESIAN_POINT ( 'NONE',  ( -21.15833593587365513, -18.77980021920990694, 100.4724318643354053 ) ) ;
#7244 = CARTESIAN_POINT ( 'NONE',  ( 0.000000000000000000, -40.47821179127691238, -32.64221760512803172 ) ) ;
#7245 = EDGE_CURVE ( 'NONE', #19089, #23662, #17027, .T. ) ;
#7246 = ORIENTED_EDGE ( 'NONE', *, *, #19133, .F. ) ;
#7247 = FACE_OUTER_BOUND ( 'NONE', #14787, .T. ) ;
#7248 = VECTOR ( 'NONE', #10131, 1000.000000000000000 ) ;
#7249 = CARTESIAN_POINT ( 'NONE',  ( -35.50000000000000711, -112.8835768857893527, -1.616767172155725740 ) ) ;
#7250 = DIRECTION ( 'NONE',  ( 1.000000000000000000, 0.000000000000000000, 0.000000000000000000 ) ) ;
#7251 = CARTESIAN_POINT ( 'NONE',  ( 8.000000000000000000, 17.47118961583601759, 0.9861715913088272556 ) ) ;
#7252 = LINE ( 'NONE', #12852, #18227 ) ;
#7253 = AXIS2_PLACEMENT_3D ( 'NONE', #26527, #29227, #4382 ) ;
#7254 = AXIS2_PLACEMENT_3D ( 'NONE', #31823, #10408, #2320 ) ;
#7255 = EDGE_LOOP ( 'NONE', ( #23658, #22124, #33272, #23675 ) ) ;
#7256 = AXIS2_PLACEMENT_3D ( 'NONE', #25644, #9250, #31573 ) ;
#7257 = LINE ( 'NONE', #17516, #7826 ) ;
#7258 = ADVANCED_FACE ( 'NONE', ( #4349 ), #15297, .T. ) ;
#7259 = CARTESIAN_POINT ( 'NONE',  ( -34.50000000000000000, -116.2431927316855109, -2.224114562372550008 ) ) ;
#7260 = CARTESIAN_POINT ( 'NONE',  ( 4.000000000000000000, -12.46108038583301791, -15.64357617739007722 ) ) ;
#7261 = VERTEX_POINT ( 'NONE', #649 ) ;
#7262 = ORIENTED_EDGE ( 'NONE', *, *, #34832, .T. ) ;
#7263 = EDGE_CURVE ( 'NONE', #453, #28247, #8224, .T. ) ;
#7264 = CARTESIAN_POINT ( 'NONE',  ( -37.74901162816869515, -114.6652019342044042, 2.066024454178448710 ) ) ;
#7265 = ADVANCED_FACE ( 'NONE', ( #8399 ), #16672, .F. ) ;
#7266 = AXIS2_PLACEMENT_3D ( 'NONE', #8889, #17161, #22567 ) ;
#7267 = AXIS2_PLACEMENT_3D ( 'NONE', #8389, #2318, #21721 ) ;
#7268 = DIRECTION ( 'NONE',  ( 1.000000000000000000, -0.000000000000000000, -0.000000000000000000 ) ) ;
#7269 = ORIENTED_EDGE ( 'NONE', *, *, #30037, .T. ) ;
#7270 = VERTEX_POINT ( 'NONE', #30551 ) ;
#7271 = CARTESIAN_POINT ( 'NONE',  ( -34.50000000000000000, -113.0601156079281253, 0.8807106166081309917 ) ) ;
#7272 = ADVANCED_FACE ( 'NONE', ( #11288 ), #5882, .T. ) ;
#7273 = DIRECTION ( 'NONE',  ( 0.000000000000000000, 0.000000000000000000, 1.000000000000000000 ) ) ;
#7274 = EDGE_CURVE ( 'NONE', #223, #19677, #33257, .T. ) ;
#7275 = DIRECTION ( 'NONE',  ( -1.000000000000000000, 0.000000000000000000, 0.000000000000000000 ) ) ;
#7276 = AXIS2_PLACEMENT_3D ( 'NONE', #10076, #21231, #2357 ) ;
#7277 = CIRCLE ( 'NONE', #23973, 20.00000000000000355 ) ;
#7278 = CARTESIAN_POINT ( 'NONE',  ( -35.50000000000000000, -113.9813390189866027, 10.50487145766371100 ) ) ;
#7279 = CARTESIAN_POINT ( 'NONE',  ( 7.999999999999992895, -36.34385289850568057, -29.77717097092114074 ) ) ;
#7280 = AXIS2_PLACEMENT_3D ( 'NONE', #28373, #22780, #20067 ) ;
#7281 = CARTESIAN_POINT ( 'NONE',  ( -35.95093014754292682, -114.9929510916434339, 14.11777216781842448 ) ) ;
#7282 = DIRECTION ( 'NONE',  ( 0.000000000000000000, 0.2538061376417690140, 0.9672551082808337197 ) ) ;
#7283 = AXIS2_PLACEMENT_3D ( 'NONE', #22564, #258, #5678 ) ;
#7284 = VECTOR ( 'NONE', #12162, 1000.000000000000000 ) ;
#7285 = DIRECTION ( 'NONE',  ( 0.000000000000000000, 0.000000000000000000, -1.000000000000000000 ) ) ;
#7286 = ORIENTED_EDGE ( 'NONE', *, *, #27833, .T. ) ;
#7287 = CARTESIAN_POINT ( 'NONE',  ( -36.03125000000003553, -115.9929510916434481, 13.11852480586264846 ) ) ;
#7288 = DIRECTION ( 'NONE',  ( -1.000000000000000000, 0.000000000000000000, 0.000000000000000000 ) ) ;
#7289 = AXIS2_PLACEMENT_3D ( 'NONE', #19639, #19808, #30481 ) ;
#7290 = CARTESIAN_POINT ( 'NONE',  ( -55.00000000000000000, -2.775557561562891351E-14, 106.0000000000000000 ) ) ;
#7291 = EDGE_CURVE ( 'NONE', #32647, #8637, #22428, .T. ) ;
#7292 = LINE ( 'NONE', #10360, #24571 ) ;
#7293 = VECTOR ( 'NONE', #16630, 1000.000000000000000 ) ;
#7294 = ORIENTED_EDGE ( 'NONE', *, *, #18679, .T. ) ;
#7295 = CARTESIAN_POINT ( 'NONE',  ( 8.000000000000000000, -8.128228055638974325, 16.94522934049209795 ) ) ;
#7296 = LINE ( 'NONE', #18451, #30240 ) ;
#7297 = LINE ( 'NONE', #9817, #18202 ) ;
#7298 = DIRECTION ( 'NONE',  ( -1.000000000000000000, 1.110223024625156540E-16, 0.000000000000000000 ) ) ;
#7299 = ORIENTED_EDGE ( 'NONE', *, *, #35455, .F. ) ;
#7300 = CARTESIAN_POINT ( 'NONE',  ( -36.94073759706866156, -113.0000000000000000, 2.628524454178448710 ) ) ;
#7301 = CARTESIAN_POINT ( 'NONE',  ( 8.000000000000000000, 0.000000000000000000, 0.000000000000000000 ) ) ;
#7302 = CYLINDRICAL_SURFACE ( 'NONE', #15853, 47.49900000000001654 ) ;
#7303 = ORIENTED_EDGE ( 'NONE', *, *, #35204, .T. ) ;
#7304 = CIRCLE ( 'NONE', #21088, 17.49900000000002720 ) ;
#7305 = ORIENTED_EDGE ( 'NONE', *, *, #31327, .T. ) ;
#7306 = SURFACE_STYLE_FILL_AREA ( #6772 ) ;
#7307 = AXIS2_PLACEMENT_3D ( 'NONE', #68, #18971, #32473 ) ;
#7308 = LINE ( 'NONE', #1923, #30186 ) ;
#7309 = ORIENTED_EDGE ( 'NONE', *, *, #30598, .F. ) ;
#7310 = EDGE_CURVE ( 'NONE', #428, #2565, #16848, .T. ) ;
#7311 = CARTESIAN_POINT ( 'NONE',  ( -39.02454729103295961, -113.2308352781851539, 3.340225545821550845 ) ) ;
#7312 = EDGE_CURVE ( 'NONE', #6849, #21828, #22232, .T. ) ;
#7313 = ORIENTED_EDGE ( 'NONE', *, *, #11127, .T. ) ;
#7314 = AXIS2_PLACEMENT_3D ( 'NONE', #20806, #9675, #28939 ) ;
#7315 = AXIS2_PLACEMENT_3D ( 'NONE', #30081, #16370, #10992 ) ;
#7316 = CYLINDRICAL_SURFACE ( 'NONE', #23031, 3.799999999999999822 ) ;
#7317 = ORIENTED_EDGE ( 'NONE', *, *, #20316, .F. ) ;
#7318 = EDGE_LOOP ( 'NONE', ( #12183, #5164, #7561, #27596 ) ) ;
#7319 = AXIS2_PLACEMENT_3D ( 'NONE', #13739, #2776, #32995 ) ;
#7320 = DIRECTION ( 'NONE',  ( -1.000000000000000000, 0.000000000000000000, 0.000000000000000000 ) ) ;
#7321 = CIRCLE ( 'NONE', #2159, 52.00000000000000711 ) ;
#7322 = PRESENTATION_LAYER_ASSIGNMENT (  '', '', ( #30331 ) ) ;
#7323 = EDGE_CURVE ( 'NONE', #11554, #16212, #11902, .T. ) ;
#7324 = DIRECTION ( 'NONE',  ( -1.000000000000000000, -0.000000000000000000, -0.000000000000000000 ) ) ;
#7325 = ORIENTED_EDGE ( 'NONE', *, *, #33112, .F. ) ;
#7326 = ORIENTED_EDGE ( 'NONE', *, *, #23562, .F. ) ;
#7327 = DIRECTION ( 'NONE',  ( -1.000000000000000000, 0.000000000000000000, 0.000000000000000000 ) ) ;
#7328 = CARTESIAN_POINT ( 'NONE',  ( 0.000000000000000000, 0.000000000000000000, 0.000000000000000000 ) ) ;
#7329 = VERTEX_POINT ( 'NONE', #14152 ) ;
#7330 = DIRECTION ( 'NONE',  ( 0.000000000000000000, -0.2486898871648622888, 0.9685831611286290777 ) ) ;
#7331 = AXIS2_PLACEMENT_3D ( 'NONE', #35603, #18847, #30373 ) ;
#7332 = CARTESIAN_POINT ( 'NONE',  ( 2.600000000000004974, -12.74999999999999822, -1.691777834109592378E-31 ) ) ;
#7333 = CARTESIAN_POINT ( 'NONE',  ( 0.000000000000000000, 0.000000000000000000, -43.60000000000000142 ) ) ;
#7334 = CARTESIAN_POINT ( 'NONE',  ( -34.50000000000000000, -115.9929510916434481, 12.39849696637031684 ) ) ;
#7335 = CARTESIAN_POINT ( 'NONE',  ( 1.799999999999996048, 0.000000000000000000, 0.000000000000000000 ) ) ;
#7336 = CARTESIAN_POINT ( 'NONE',  ( -35.00000000000000000, -114.0592624029313242, 4.503524454178448266 ) ) ;
#7337 = CARTESIAN_POINT ( 'NONE',  ( -34.50000000000000000, -115.9929510916434481, 10.52000928670414126 ) ) ;
#7338 = DIRECTION ( 'NONE',  ( 0.000000000000000000, 0.3420201433256629953, 0.9396926207859104263 ) ) ;
#7339 = AXIS2_PLACEMENT_3D ( 'NONE', #19358, #30366, #27496 ) ;
#7340 = TOROIDAL_SURFACE ( 'NONE', #3349, 6.983999999999990216, 0.04100000000000673939 ) ;
#7341 = EDGE_CURVE ( 'NONE', #14392, #14078, #25156, .T. ) ;
#7342 = DIRECTION ( 'NONE',  ( -1.174092375852890260E-15, 4.222049128630259891E-16, 1.000000000000000000 ) ) ;
#7343 = AXIS2_PLACEMENT_3D ( 'NONE', #15130, #17669, #28669 ) ;
#7344 = DIRECTION ( 'NONE',  ( 1.000000000000000000, 0.000000000000000000, 0.000000000000000000 ) ) ;
#7345 = DIRECTION ( 'NONE',  ( 1.110223024625156540E-16, 1.000000000000000000, 0.000000000000000000 ) ) ;
#7347 = EDGE_CURVE ( 'NONE', #24556, #7742, #21091, .T. ) ;
#7346 = APPLICATION_CONTEXT ( 'automotive_design' ) ;
#7348 = EDGE_CURVE ( 'NONE', #6171, #34917, #31468, .T. ) ;
#7349 = DIRECTION ( 'NONE',  ( -1.000000000000000000, 0.000000000000000000, 0.000000000000000000 ) ) ;
#7350 = VERTEX_POINT ( 'NONE', #19712 ) ;
#7351 = CARTESIAN_POINT ( 'NONE',  ( -35.81662171581203324, -110.9754527089670546, 9.715225545821551734 ) ) ;
#7352 = VECTOR ( 'NONE', #19436, 1000.000000000000000 ) ;
#7353 = DIRECTION ( 'NONE',  ( 0.000000000000000000, 0.000000000000000000, 1.000000000000000000 ) ) ;
#7354 = CARTESIAN_POINT ( 'NONE',  ( -35.50000000000000000, -113.0140978167138712, 0.8752176474016720720 ) ) ;
#7355 = ORIENTED_EDGE ( 'NONE', *, *, #11892, .T. ) ;
#7356 = ORIENTED_EDGE ( 'NONE', *, *, #27956, .F. ) ;
#7357 = DIRECTION ( 'NONE',  ( -1.000000000000000000, 0.000000000000000000, 0.000000000000000000 ) ) ;
#7358 = CARTESIAN_POINT ( 'NONE',  ( 8.000000000000000000, 14.18878633068169925, -6.236773481717946765 ) ) ;
#7359 = ORIENTED_EDGE ( 'NONE', *, *, #27347, .F. ) ;
#7360 = EDGE_CURVE ( 'NONE', #8438, #10152, #12475, .T. ) ;
#7361 = VERTEX_POINT ( 'NONE', #3382 ) ;
#7362 = EDGE_CURVE ( 'NONE', #11298, #33791, #126, .T. ) ;
#7363 = ORIENTED_EDGE ( 'NONE', *, *, #19417, .F. ) ;
#7364 = CIRCLE ( 'NONE', #28053, 20.00000000000001066 ) ;
#7365 = CARTESIAN_POINT ( 'NONE',  ( 7.999999999999992895, -39.78933988720132220, 24.98727647984988565 ) ) ;
#7366 = DIRECTION ( 'NONE',  ( 0.000000000000000000, 0.000000000000000000, 1.000000000000000000 ) ) ;
#7367 = DIRECTION ( 'NONE',  ( -1.000000000000000000, -2.084812053021932845E-17, -2.283206711915154518E-18 ) ) ;
#7368 = CARTESIAN_POINT ( 'NONE',  ( 7.999999999999992895, 0.000000000000000000, 0.000000000000000000 ) ) ;
#7369 = VERTEX_POINT ( 'NONE', #22084 ) ;
#7370 = ORIENTED_EDGE ( 'NONE', *, *, #22769, .T. ) ;
#7371 = CARTESIAN_POINT ( 'NONE',  ( -35.50000000000000711, -112.7472371723319355, 1.839427296857320648 ) ) ;
#7372 = AXIS2_PLACEMENT_3D ( 'NONE', #33605, #12009, #31096 ) ;
#7373 = CYLINDRICAL_SURFACE ( 'NONE', #11088, 6.000000000000005329 ) ;
#7374 = CARTESIAN_POINT ( 'NONE',  ( -1.799999999999996048, 0.000000000000000000, 0.000000000000000000 ) ) ;
#7375 = ORIENTED_EDGE ( 'NONE', *, *, #21969, .F. ) ;
#7376 = MECHANICAL_DESIGN_GEOMETRIC_PRESENTATION_REPRESENTATION (  '', ( #22884 ), #3380 ) ;
#7377 = LINE ( 'NONE', #5391, #27015 ) ;
#7378 = CYLINDRICAL_SURFACE ( 'NONE', #30521, 7.199999999999994849 ) ;
#7379 = CARTESIAN_POINT ( 'NONE',  ( -34.50000000000000000, -114.9819937217110635, 10.35556074009299188 ) ) ;
#7380 = CARTESIAN_POINT ( 'NONE',  ( 0.000000000000000000, 10.46102064772339979, 19.35373470438986843 ) ) ;
#7381 = CARTESIAN_POINT ( 'NONE',  ( -36.00585935943767169, -114.9929510916434339, 13.11852578240983291 ) ) ;
#7382 = LINE ( 'NONE', #15994, #16253 ) ;
#7383 = CARTESIAN_POINT ( 'NONE',  ( -39.00000000000000000, -113.9929510916434339, 12.26648026267477221 ) ) ;
#7384 = CARTESIAN_POINT ( 'NONE',  ( 8.000000000000000000, 0.000000000000000000, 0.000000000000000000 ) ) ;
#7385 = EDGE_CURVE ( 'NONE', #17296, #12175, #19380, .T. ) ;
#7386 = CARTESIAN_POINT ( 'NONE',  ( -10.00000000000000000, 0.000000000000000000, 0.000000000000000000 ) ) ;
#7387 = FACE_OUTER_BOUND ( 'NONE', #30294, .T. ) ;
#7388 = ORIENTED_EDGE ( 'NONE', *, *, #28035, .F. ) ;
#7389 = CYLINDRICAL_SURFACE ( 'NONE', #8929, 47.49900000000001654 ) ;
#7390 = CARTESIAN_POINT ( 'NONE',  ( -9.999999999999994671, 0.000000000000000000, 0.000000000000000000 ) ) ;
#7391 = EDGE_CURVE ( 'NONE', #12602, #25795, #22252, .T. ) ;
#7392 = ORIENTED_EDGE ( 'NONE', *, *, #20073, .F. ) ;
#7393 = CARTESIAN_POINT ( 'NONE',  ( -35.96730626674924025, -114.9929510916434339, 13.11752178341330044 ) ) ;
#7394 = ORIENTED_EDGE ( 'NONE', *, *, #28358, .F. ) ;
#7395 = AXIS2_PLACEMENT_3D ( 'NONE', #20620, #31980, #4278 ) ;
#7396 = CARTESIAN_POINT ( 'NONE',  ( -34.97545270896703329, -113.2308352781851539, 4.409774454178448266 ) ) ;
#7397 = CARTESIAN_POINT ( 'NONE',  ( 7.999999999999992895, -40.47821179127691948, -32.64221760512803172 ) ) ;
#7398 = EDGE_LOOP ( 'NONE', ( #34738, #12311, #30821, #23289 ) ) ;
#7399 = VECTOR ( 'NONE', #9307, 1000.000000000000000 ) ;
#7400 = VERTEX_POINT ( 'NONE', #21847 ) ;
#7401 = CARTESIAN_POINT ( 'NONE',  ( -38.37230871539094323, -112.5438815906447729, 8.441024454178448266 ) ) ;
#7402 = ORIENTED_EDGE ( 'NONE', *, *, #31805, .F. ) ;
#7403 = CARTESIAN_POINT ( 'NONE',  ( -40.02454729103296671, -115.1833782841879525, 3.659774454178448710 ) ) ;
#7404 = CARTESIAN_POINT ( 'NONE',  ( 7.999999999999992895, -6.109652351741458709, -46.58570277113513214 ) ) ;
#7405 = CARTESIAN_POINT ( 'NONE',  ( 7.999999999999992895, 46.90537658765334328, -2.727856614653800804 ) ) ;
#7406 = VERTEX_POINT ( 'NONE', #27451 ) ;
#7407 = VERTEX_POINT ( 'NONE', #10882 ) ;
#7408 = CARTESIAN_POINT ( 'NONE',  ( -3.160591952521663028, -3.281206521718052382, -0.7999999999999951594 ) ) ;
#7409 = LINE ( 'NONE', #13, #10973 ) ;
#7410 = ORIENTED_EDGE ( 'NONE', *, *, #7425, .T. ) ;
#7411 = ORIENTED_EDGE ( 'NONE', *, *, #18010, .T. ) ;
#7412 = CARTESIAN_POINT ( 'NONE',  ( -34.50000000000000000, -111.0173113992184710, -0.7556348869410824953 ) ) ;
#7413 = DIRECTION ( 'NONE',  ( -1.000000000000000000, 0.000000000000000000, 0.000000000000000000 ) ) ;
#7414 = ORIENTED_EDGE ( 'NONE', *, *, #19628, .F. ) ;
#7415 = ORIENTED_EDGE ( 'NONE', *, *, #9816, .T. ) ;
#7416 = DIRECTION ( 'NONE',  ( -1.000000000000000000, 0.000000000000000000, 0.000000000000000000 ) ) ;
#7417 = CIRCLE ( 'NONE', #15440, 7.199999999999990408 ) ;
#7418 = CARTESIAN_POINT ( 'NONE',  ( -38.00000000000000711, -113.9929510916434339, 12.59102132592609102 ) ) ;
#7419 = DIRECTION ( 'NONE',  ( 0.000000000000000000, -1.000000000000000000, 0.000000000000000000 ) ) ;
#7420 = DIRECTION ( 'NONE',  ( 0.000000000000000000, 0.6845471059286846183, 0.7289686274214154382 ) ) ;
#7421 = CARTESIAN_POINT ( 'NONE',  ( -34.50000000000000000, -113.9557924591415627, 10.50182206170499555 ) ) ;
#7422 = CARTESIAN_POINT ( 'NONE',  ( -37.24999999999992184, -115.9929510916434481, 13.11852480586264846 ) ) ;
#7423 = FACE_OUTER_BOUND ( 'NONE', #35224, .T. ) ;
#7424 = PLANE ( 'NONE',  #27331 ) ;
#7425 = EDGE_CURVE ( 'NONE', #4708, #9210, #18793, .T. ) ;
#7426 = ORIENTED_EDGE ( 'NONE', *, *, #20550, .F. ) ;
#7427 = DIRECTION ( 'NONE',  ( 0.000000000000000000, 0.000000000000000000, 1.000000000000000000 ) ) ;
#7428 = DIRECTION ( 'NONE',  ( 0.000000000000000000, 0.000000000000000000, 1.000000000000000000 ) ) ;
#7429 = LINE ( 'NONE', #17868, #21456 ) ;
#7430 = ORIENTED_EDGE ( 'NONE', *, *, #14341, .T. ) ;
#7431 = CARTESIAN_POINT ( 'NONE',  ( 8.000000000000000000, -9.471478019455243924, 14.71414642875952161 ) ) ;
#7432 = CARTESIAN_POINT ( 'NONE',  ( -35.50000000000000711, -112.9813730236132585, -1.624774171495860786 ) ) ;
#7433 = CARTESIAN_POINT ( 'NONE',  ( -34.49999999999998579, -13.10640646055107084, 90.70096189432331357 ) ) ;
#7434 = AXIS2_PLACEMENT_3D ( 'NONE', #7328, #18300, #4649 ) ;
#7435 = EDGE_CURVE ( 'NONE', #14850, #29835, #23394, .T. ) ;
#7436 = CARTESIAN_POINT ( 'NONE',  ( -35.50000000000000711, -114.6604609523327838, 9.751889438017201428 ) ) ;
#7437 = CYLINDRICAL_SURFACE ( 'NONE', #1563, 20.00000000000000355 ) ;
#7438 = VERTEX_POINT ( 'NONE', #32839 ) ;
#7439 = VECTOR ( 'NONE', #9763, 1000.000000000000000 ) ;
#7440 = DIRECTION ( 'NONE',  ( -1.000000000000000000, 0.000000000000000000, 0.000000000000000000 ) ) ;
#7441 = CARTESIAN_POINT ( 'NONE',  ( -35.50000000000000000, -112.3070160848889429, 2.749963775944984867 ) ) ;
#7442 = DIRECTION ( 'NONE',  ( -1.000000000000000000, 0.000000000000000000, 0.000000000000000000 ) ) ;
#7443 = VERTEX_POINT ( 'NONE', #29798 ) ;
#7444 = ORIENTED_EDGE ( 'NONE', *, *, #1176, .T. ) ;
#7445 = CARTESIAN_POINT ( 'NONE',  ( -38.99999999999999289, -113.9407375970686900, 3.753524454178449155 ) ) ;
#7446 = AXIS2_PLACEMENT_3D ( 'NONE', #17286, #3633, #28955 ) ;
#7447 = CARTESIAN_POINT ( 'NONE',  ( 7.999999999999992895, -32.32520163883607722, 34.09746168776025854 ) ) ;
#7448 = ORIENTED_EDGE ( 'NONE', *, *, #20746, .F. ) ;
#7449 = ORIENTED_EDGE ( 'NONE', *, *, #15260, .F. ) ;
#7450 = CARTESIAN_POINT ( 'NONE',  ( -34.50000000000000000, -113.0140978167136581, -0.6247823525984261828 ) ) ;
#7451 = DIRECTION ( 'NONE',  ( -1.000000000000000000, 0.000000000000000000, 0.000000000000000000 ) ) ;
#7452 = DIRECTION ( 'NONE',  ( 0.000000000000000000, 0.000000000000000000, -1.000000000000000000 ) ) ;
#7453 = CARTESIAN_POINT ( 'NONE',  ( -35.50000000000000000, -113.9186338266397058, 10.49738657667399266 ) ) ;
#7454 = CARTESIAN_POINT ( 'NONE',  ( -34.49999999999998579, -25.98076211353322051, 84.99999999999992895 ) ) ;
#7455 = CARTESIAN_POINT ( 'NONE',  ( -34.50000000000000000, -112.0209493036498287, 0.9959249592223760050 ) ) ;
#7456 = CARTESIAN_POINT ( 'NONE',  ( -34.50481333282507279, -114.9929510916434339, 12.74107470552716492 ) ) ;
#7457 = DIRECTION ( 'NONE',  ( -1.174092375852890260E-15, 4.222049128630259891E-16, 1.000000000000000000 ) ) ;
#7458 = AXIS2_PLACEMENT_3D ( 'NONE', #29527, #7893, #21223 ) ;
#7459 = EDGE_CURVE ( 'NONE', #31803, #32697, #14186, .T. ) ;
#7460 = EDGE_CURVE ( 'NONE', #23680, #16526, #7863, .T. ) ;
#7461 = DIRECTION ( 'NONE',  ( 0.000000000000000000, -0.8660254037844327124, -0.5000000000000104361 ) ) ;
#7462 = ORIENTED_EDGE ( 'NONE', *, *, #30839, .F. ) ;
#7463 = PRODUCT_DEFINITION_FORMATION_WITH_SPECIFIED_SOURCE ( 'ANY', '', #15545, .NOT_KNOWN. ) ;
#7464 = CARTESIAN_POINT ( 'NONE',  ( -35.69272627125608466, -115.9929510916434481, 13.01835785830562209 ) ) ;
#7465 = CARTESIAN_POINT ( 'NONE',  ( -35.50000000000000711, -114.1807644833817648, -1.624782352598427959 ) ) ;
#7466 = CARTESIAN_POINT ( 'NONE',  ( 115.0000000000000000, 81.48267994499606459, 37.65054357219658243 ) ) ;
#7467 = VECTOR ( 'NONE', #13834, 1000.000000000000000 ) ;
#7468 = CARTESIAN_POINT ( 'NONE',  ( 8.000000000000000000, -10.46102064772354723, 19.35373470438981514 ) ) ;
#7469 = DIRECTION ( 'NONE',  ( 0.000000000000000000, 0.2538061376417690140, 0.9672551082808337197 ) ) ;
#7470 = ORIENTED_EDGE ( 'NONE', *, *, #33855, .T. ) ;
#7471 = DIRECTION ( 'NONE',  ( 0.000000000000000000, 0.000000000000000000, 1.000000000000000000 ) ) ;
#7472 = DIRECTION ( 'NONE',  ( 1.000000000000000000, 0.000000000000000000, 0.000000000000000000 ) ) ;
#7473 = CYLINDRICAL_SURFACE ( 'NONE', #26285, 17.49900000000000233 ) ;
#7474 = CARTESIAN_POINT ( 'NONE',  ( 8.000000000000000000, 11.11653975335807587, -12.74840161668719851 ) ) ;
#7475 = EDGE_CURVE ( 'NONE', #24024, #9557, #27092, .T. ) ;
#7476 = CARTESIAN_POINT ( 'NONE',  ( -36.52652403469556930, -113.0245472910329880, 7.222274454178449155 ) ) ;
#7477 = FACE_OUTER_BOUND ( 'NONE', #26328, .T. ) ;
#7478 = CARTESIAN_POINT ( 'NONE',  ( 50.00000000000000711, 0.000000000000000000, 70.00000000000000000 ) ) ;
#7479 = EDGE_CURVE ( 'NONE', #32761, #28824, #35559, .T. ) ;
#7480 = VERTEX_POINT ( 'NONE', #7990 ) ;
#7481 = VERTEX_POINT ( 'NONE', #29433 ) ;
#7482 = FACE_BOUND ( 'NONE', #19426, .T. ) ;
#7483 = CARTESIAN_POINT ( 'NONE',  ( 3.872983346207416133, 1.000000000000001110, 55.00000000000000000 ) ) ;
#7484 = ORIENTED_EDGE ( 'NONE', *, *, #24002, .F. ) ;
#7485 = CARTESIAN_POINT ( 'NONE',  ( -39.02454729103295961, -113.2308352781851539, 6.340225545821550845 ) ) ;
#7486 = ORIENTED_EDGE ( 'NONE', *, *, #22024, .T. ) ;
#7487 = EDGE_LOOP ( 'NONE', ( #2998, #1669 ) ) ;
#7488 = ORIENTED_EDGE ( 'NONE', *, *, #22566, .F. ) ;
#7489 = LINE ( 'NONE', #18472, #11422 ) ;
#7490 = AXIS2_PLACEMENT_3D ( 'NONE', #28335, #25642, #17155 ) ;
#7491 = VECTOR ( 'NONE', #23799, 1000.000000000000000 ) ;
#7492 = EDGE_CURVE ( 'NONE', #14157, #28884, #13233, .T. ) ;
#7493 = CARTESIAN_POINT ( 'NONE',  ( 112.0000000000000000, 81.48267994499606459, 30.15054357219658954 ) ) ;
#7494 = ORIENTED_EDGE ( 'NONE', *, *, #1630, .F. ) ;
#7495 = ORIENTED_EDGE ( 'NONE', *, *, #15610, .F. ) ;
#7496 = CARTESIAN_POINT ( 'NONE',  ( -9.999999999999994671, 0.000000000000000000, 0.000000000000000000 ) ) ;
#7497 = LINE ( 'NONE', #10562, #4015 ) ;
#7498 = ORIENTED_EDGE ( 'NONE', *, *, #5562, .F. ) ;
#7499 = DIRECTION ( 'NONE',  ( 1.000000000000000000, 0.000000000000000000, 0.000000000000000000 ) ) ;
#7500 = CARTESIAN_POINT ( 'NONE',  ( -34.49999999999998579, -13.10640646055107084, 90.70096189432331357 ) ) ;
#7501 = DIRECTION ( 'NONE',  ( -1.000000000000000000, 0.000000000000000000, -0.000000000000000000 ) ) ;
#7502 = EDGE_CURVE ( 'NONE', #20170, #7837, #24206, .T. ) ;
#7503 = EDGE_CURVE ( 'NONE', #4040, #23706, #4950, .T. ) ;
#7504 = CIRCLE ( 'NONE', #21920, 20.00000000000000355 ) ;
#7505 = CARTESIAN_POINT ( 'NONE',  ( -35.00000000000000000, -114.0000000000003411, 9.500000000000035527 ) ) ;
#7506 = CARTESIAN_POINT ( 'NONE',  ( -36.11231047232249836, -112.0245472910329880, 8.722274454178448266 ) ) ;
#7507 = EDGE_CURVE ( 'NONE', #21532, #30052, #34932, .T. ) ;
#7508 = CARTESIAN_POINT ( 'NONE',  ( -34.50000000000000000, -115.9929510916434481, 10.68227981832981044 ) ) ;
#7509 = CARTESIAN_POINT ( 'NONE',  ( 0.000000000000000000, -2.710505431213761085E-17, 45.99999999999998579 ) ) ;
#7510 = CARTESIAN_POINT ( 'NONE',  ( 8.000000000000000000, 8.605879768205412006, -12.89022243466699535 ) ) ;
#7511 = CIRCLE ( 'NONE', #29938, 7.199999999999986855 ) ;
#7512 = FACE_OUTER_BOUND ( 'NONE', #27935, .T. ) ;
#7513 = CARTESIAN_POINT ( 'NONE',  ( 0.000000000000000000, 0.000000000000000000, -39.50000000000000711 ) ) ;
#7514 = LINE ( 'NONE', #18132, #13610 ) ;
#7515 = VERTEX_POINT ( 'NONE', #2432 ) ;
#7516 = EDGE_CURVE ( 'NONE', #4505, #8054, #26738, .T. ) ;
#7517 = AXIS2_PLACEMENT_3D ( 'NONE', #16405, #16594, #13551 ) ;
#7518 = CARTESIAN_POINT ( 'NONE',  ( -37.05926240293131713, -112.0000000000000142, 3.621475545821551290 ) ) ;
#7519 = AXIS2_PLACEMENT_3D ( 'NONE', #1660, #1123, #4365 ) ;
#7520 = DIRECTION ( 'NONE',  ( 1.000000000000000000, 0.000000000000000000, 0.000000000000000000 ) ) ;
#7521 = LINE ( 'NONE', #26799, #12487 ) ;
#7522 = EDGE_CURVE ( 'NONE', #24075, #30211, #16492, .T. ) ;
#7523 = AXIS2_PLACEMENT_3D ( 'NONE', #16515, #24641, #23559 ) ;
#7524 = ORIENTED_EDGE ( 'NONE', *, *, #26877, .T. ) ;
#7525 = ORIENTED_EDGE ( 'NONE', *, *, #34561, .F. ) ;
#7527 = CYLINDRICAL_SURFACE ( 'NONE', #2236, 4.800000000000000711 ) ;
#7526 = PRODUCT ( 'spur gear_iso_ISO - Spur gear 2M 18T 20PA 8FW ---S18A75H50L8.0S1', 'spur gear_iso_ISO - Spur gear 2M 18T 20PA 8FW ---S18A75H50L8.0S1', '', ( #14508 ) ) ;
#7528 = LINE ( 'NONE', #7358, #32445 ) ;
#7529 = VERTEX_POINT ( 'NONE', #29614 ) ;
#7530 = ORIENTED_EDGE ( 'NONE', *, *, #8163, .T. ) ;
#7531 = ORIENTED_EDGE ( 'NONE', *, *, #13427, .T. ) ;
#7532 = CARTESIAN_POINT ( 'NONE',  ( 7.999999999999992895, 0.000000000000000000, 0.000000000000000000 ) ) ;
#7533 = DIRECTION ( 'NONE',  ( 1.000000000000000000, 0.000000000000000000, 0.000000000000000000 ) ) ;
#7534 = DIRECTION ( 'NONE',  ( 0.000000000000000000, 0.000000000000000000, -1.000000000000000000 ) ) ;
#7535 = EDGE_CURVE ( 'NONE', #5141, #13387, #3880, .T. ) ;
#7536 = CARTESIAN_POINT ( 'NONE',  ( 7.999999999999992895, -45.78515115856053797, 12.64416602183649019 ) ) ;
#7537 = EDGE_LOOP ( 'NONE', ( #5246, #24816, #31177, #11344 ) ) ;
#7538 = EDGE_LOOP ( 'NONE', ( #13140, #18016, #8020, #16187 ) ) ;
#7539 = CARTESIAN_POINT ( 'NONE',  ( -35.50000000000000711, -112.0140978167138712, -0.5622823525984296245 ) ) ;
#7540 = EDGE_CURVE ( 'NONE', #29334, #4579, #24004, .T. ) ;
#7541 = DIRECTION ( 'NONE',  ( 0.000000000000000000, 0.000000000000000000, 1.000000000000000000 ) ) ;
#7542 = DIRECTION ( 'NONE',  ( 0.000000000000000000, 0.000000000000000000, 1.000000000000000000 ) ) ;
#7543 = ORIENTED_EDGE ( 'NONE', *, *, #34012, .T. ) ;
#7544 = CIRCLE ( 'NONE', #23059, 12.55910585664918422 ) ;
#7545 = CARTESIAN_POINT ( 'NONE',  ( -21.15833593587365513, -21.98076211353320630, 86.49999999999995737 ) ) ;
#7546 = DIRECTION ( 'NONE',  ( 0.000000000000000000, 0.000000000000000000, 1.000000000000000000 ) ) ;
#7547 = CARTESIAN_POINT ( 'NONE',  ( -34.50000000000000000, -114.9929510916434339, 12.59102132592610523 ) ) ;
#7548 = DIRECTION ( 'NONE',  ( 0.000000000000000000, 0.000000000000000000, -1.000000000000000000 ) ) ;
#7549 = EDGE_CURVE ( 'NONE', #19623, #453, #33190, .T. ) ;
#7550 = CARTESIAN_POINT ( 'NONE',  ( -37.42187499999997158, -114.9929510916434339, 13.11852480586264669 ) ) ;
#7551 = DIRECTION ( 'NONE',  ( 0.000000000000000000, 0.000000000000000000, 1.000000000000000000 ) ) ;
#7552 = EDGE_CURVE ( 'NONE', #13661, #13787, #992, .T. ) ;
#7553 = CARTESIAN_POINT ( 'NONE',  ( -34.50000000000000000, -114.1068310684433129, 9.512752019463897923 ) ) ;
#7554 = DIRECTION ( 'NONE',  ( -1.000000000000000000, 0.000000000000000000, 0.000000000000000000 ) ) ;
#7555 = CARTESIAN_POINT ( 'NONE',  ( -38.00000000000000711, -114.9929510916434339, 12.59102132592608925 ) ) ;
#7556 = ORIENTED_EDGE ( 'NONE', *, *, #1254, .F. ) ;
#7557 = CARTESIAN_POINT ( 'NONE',  ( 6.071532165918824830E-15, 1.000000000000000000, -22.00000000000000000 ) ) ;
#7558 = DIRECTION ( 'NONE',  ( 0.000000000000000000, 0.000000000000000000, -1.000000000000000000 ) ) ;
#7559 = ORIENTED_EDGE ( 'NONE', *, *, #925, .F. ) ;
#7560 = CARTESIAN_POINT ( 'NONE',  ( -37.97447287825094975, -114.9929510916434339, 12.77960891308616809 ) ) ;
#7561 = ORIENTED_EDGE ( 'NONE', *, *, #15830, .T. ) ;
#7562 = CARTESIAN_POINT ( 'NONE',  ( -38.37230871539094323, -112.5438815906447729, 8.441024454178448266 ) ) ;
#7563 = CARTESIAN_POINT ( 'NONE',  ( 70.00000000000001421, -35.39471919948800149, 89.19850115919967948 ) ) ;
#7564 = ORIENTED_EDGE ( 'NONE', *, *, #24730, .F. ) ;
#7565 = ORIENTED_EDGE ( 'NONE', *, *, #12189, .F. ) ;
#7566 = FACE_OUTER_BOUND ( 'NONE', #29465, .T. ) ;
#7567 = VECTOR ( 'NONE', #12998, 1000.000000000000000 ) ;
#7568 =( GEOMETRIC_REPRESENTATION_CONTEXT ( 3 ) GLOBAL_UNCERTAINTY_ASSIGNED_CONTEXT ( ( #28039 ) ) GLOBAL_UNIT_ASSIGNED_CONTEXT ( ( #17842, #34065, #31886 ) ) REPRESENTATION_CONTEXT ( 'NONE', 'WORKASPACE' ) );
#7569 = EDGE_LOOP ( 'NONE', ( #25841, #3656, #2365, #21582 ) ) ;
#7570 = VECTOR ( 'NONE', #13440, 1000.000000000000000 ) ;
#7571 = CARTESIAN_POINT ( 'NONE',  ( -33.97545270896702618, -112.8166217158120475, 2.909774454178449155 ) ) ;
#7572 = DIRECTION ( 'NONE',  ( -1.000000000000000000, 0.000000000000000000, 0.000000000000000000 ) ) ;
#7573 = CARTESIAN_POINT ( 'NONE',  ( 8.000000000000007105, -9.637487275701184686, 10.15474465512046542 ) ) ;
#7574 = ORIENTED_EDGE ( 'NONE', *, *, #29836, .T. ) ;
#7575 = EDGE_LOOP ( 'NONE', ( #21540, #23839, #7355, #19749 ) ) ;
#7576 = CARTESIAN_POINT ( 'NONE',  ( 70.00001200000001234, -25.45716333793490449, 88.99999999999995737 ) ) ;
#7577 = EDGE_CURVE ( 'NONE', #21336, #14025, #17652, .T. ) ;
#7578 = CARTESIAN_POINT ( 'NONE',  ( -10.00000000000000178, 0.000000000000000000, 0.000000000000000000 ) ) ;
#7579 = ORIENTED_EDGE ( 'NONE', *, *, #26743, .T. ) ;
#7580 = ORIENTED_EDGE ( 'NONE', *, *, #10023, .T. ) ;
#7581 = CARTESIAN_POINT ( 'NONE',  ( -34.50000000000000000, -111.0140978167138570, -0.4685323525984296800 ) ) ;
#7582 = ADVANCED_FACE ( 'NONE', ( #35029 ), #8689, .F. ) ;
#7583 = DIRECTION ( 'NONE',  ( 0.000000000000000000, 0.8443279255020164076, -0.5358267949789946583 ) ) ;
#7584 = VERTEX_POINT ( 'NONE', #27629 ) ;
#7585 = CARTESIAN_POINT ( 'NONE',  ( -35.50000000000000711, -114.1489256397697289, 9.518467544735724317 ) ) ;
#7586 = CARTESIAN_POINT ( 'NONE',  ( -34.50000000000000000, -113.9929510916434339, 10.50625754673587409 ) ) ;
#7587 = DIRECTION ( 'NONE',  ( 0.000000000000000000, 0.2486898871648483555, 0.9685831611286328524 ) ) ;
#7588 = DIRECTION ( 'NONE',  ( 0.000000000000000000, 0.000000000000000000, 1.000000000000000000 ) ) ;
#7589 = AXIS2_PLACEMENT_3D ( 'NONE', #8026, #11094, #16288 ) ;
#7590 = CARTESIAN_POINT ( 'NONE',  ( -37.43749999999998579, -113.9929510916434339, 13.11852480586264846 ) ) ;
#7591 = CARTESIAN_POINT ( 'NONE',  ( -37.99959864031216483, -115.9929510916434481, 12.63896776382213538 ) ) ;
#7592 = DIRECTION ( 'NONE',  ( 0.000000000000000000, 0.000000000000000000, -1.000000000000000000 ) ) ;
#7593 = DIRECTION ( 'NONE',  ( 0.000000000000000000, 0.000000000000000000, 1.000000000000000000 ) ) ;
#7594 = ORIENTED_EDGE ( 'NONE', *, *, #26167, .T. ) ;
#7595 = LINE ( 'NONE', #5628, #19510 ) ;
#7596 = FACE_OUTER_BOUND ( 'NONE', #14119, .T. ) ;
#7597 = FACE_OUTER_BOUND ( 'NONE', #26050, .T. ) ;
#7598 = EDGE_LOOP ( 'NONE', ( #21202, #26690, #24766, #18163 ) ) ;
#7599 = AXIS2_PLACEMENT_3D ( 'NONE', #11234, #28153, #777 ) ;
#7600 = DIRECTION ( 'NONE',  ( -1.000000000000000000, -1.734723475976807094E-16, 0.000000000000000000 ) ) ;
#7601 = CARTESIAN_POINT ( 'NONE',  ( -35.50000000000000711, -112.3995503592287690, -1.424448457485529618 ) ) ;
#7602 = DIRECTION ( 'NONE',  ( 0.000000000000000000, 0.000000000000000000, -1.000000000000000000 ) ) ;
#7603 = CARTESIAN_POINT ( 'NONE',  ( -35.50000102263782509, -114.9929510916434339, 12.62466071271731316 ) ) ;
#7604 = FACE_OUTER_BOUND ( 'NONE', #34444, .T. ) ;
#7605 = ORIENTED_EDGE ( 'NONE', *, *, #31891, .F. ) ;
#7606 = DIRECTION ( 'NONE',  ( 0.000000000000000000, -0.4999999999999989453, -0.8660254037844392627 ) ) ;
#7607 = CARTESIAN_POINT ( 'NONE',  ( -35.50000000000000000, -111.0140978167138570, 0.8127176474015720409 ) ) ;
#7608 = CIRCLE ( 'NONE', #27751, 4.000000000000003553 ) ;
#7609 = ORIENTED_EDGE ( 'NONE', *, *, #8189, .T. ) ;
#7610 = VERTEX_POINT ( 'NONE', #25268 ) ;
#7611 = CARTESIAN_POINT ( 'NONE',  ( -35.00000000000000000, -114.0592624029313242, 1.503524454178448710 ) ) ;
#7612 = AXIS2_PLACEMENT_3D ( 'NONE', #25114, #30168, #19854 ) ;
#7613 = AXIS2_PLACEMENT_3D ( 'NONE', #32663, #19306, #35369 ) ;
#7614 = CARTESIAN_POINT ( 'NONE',  ( 0.000000000000000000, 5.399999999999999467, -1.000000000000003109 ) ) ;
#7615 = EDGE_LOOP ( 'NONE', ( #33702, #6159, #32414, #32946 ) ) ;
#7616 = ORIENTED_EDGE ( 'NONE', *, *, #8153, .F. ) ;
#7617 = CARTESIAN_POINT ( 'NONE',  ( -34.50000000000000000, -113.0974311500471714, -0.6247823525984269599 ) ) ;
#7618 = EDGE_CURVE ( 'NONE', #2675, #2022, #591, .T. ) ;
#7619 = DIRECTION ( 'NONE',  ( 0.000000000000000000, -6.938893903907203726E-17, -1.000000000000000000 ) ) ;
#7620 = DIRECTION ( 'NONE',  ( 0.000000000000000000, 0.000000000000000000, 1.000000000000000000 ) ) ;
#7621 = AXIS2_PLACEMENT_3D ( 'NONE', #17691, #18224, #20737 ) ;
#7622 = VECTOR ( 'NONE', #17357, 1000.000000000000000 ) ;
#7623 = CARTESIAN_POINT ( 'NONE',  ( -37.99899697755054717, -114.9929510916434339, 12.65121853911336736 ) ) ;
#7624 = AXIS2_PLACEMENT_3D ( 'NONE', #29626, #4965, #22207 ) ;
#7625 = LINE ( 'NONE', #27450, #590 ) ;
#7626 = DIRECTION ( 'NONE',  ( 0.000000000000000000, -0.4999999999999928946, -0.8660254037844427044 ) ) ;
#7627 = EDGE_CURVE ( 'NONE', #6287, #14457, #25720, .T. ) ;
#7628 = CARTESIAN_POINT ( 'NONE',  ( -34.50000000000000000, -113.1807644833805426, -1.624782352598427959 ) ) ;
#7629 = DIRECTION ( 'NONE',  ( -1.000000000000000000, 0.000000000000000000, 0.000000000000000000 ) ) ;
#7630 = AXIS2_PLACEMENT_3D ( 'NONE', #6359, #427, #6190 ) ;
#7631 = CIRCLE ( 'NONE', #14506, 10.00000000000000000 ) ;
#7632 = CARTESIAN_POINT ( 'NONE',  ( -1.999999999999999112, 9.125740023391120405E-16, 4.200000000000014388 ) ) ;
#7633 = EDGE_LOOP ( 'NONE', ( #10864, #1281, #20210, #12900 ) ) ;
#7634 = CIRCLE ( 'NONE', #27786, 20.00000000000000711 ) ;
#7635 = CARTESIAN_POINT ( 'NONE',  ( -37.43749999999998579, -115.9929510916434481, 13.11852480586264846 ) ) ;
#7636 = DIRECTION ( 'NONE',  ( 0.000000000000000000, 0.000000000000000000, 1.000000000000000000 ) ) ;
#7637 = CARTESIAN_POINT ( 'NONE',  ( 0.000000000000000000, -1.111908866155017606, -9.433698091065132019 ) ) ;
#7638 = LINE ( 'NONE', #16260, #15909 ) ;
#7639 = ORIENTED_EDGE ( 'NONE', *, *, #35571, .T. ) ;
#7640 = DIRECTION ( 'NONE',  ( -1.000000000000000000, 0.000000000000000000, 0.000000000000000000 ) ) ;
#7641 = DIRECTION ( 'NONE',  ( 0.000000000000000000, 0.000000000000000000, -1.000000000000000000 ) ) ;
#7642 = FACE_OUTER_BOUND ( 'NONE', #11501, .T. ) ;
#7643 = DIRECTION ( 'NONE',  ( 0.000000000000000000, 0.000000000000000000, -1.000000000000000000 ) ) ;
#7644 = FACE_OUTER_BOUND ( 'NONE', #3609, .T. ) ;
#7645 = CARTESIAN_POINT ( 'NONE',  ( 55.00000000000000711, -25.98076211353320986, 91.99999999999994316 ) ) ;
#7646 = VERTEX_POINT ( 'NONE', #2964 ) ;
#7647 = EDGE_CURVE ( 'NONE', #28364, #4303, #5007, .T. ) ;
#7648 = AXIS2_PLACEMENT_3D ( 'NONE', #16692, #30222, #21393 ) ;
#7649 = ORIENTED_EDGE ( 'NONE', *, *, #10240, .F. ) ;
#7650 = DIRECTION ( 'NONE',  ( 0.000000000000000000, 1.000000000000000000, 0.000000000000000000 ) ) ;
#7651 = CIRCLE ( 'NONE', #19638, 20.00000000000000355 ) ;
#7652 = CARTESIAN_POINT ( 'NONE',  ( 4.000000000000000000, 4.898587196589412829E-16, -31.10000000000000142 ) ) ;
#7653 = DIRECTION ( 'NONE',  ( -1.000000000000000000, 0.000000000000000000, 0.000000000000000000 ) ) ;
#7654 = ORIENTED_EDGE ( 'NONE', *, *, #30217, .F. ) ;
#7655 = CARTESIAN_POINT ( 'NONE',  ( -38.37230871539094323, -115.4561184093552413, 6.058975545821551734 ) ) ;
#7656 = ORIENTED_EDGE ( 'NONE', *, *, #8445, .F. ) ;
#7657 = SURFACE_STYLE_USAGE ( .BOTH. , #32504 ) ;
#7658 = ORIENTED_EDGE ( 'NONE', *, *, #17331, .F. ) ;
#7659 = VERTEX_POINT ( 'NONE', #11746 ) ;
#7660 = DIRECTION ( 'NONE',  ( 1.000000000000000000, 0.000000000000000000, 0.000000000000000000 ) ) ;
#7661 = EDGE_CURVE ( 'NONE', #28491, #15607, #32597, .T. ) ;
#7662 = AXIS2_PLACEMENT_3D ( 'NONE', #1054, #12025, #28593 ) ;
#7663 = EDGE_CURVE ( 'NONE', #185, #20179, #19829, .T. ) ;
#7664 = VECTOR ( 'NONE', #23475, 1000.000000000000000 ) ;
#7665 = CARTESIAN_POINT ( 'NONE',  ( -4.000000000000000000, 0.000000000000000000, -43.60000000000000142 ) ) ;
#7666 = VERTEX_POINT ( 'NONE', #25627 ) ;
#7667 = EDGE_LOOP ( 'NONE', ( #28272, #29649, #16088, #26662 ) ) ;
#7668 = FACE_BOUND ( 'NONE', #24588, .T. ) ;
#7669 = CARTESIAN_POINT ( 'NONE',  ( 3.872983346207489852, 0.9999999999999522604, 65.00000000000000000 ) ) ;
#7670 = EDGE_CURVE ( 'NONE', #2498, #27165, #30840, .T. ) ;
#7671 = LINE ( 'NONE', #2476, #28031 ) ;
#7672 = AXIS2_PLACEMENT_3D ( 'NONE', #11835, #27878, #23179 ) ;
#7673 = DIRECTION ( 'NONE',  ( -1.000000000000000000, -0.000000000000000000, 0.000000000000000000 ) ) ;
#7674 = DIRECTION ( 'NONE',  ( 1.000000000000000000, -4.528031003192420052E-15, -1.179290629824070178E-15 ) ) ;
#7675 = CARTESIAN_POINT ( 'NONE',  ( 38.00000000000000000, 6.980486755139912911E-15, 0.000000000000000000 ) ) ;
#7676 = CARTESIAN_POINT ( 'NONE',  ( -36.23083527818513261, -116.0245472910329880, 4.784774454178448266 ) ) ;
#7677 = CARTESIAN_POINT ( 'NONE',  ( -34.50075263804418313, -115.9929510916434481, 12.66759465831979981 ) ) ;
#7678 = CARTESIAN_POINT ( 'NONE',  ( -21.15833593587365513, -35.77980021920998155, 98.97243186433534845 ) ) ;
#7679 = CARTESIAN_POINT ( 'NONE',  ( 0.000000000000000000, 0.000000000000000000, 0.000000000000000000 ) ) ;
#7680 = CARTESIAN_POINT ( 'NONE',  ( 8.000000000000000000, 16.31134495048494060, -6.336799421339643246 ) ) ;
#7681 = CARTESIAN_POINT ( 'NONE',  ( -21.15833593587365513, -24.48076211353301801, 67.99999999999991473 ) ) ;
#7682 = CIRCLE ( 'NONE', #19179, 52.00000000000000711 ) ;
#7683 = DIRECTION ( 'NONE',  ( 0.000000000000000000, 0.000000000000000000, 1.000000000000000000 ) ) ;
#7684 = CARTESIAN_POINT ( 'NONE',  ( 7.999999999999992895, 0.000000000000000000, 0.000000000000000000 ) ) ;
#7685 = ORIENTED_EDGE ( 'NONE', *, *, #2616, .F. ) ;
#7686 = CARTESIAN_POINT ( 'NONE',  ( -37.76916472181486739, -116.0245472910329880, 2.965225545821551290 ) ) ;
#7687 = CARTESIAN_POINT ( 'NONE',  ( 0.000000000000000000, 1.693188892523948885, -15.40623615209870323 ) ) ;
#7688 = EDGE_CURVE ( 'NONE', #540, #1374, #9595, .T. ) ;
#7689 = CARTESIAN_POINT ( 'NONE',  ( 8.000000000000007105, 0.000000000000000000, 0.000000000000000000 ) ) ;
#7690 = ORIENTED_EDGE ( 'NONE', *, *, #35407, .T. ) ;
#7691 = ORIENTED_EDGE ( 'NONE', *, *, #10109, .F. ) ;
#7692 =( NAMED_UNIT ( * ) SI_UNIT ( $, .STERADIAN. ) SOLID_ANGLE_UNIT ( ) );
#7693 = DIRECTION ( 'NONE',  ( 0.000000000000000000, 0.000000000000000000, 1.000000000000000000 ) ) ;
#7694 = EDGE_LOOP ( 'NONE', ( #1040, #26091, #28918, #4176 ) ) ;
#7695 = EDGE_LOOP ( 'NONE', ( #23712, #21767, #29109, #21504 ) ) ;
#7696 = CIRCLE ( 'NONE', #27279, 10.99999999999999822 ) ;
#7697 = EDGE_CURVE ( 'NONE', #30988, #33867, #15331, .T. ) ;
#7698 = PLANE ( 'NONE',  #11967 ) ;
#7699 = EDGE_CURVE ( 'NONE', #26586, #17467, #22369, .T. ) ;
#7700 = CARTESIAN_POINT ( 'NONE',  ( 0.000000000000000000, 0.000000000000000000, 49.10000000000000142 ) ) ;
#7701 = EDGE_CURVE ( 'NONE', #31687, #30036, #27964, .T. ) ;
#7702 = DIRECTION ( 'NONE',  ( -0.000000000000000000, -0.000000000000000000, -1.000000000000000000 ) ) ;
#7703 = DIRECTION ( 'NONE',  ( 0.000000000000000000, 0.4817536741017100499, 0.8763066800438663595 ) ) ;
#7704 = ORIENTED_EDGE ( 'NONE', *, *, #14731, .T. ) ;
#7705 = ORIENTED_EDGE ( 'NONE', *, *, #18288, .F. ) ;
#7706 = CARTESIAN_POINT ( 'NONE',  ( -35.50000000000000711, -112.9415908020655195, 1.873661708251232572 ) ) ;
#7707 = VECTOR ( 'NONE', #16321, 1000.000000000000000 ) ;
#7708 = CIRCLE ( 'NONE', #27847, 10.50000000000000178 ) ;
#7709 = DIRECTION ( 'NONE',  ( 0.000000000000000000, 0.000000000000000000, -1.000000000000000000 ) ) ;
#7710 = EDGE_CURVE ( 'NONE', #15866, #29572, #6178, .T. ) ;
#7711 = DIRECTION ( 'NONE',  ( 1.000000000000000000, -4.524158825347490025E-15, -1.174092375852883357E-15 ) ) ;
#7712 = ORIENTED_EDGE ( 'NONE', *, *, #4182, .F. ) ;
#7713 = CARTESIAN_POINT ( 'NONE',  ( 7.999999999999992895, -35.11945359308084846, -38.34871548466050939 ) ) ;
#7714 = EDGE_CURVE ( 'NONE', #28924, #33336, #16617, .T. ) ;
#7715 = FACE_OUTER_BOUND ( 'NONE', #9130, .T. ) ;
#7716 = CARTESIAN_POINT ( 'NONE',  ( -34.50000000000000000, -114.9927795562974069, 10.48735431211914815 ) ) ;
#7717 = DIRECTION ( 'NONE',  ( -1.000000000000000000, 0.000000000000000000, 0.000000000000000000 ) ) ;
#7718 = CARTESIAN_POINT ( 'NONE',  ( -35.93473953453761283, -114.9929510916434339, 13.11451721564123574 ) ) ;
#7719 = DIRECTION ( 'NONE',  ( 0.000000000000000000, 0.000000000000000000, 1.000000000000000000 ) ) ;
#7720 = CARTESIAN_POINT ( 'NONE',  ( -39.00000000000000000, -113.9929510916434339, 12.53051367006571937 ) ) ;
#7721 = CARTESIAN_POINT ( 'NONE',  ( 8.000000000000000000, -11.19999565274241782, -10.71350075272084545 ) ) ;
#7722 = CARTESIAN_POINT ( 'NONE',  ( 22.99999999999999289, 1.230770033143089817E-14, 0.000000000000000000 ) ) ;
#7723 = CARTESIAN_POINT ( 'NONE',  ( 7.999999999999992895, 0.000000000000000000, 0.000000000000000000 ) ) ;
#7724 = AXIS2_PLACEMENT_3D ( 'NONE', #25632, #25816, #31021 ) ;
#7725 = ORIENTED_EDGE ( 'NONE', *, *, #4265, .F. ) ;
#7726 = DIRECTION ( 'NONE',  ( 1.000000000000000000, 0.000000000000000000, 0.000000000000000000 ) ) ;
#7727 = LINE ( 'NONE', #18710, #6552 ) ;
#7728 = ORIENTED_EDGE ( 'NONE', *, *, #20623, .F. ) ;
#7729 = CARTESIAN_POINT ( 'NONE',  ( -38.00000000000000711, -114.9929510916434339, 12.56351784598954779 ) ) ;
#7730 = ORIENTED_EDGE ( 'NONE', *, *, #24865, .T. ) ;
#7731 = CARTESIAN_POINT ( 'NONE',  ( -39.97545270896702618, -112.6980969099493990, 2.347274454178448710 ) ) ;
#7732 = CARTESIAN_POINT ( 'NONE',  ( -2.000000000000001776, 0.000000000000000000, 0.000000000000000000 ) ) ;
#7733 = EDGE_CURVE ( 'NONE', #22530, #9085, #26280, .T. ) ;
#7734 = ORIENTED_EDGE ( 'NONE', *, *, #32780, .T. ) ;
#7735 = ORIENTED_EDGE ( 'NONE', *, *, #13477, .T. ) ;
#7736 = AXIS2_PLACEMENT_3D ( 'NONE', #30487, #14162, #11295 ) ;
#7737 = DIRECTION ( 'NONE',  ( 1.000000000000000000, 1.734723475976807094E-16, 0.000000000000000000 ) ) ;
#7738 = CIRCLE ( 'NONE', #26754, 20.00000000000000711 ) ;
#7739 = EDGE_CURVE ( 'NONE', #23477, #1430, #30876, .T. ) ;
#7740 = LINE ( 'NONE', #2203, #23211 ) ;
#7741 = EDGE_CURVE ( 'NONE', #31582, #16323, #19918, .T. ) ;
#7742 = VERTEX_POINT ( 'NONE', #768 ) ;
#7743 = CARTESIAN_POINT ( 'NONE',  ( -35.81662171581204746, -117.0245472910329738, 3.284774454178449155 ) ) ;
#7744 = DIRECTION ( 'NONE',  ( 0.000000000000000000, -0.8660254037844329345, -0.5000000000000101030 ) ) ;
#7745 = CARTESIAN_POINT ( 'NONE',  ( 0.000000000000000000, 39.64889472655731595, 33.64468972902522381 ) ) ;
#7746 = VERTEX_POINT ( 'NONE', #25450 ) ;
#7747 = ORIENTED_EDGE ( 'NONE', *, *, #32341, .F. ) ;
#7748 = EDGE_CURVE ( 'NONE', #7835, #20427, #25178, .T. ) ;
#7749 = DIRECTION ( 'NONE',  ( 0.000000000000000000, 0.000000000000000000, 1.000000000000000000 ) ) ;
#7750 = EDGE_CURVE ( 'NONE', #1850, #10066, #30322, .T. ) ;
#7751 = DIRECTION ( 'NONE',  ( 1.000000000000000000, -0.000000000000000000, 0.000000000000000000 ) ) ;
#7753 = EDGE_LOOP ( 'NONE', ( #7179, #6986 ) ) ;
#7752 = CIRCLE ( 'NONE', #302, 6.000000000000005329 ) ;
#7754 = ORIENTED_EDGE ( 'NONE', *, *, #25760, .T. ) ;
#7755 = CARTESIAN_POINT ( 'NONE',  ( -34.50000000000000000, -111.6790780953339066, 2.383953864837686343 ) ) ;
#7756 = CARTESIAN_POINT ( 'NONE',  ( 8.000000000000000000, -3.384281271887945586, 18.48663108841355651 ) ) ;
#7757 = EDGE_LOOP ( 'NONE', ( #34126, #16573 ) ) ;
#7758 = CARTESIAN_POINT ( 'NONE',  ( -35.50000000000000711, -114.1861579685891712, 9.524983039397698192 ) ) ;
#7759 = ADVANCED_FACE ( 'NONE', ( #22192 ), #33193, .T. ) ;
#7760 = AXIS2_PLACEMENT_3D ( 'NONE', #16708, #19064, #11326 ) ;
#7761 = CARTESIAN_POINT ( 'NONE',  ( -38.00000000000000711, -113.9929510916434339, 12.56351784598954779 ) ) ;
#7762 = AXIS2_PLACEMENT_3D ( 'NONE', #34316, #9109, #23315 ) ;
#7763 = CARTESIAN_POINT ( 'NONE',  ( 8.000000000000000000, 15.46619997295642079, 1.007799283846740002 ) ) ;
#7764 = CYLINDRICAL_SURFACE ( 'NONE', #23709, 20.00000000000000355 ) ;
#7765 = CARTESIAN_POINT ( 'NONE',  ( -37.99994980024369085, -113.9929510916434339, 12.62670525340494621 ) ) ;
#7766 = AXIS2_PLACEMENT_3D ( 'NONE', #18324, #26259, #4672 ) ;
#7767 = CARTESIAN_POINT ( 'NONE',  ( -37.99359134332094357, -115.9929510916434481, 12.69998175888958514 ) ) ;
#7768 = CARTESIAN_POINT ( 'NONE',  ( -9.999999999999994671, 0.000000000000000000, 0.000000000000000000 ) ) ;
#7769 = CARTESIAN_POINT ( 'NONE',  ( 0.000000000000000000, 0.000000000000000000, 0.000000000000000000 ) ) ;
#7770 = ORIENTED_EDGE ( 'NONE', *, *, #5964, .F. ) ;
#7771 = CARTESIAN_POINT ( 'NONE',  ( 4.000000000000000000, -13.24207120356975587, 14.98824707027438485 ) ) ;
#7772 = DIRECTION ( 'NONE',  ( 1.000000000000000000, -4.524158825347490025E-15, -1.174092375852883357E-15 ) ) ;
#7773 = DIRECTION ( 'NONE',  ( -0.000000000000000000, 0.000000000000000000, -1.000000000000000000 ) ) ;
#7774 = EDGE_CURVE ( 'NONE', #34245, #27419, #4823, .T. ) ;
#7775 = AXIS2_PLACEMENT_3D ( 'NONE', #7557, #15815, #2192 ) ;
#7776 = ORIENTED_EDGE ( 'NONE', *, *, #10887, .F. ) ;
#7777 = DIRECTION ( 'NONE',  ( 0.000000000000000000, 0.000000000000000000, -1.000000000000000000 ) ) ;
#7778 = ADVANCED_FACE ( 'NONE', ( #26605 ), #12914, .F. ) ;
#7779 = CARTESIAN_POINT ( 'NONE',  ( -35.50000000000000000, -113.0140978167138712, 0.2502176474015764263 ) ) ;
#7780 = DIRECTION ( 'NONE',  ( 0.000000000000000000, 1.000000000000000000, 0.000000000000000000 ) ) ;
#7781 = ADVANCED_FACE ( 'NONE', ( #18120 ), #13109, .T. ) ;
#7782 = CARTESIAN_POINT ( 'NONE',  ( -35.50000000000000711, -114.9925223117477202, 10.47601618151863079 ) ) ;
#7783 = CARTESIAN_POINT ( 'NONE',  ( -4.000000000000000000, 0.000000000000000000, 50.00000000000000000 ) ) ;
#7784 = ORIENTED_EDGE ( 'NONE', *, *, #29774, .F. ) ;
#7785 = FACE_OUTER_BOUND ( 'NONE', #31155, .T. ) ;
#7786 = VECTOR ( 'NONE', #35574, 1000.000000000000000 ) ;
#7787 = CARTESIAN_POINT ( 'NONE',  ( -35.50000000000000000, -111.7850029017436810, -2.224114562373086912 ) ) ;
#7788 = ORIENTED_EDGE ( 'NONE', *, *, #18922, .F. ) ;
#7789 = VERTEX_POINT ( 'NONE', #31996 ) ;
#7790 = ADVANCED_FACE ( 'NONE', ( #34705 ), #29125, .F. ) ;
#7791 = CARTESIAN_POINT ( 'NONE',  ( -35.99999999999999289, -114.0592624029313242, 6.003524454178450043 ) ) ;
#7792 = EDGE_CURVE ( 'NONE', #9366, #2211, #24593, .T. ) ;
#7793 = AXIS2_PLACEMENT_3D ( 'NONE', #25815, #9942, #9406 ) ;
#7794 = AXIS2_PLACEMENT_3D ( 'NONE', #24403, #19162, #33215 ) ;
#7795 = FACE_OUTER_BOUND ( 'NONE', #20220, .T. ) ;
#7796 = ORIENTED_EDGE ( 'NONE', *, *, #34152, .T. ) ;
#7797 = ORIENTED_EDGE ( 'NONE', *, *, #29587, .T. ) ;
#7798 = CARTESIAN_POINT ( 'NONE',  ( -34.50000000000000000, -113.1807644833805426, -0.6247823525984269599 ) ) ;
#7799 = AXIS2_PLACEMENT_3D ( 'NONE', #11209, #20174, #33700 ) ;
#7800 = LINE ( 'NONE', #30132, #22312 ) ;
#7801 = CARTESIAN_POINT ( 'NONE',  ( -1.519999999999992912, 1.359543261233475143E-15, 6.983999999999990216 ) ) ;
#7802 = DIRECTION ( 'NONE',  ( -1.000000000000000000, 0.000000000000000000, 0.000000000000000000 ) ) ;
#7803 = AXIS2_PLACEMENT_3D ( 'NONE', #26250, #12925, #18316 ) ;
#7804 = CARTESIAN_POINT ( 'NONE',  ( -37.99999897736218202, -114.9929510916434339, 12.62466071271732915 ) ) ;
#7805 = FACE_OUTER_BOUND ( 'NONE', #22139, .T. ) ;
#7806 = CARTESIAN_POINT ( 'NONE',  ( 0.6000000000000035305, -12.74999999999999822, -1.200000000000006617 ) ) ;
#7807 = CARTESIAN_POINT ( 'NONE',  ( -34.50000000000000000, -114.9724313160460696, -1.624792769101446765 ) ) ;
#7808 = DIRECTION ( 'NONE',  ( -1.000000000000000000, 0.000000000000000000, -0.000000000000000000 ) ) ;
#7809 = AXIS2_PLACEMENT_3D ( 'NONE', #16045, #26536, #12484 ) ;
#7810 = CARTESIAN_POINT ( 'NONE',  ( 0.000000000000000000, -31.08872492059985859, 41.68322423723089543 ) ) ;
#7811 = VERTEX_POINT ( 'NONE', #7332 ) ;
#7812 = CARTESIAN_POINT ( 'NONE',  ( -35.50000000000000711, -114.1712995509219724, 9.522174004479579068 ) ) ;
#7813 = CARTESIAN_POINT ( 'NONE',  ( 0.000000000000000000, -12.49559743815785140, 9.169462670380546854 ) ) ;
#7814 = PRESENTATION_STYLE_ASSIGNMENT (( #10893 ) ) ;
#7815 = DIRECTION ( 'NONE',  ( 0.000000000000000000, 0.000000000000000000, 1.000000000000000000 ) ) ;
#7816 = VECTOR ( 'NONE', #23457, 1000.000000000000000 ) ;
#7817 = CIRCLE ( 'NONE', #905, 19.99999999999998579 ) ;
#7818 = DIRECTION ( 'NONE',  ( 0.000000000000000000, 0.3420201433256693235, -0.9396926207859082059 ) ) ;
#7819 = VERTEX_POINT ( 'NONE', #26240 ) ;
#7820 = CIRCLE ( 'NONE', #34365, 45.00000000000000000 ) ;
#7821 = CARTESIAN_POINT ( 'NONE',  ( 4.000000000000003553, 18.53613841426789932, 48.58406706613910586 ) ) ;
#7822 = CARTESIAN_POINT ( 'NONE',  ( 7.999999999999992895, -49.65209126885753221, -15.44894276735603356 ) ) ;
#7823 = ADVANCED_FACE ( 'NONE', ( #4474 ), #4654, .T. ) ;
#7824 = DIRECTION ( 'NONE',  ( 1.000000000000000000, 0.000000000000000000, 0.000000000000000000 ) ) ;
#7825 = CARTESIAN_POINT ( 'NONE',  ( 8.000000000000007105, 9.637487275701364098, -10.15474465512039615 ) ) ;
#7826 = VECTOR ( 'NONE', #6542, 1000.000000000000000 ) ;
#7827 = LINE ( 'NONE', #30345, #3776 ) ;
#7828 = CARTESIAN_POINT ( 'NONE',  ( 0.000000000000000000, 14.80634052301623171, -8.177498406287266874 ) ) ;
#7829 = ORIENTED_EDGE ( 'NONE', *, *, #35524, .F. ) ;
#7830 = CIRCLE ( 'NONE', #1516, 44.99999999999999289 ) ;
#7831 = ORIENTED_EDGE ( 'NONE', *, *, #9791, .T. ) ;
#7832 = DIRECTION ( 'NONE',  ( 0.000000000000000000, 0.000000000000000000, 1.000000000000000000 ) ) ;
#7833 = CARTESIAN_POINT ( 'NONE',  ( 8.000000000000000000, 0.000000000000000000, 0.000000000000000000 ) ) ;
#7834 = CARTESIAN_POINT ( 'NONE',  ( -39.49999999999999289, -11.24969279549607748, 111.5585998451919778 ) ) ;
#7835 = VERTEX_POINT ( 'NONE', #1941 ) ;
#7836 = CARTESIAN_POINT ( 'NONE',  ( -36.23083527818512550, -111.9754527089670404, 5.215225545821551734 ) ) ;
#7837 = VERTEX_POINT ( 'NONE', #32175 ) ;
#7838 = VERTEX_POINT ( 'NONE', #21183 ) ;
#7839 = ORIENTED_EDGE ( 'NONE', *, *, #20702, .F. ) ;
#7840 = CARTESIAN_POINT ( 'NONE',  ( -55.00000000000000000, -25.98076211353320275, 84.99999999999994316 ) ) ;
#7841 = VECTOR ( 'NONE', #23421, 1000.000000000000227 ) ;
#7842 = AXIS2_PLACEMENT_3D ( 'NONE', #33497, #19784, #30799 ) ;
#7843 = CIRCLE ( 'NONE', #8993, 45.00000000000000000 ) ;
#7844 = DIRECTION ( 'NONE',  ( -1.000000000000000000, -1.836970198721029934E-16, -0.000000000000000000 ) ) ;
#7845 = VERTEX_POINT ( 'NONE', #7500 ) ;
#7846 = ORIENTED_EDGE ( 'NONE', *, *, #13477, .F. ) ;
#7847 = AXIS2_PLACEMENT_3D ( 'NONE', #13079, #21687, #23875 ) ;
#7848 = CARTESIAN_POINT ( 'NONE',  ( 8.000000000000007105, 0.000000000000000000, 0.000000000000000000 ) ) ;
#7849 = CARTESIAN_POINT ( 'NONE',  ( 8.000000000000000000, 0.000000000000000000, 0.000000000000000000 ) ) ;
#7850 = CARTESIAN_POINT ( 'NONE',  ( 44.00000000000000000, 4.000000000000010658, 4.898587196589409870E-16 ) ) ;
#7851 = AXIS2_PLACEMENT_3D ( 'NONE', #16769, #3293, #27611 ) ;
#7852 = PLANE ( 'NONE',  #33220 ) ;
#7853 = CARTESIAN_POINT ( 'NONE',  ( 7.999999999999992895, 0.000000000000000000, 0.000000000000000000 ) ) ;
#7854 = CARTESIAN_POINT ( 'NONE',  ( -35.02454729103298092, -114.8876895276775087, 4.597274454178448266 ) ) ;
#7855 = CARTESIAN_POINT ( 'NONE',  ( -37.18750000000004974, -115.9929510916434481, 14.11852480586265024 ) ) ;
#7856 = DIRECTION ( 'NONE',  ( 0.000000000000000000, -0.2588190451025151329, -0.9659258262890697555 ) ) ;
#7857 = VECTOR ( 'NONE', #26569, 1000.000000000000000 ) ;
#7858 = DIRECTION ( 'NONE',  ( -1.000000000000000000, -0.000000000000000000, 0.000000000000000000 ) ) ;
#7859 = CIRCLE ( 'NONE', #9592, 17.49900000000001299 ) ;
#7860 = CARTESIAN_POINT ( 'NONE',  ( -21.15833593587365513, -26.68172400785650922, 80.78589838486213637 ) ) ;
#7861 = DIRECTION ( 'NONE',  ( -1.000000000000000000, 0.000000000000000000, 0.000000000000000000 ) ) ;
#7862 = ADVANCED_FACE ( 'NONE', ( #26426 ), #34894, .T. ) ;
#7863 = CIRCLE ( 'NONE', #20495, 9.499000000000000554 ) ;
#7864 = DIRECTION ( 'NONE',  ( -1.000000000000000000, -0.000000000000000000, -0.000000000000000000 ) ) ;
#7865 = DIRECTION ( 'NONE',  ( 0.000000000000000000, 0.000000000000000000, 1.000000000000000000 ) ) ;
#7866 = ORIENTED_EDGE ( 'NONE', *, *, #33945, .T. ) ;
#7867 = CARTESIAN_POINT ( 'NONE',  ( -35.00000000000000000, -113.9407375970686900, 3.996475545821551290 ) ) ;
#7868 = CARTESIAN_POINT ( 'NONE',  ( 0.000000000000000000, 0.000000000000000000, -34.40000000000000568 ) ) ;
#7869 = DIRECTION ( 'NONE',  ( -5.339440136655842133E-16, -1.000000000000000000, 6.938893903907197563E-17 ) ) ;
#7870 = CARTESIAN_POINT ( 'NONE',  ( 0.000000000000000000, -16.71027810728550733, -2.620268201066114688 ) ) ;
#7871 = ORIENTED_EDGE ( 'NONE', *, *, #22097, .F. ) ;
#7872 = CARTESIAN_POINT ( 'NONE',  ( -34.50000000000000000, -113.0140978167156902, -0.6247823525984268489 ) ) ;
#7873 = VERTEX_POINT ( 'NONE', #18483 ) ;
#7874 = VECTOR ( 'NONE', #216, 1000.000000000000227 ) ;
#7875 = DIRECTION ( 'NONE',  ( -0.000000000000000000, 0.000000000000000000, -1.000000000000000000 ) ) ;
#7876 = DIRECTION ( 'NONE',  ( 0.000000000000000000, 0.000000000000000000, 1.000000000000000000 ) ) ;
#7877 = VERTEX_POINT ( 'NONE', #1756 ) ;
#7878 = CIRCLE ( 'NONE', #33203, 11.00000000000001066 ) ;
#7879 =( GEOMETRIC_REPRESENTATION_CONTEXT ( 3 ) GLOBAL_UNCERTAINTY_ASSIGNED_CONTEXT ( ( #243 ) ) GLOBAL_UNIT_ASSIGNED_CONTEXT ( ( #22968, #4630, #23150 ) ) REPRESENTATION_CONTEXT ( 'NONE', 'WORKASPACE' ) );
#7880 = EDGE_CURVE ( 'NONE', #15577, #21509, #32064, .T. ) ;
#7881 = EDGE_LOOP ( 'NONE', ( #20022, #19040 ) ) ;
#7882 = DIRECTION ( 'NONE',  ( -1.000000000000000000, 0.000000000000000000, 0.000000000000000000 ) ) ;
#7883 = CARTESIAN_POINT ( 'NONE',  ( -36.11231047232249836, -115.9754527089670262, 8.777725545821553510 ) ) ;
#7884 = DIRECTION ( 'NONE',  ( 1.000000000000000000, 0.000000000000000000, 0.000000000000000000 ) ) ;
#7885 = LINE ( 'NONE', #16153, #28240 ) ;
#7886 = CIRCLE ( 'NONE', #1577, 3.799999999999999822 ) ;
#7887 = ORIENTED_EDGE ( 'NONE', *, *, #5554, .T. ) ;
#7888 = ORIENTED_EDGE ( 'NONE', *, *, #32019, .F. ) ;
#7889 = CARTESIAN_POINT ( 'NONE',  ( -35.50000000000000711, -112.8835768857893527, -1.616767172155725740 ) ) ;
#7890 = PLANE ( 'NONE',  #19164 ) ;
#7891 = DIRECTION ( 'NONE',  ( -1.000000000000000000, -0.000000000000000000, -0.000000000000000000 ) ) ;
#7892 = ORIENTED_EDGE ( 'NONE', *, *, #17976, .T. ) ;
#7893 = DIRECTION ( 'NONE',  ( 1.000000000000000000, -0.000000000000000000, -0.000000000000000000 ) ) ;
#7894 = VECTOR ( 'NONE', #4821, 1000.000000000000000 ) ;
#7895 = ADVANCED_FACE ( 'NONE', ( #28941 ), #15058, .T. ) ;
#7896 = CIRCLE ( 'NONE', #29205, 3.799999999999999822 ) ;
#7897 = CARTESIAN_POINT ( 'NONE',  ( -34.50000000000000000, -112.8835768857893527, -1.616767172155725740 ) ) ;
#7898 = AXIS2_PLACEMENT_3D ( 'NONE', #15488, #18381, #29382 ) ;
#7899 = CARTESIAN_POINT ( 'NONE',  ( -38.25557080230232998, -114.9929510916434339, 13.92914543265419525 ) ) ;
#7900 = CARTESIAN_POINT ( 'NONE',  ( -90.00000000000002842, 0.000000000000000000, 6.938893903907228378E-15 ) ) ;
#7901 = CARTESIAN_POINT ( 'NONE',  ( -38.00000000000000711, -114.9929510916434339, 12.59652202191340820 ) ) ;
#7902 = DIRECTION ( 'NONE',  ( 1.000000000000000000, -0.000000000000000000, -0.000000000000000000 ) ) ;
#7903 = CARTESIAN_POINT ( 'NONE',  ( -34.50000000000000000, -114.9929510916434339, 10.61627146648203812 ) ) ;
#7904 = CARTESIAN_POINT ( 'NONE',  ( -2.321707774797454604, -4.824281976789094095, -0.7999999999999951594 ) ) ;
#7905 = CIRCLE ( 'NONE', #28046, 22.00000000000000000 ) ;
#7906 = CARTESIAN_POINT ( 'NONE',  ( 5.400000000000085620, -1.000000000000049516, -52.50000000000000000 ) ) ;
#7907 = LINE ( 'NONE', #18891, #16843 ) ;
#7908 = ORIENTED_EDGE ( 'NONE', *, *, #10208, .F. ) ;
#7909 = CYLINDRICAL_SURFACE ( 'NONE', #16426, 20.00000000000000355 ) ;
#7910 = DIRECTION ( 'NONE',  ( -1.000000000000000000, 0.000000000000000000, 0.000000000000000000 ) ) ;
#7911 = EDGE_CURVE ( 'NONE', #22574, #20209, #21352, .T. ) ;
#7912 = VERTEX_POINT ( 'NONE', #6791 ) ;
#7913 = EDGE_CURVE ( 'NONE', #22617, #22087, #5625, .T. ) ;
#7914 = CARTESIAN_POINT ( 'NONE',  ( -36.01562499999996447, -114.9929510916434339, 13.11852480586264669 ) ) ;
#7915 = ORIENTED_EDGE ( 'NONE', *, *, #28625, .T. ) ;
#7916 = CARTESIAN_POINT ( 'NONE',  ( -38.37230871539094323, -112.5438815906447729, 5.441024454178449155 ) ) ;
#7917 = DIRECTION ( 'NONE',  ( -0.000000000000000000, -0.2538061376417690140, -0.9672551082808337197 ) ) ;
#7918 = AXIS2_PLACEMENT_3D ( 'NONE', #16397, #13200, #21811 ) ;
#7919 = EDGE_LOOP ( 'NONE', ( #16845, #26912, #1881, #16569 ) ) ;
#7920 = EDGE_LOOP ( 'NONE', ( #20972, #2333 ) ) ;
#7921 = DIRECTION ( 'NONE',  ( 0.000000000000000000, -1.000000000000000000, 0.000000000000000000 ) ) ;
#7922 = DIRECTION ( 'NONE',  ( 0.000000000000000000, 0.9822872507286879440, 0.1873813145857285423 ) ) ;
#7923 = AXIS2_PLACEMENT_3D ( 'NONE', #9719, #28636, #26473 ) ;
#7924 = ADVANCED_FACE ( 'NONE', ( #26067 ), #4289, .T. ) ;
#7925 = ORIENTED_EDGE ( 'NONE', *, *, #26088, .T. ) ;
#7926 = CARTESIAN_POINT ( 'NONE',  ( -38.37230871539094323, -112.5438815906447729, 8.441024454178448266 ) ) ;
#7927 = AXIS2_PLACEMENT_3D ( 'NONE', #3076, #27903, #14031 ) ;
#7928 = ADVANCED_FACE ( 'NONE', ( #20807 ), #29842, .T. ) ;
#7929 = VECTOR ( 'NONE', #5027, 1000.000000000000000 ) ;
#7930 = CARTESIAN_POINT ( 'NONE',  ( 7.999999999999992895, 35.11945359308111847, 38.34871548466027491 ) ) ;
#7931 = DIRECTION ( 'NONE',  ( -9.266685234918781277E-17, 8.062994716340199375E-15, 1.000000000000000000 ) ) ;
#7932 = VERTEX_POINT ( 'NONE', #13800 ) ;
#7933 = ORIENTED_EDGE ( 'NONE', *, *, #34608, .T. ) ;
#7934 = DIRECTION ( 'NONE',  ( -1.000000000000000000, 0.000000000000000000, 0.000000000000000000 ) ) ;
#7935 = CIRCLE ( 'NONE', #17118, 4.800000000000001599 ) ;
#7936 = DIRECTION ( 'NONE',  ( 0.000000000000000000, 0.000000000000000000, -1.000000000000000000 ) ) ;
#7937 = ORIENTED_EDGE ( 'NONE', *, *, #33983, .F. ) ;
#7938 = ORIENTED_EDGE ( 'NONE', *, *, #6699, .F. ) ;
#7939 = CARTESIAN_POINT ( 'NONE',  ( -34.50000000000000000, -111.0141141789186605, -0.6738694770610589302 ) ) ;
#7940 = DIRECTION ( 'NONE',  ( -1.000000000000000000, 0.000000000000000000, 0.000000000000000000 ) ) ;
#7941 = ORIENTED_EDGE ( 'NONE', *, *, #743, .F. ) ;
#7942 = CARTESIAN_POINT ( 'NONE',  ( -35.50000000000000711, -114.9929510916434339, 10.52826033068511435 ) ) ;
#7943 = ADVANCED_FACE ( 'NONE', ( #16296 ), #19019, .T. ) ;
#7944 = CARTESIAN_POINT ( 'NONE',  ( -34.50000306791346816, -113.9929510916434339, 12.62875129555796150 ) ) ;
#7945 = CARTESIAN_POINT ( 'NONE',  ( -21.15833593587365513, -35.77980021920998155, 98.97243186433534845 ) ) ;
#7946 = AXIS2_PLACEMENT_3D ( 'NONE', #23889, #10204, #21173 ) ;
#7947 = DIRECTION ( 'NONE',  ( -1.000000000000000000, 0.000000000000000000, 0.000000000000000000 ) ) ;
#7948 = CARTESIAN_POINT ( 'NONE',  ( -37.99999897736217491, -113.9929510916434339, 12.62466071271733092 ) ) ;
#7949 = CARTESIAN_POINT ( 'NONE',  ( -36.12500000000014211, -115.9929510916434481, 13.11852480586264846 ) ) ;
#7950 = FACE_OUTER_BOUND ( 'NONE', #22565, .T. ) ;
#7951 = DIRECTION ( 'NONE',  ( 0.000000000000000000, 1.000000000000000000, 9.406921877466749789E-15 ) ) ;
#7952 = EDGE_CURVE ( 'NONE', #14603, #30739, #17682, .T. ) ;
#7953 = ADVANCED_FACE ( 'NONE', ( #4995 ), #32519, .T. ) ;
#7954 = VERTEX_POINT ( 'NONE', #15952 ) ;
#7955 = EDGE_CURVE ( 'NONE', #14767, #532, #24786, .T. ) ;
#7956 = CARTESIAN_POINT ( 'NONE',  ( 0.9999999999999453770, -6.008326913195871199, -0.7999999999999951594 ) ) ;
#7957 = CARTESIAN_POINT ( 'NONE',  ( 3.799999999999999822, -2.710505431213761085E-17, -30.90000000000000568 ) ) ;
#7958 = CIRCLE ( 'NONE', #23484, 2.447112362156711018 ) ;
#7959 = DIRECTION ( 'NONE',  ( 0.000000000000000000, 0.000000000000000000, 1.000000000000000000 ) ) ;
#7960 = ORIENTED_EDGE ( 'NONE', *, *, #34015, .T. ) ;
#7961 = CARTESIAN_POINT ( 'NONE',  ( 0.000000000000000000, 0.000000000000000000, 0.000000000000000000 ) ) ;
#7962 = VERTEX_POINT ( 'NONE', #283 ) ;
#7963 = CARTESIAN_POINT ( 'NONE',  ( -35.50000000000000711, -116.0140978167138712, -0.4997823525984418369 ) ) ;
#7964 = LINE ( 'NONE', #27067, #27663 ) ;
#7965 = CARTESIAN_POINT ( 'NONE',  ( -35.50000000000000711, -114.9927795562974069, 10.48735431211914815 ) ) ;
#7966 = CARTESIAN_POINT ( 'NONE',  ( 7.999999999999992895, -6.109652351742118626, 46.58570277113506819 ) ) ;
#7967 = EDGE_CURVE ( 'NONE', #3021, #15081, #27308, .T. ) ;
#7968 = EDGE_LOOP ( 'NONE', ( #34520, #2771, #11921, #15688 ) ) ;
#7969 = CARTESIAN_POINT ( 'NONE',  ( 65.00000000000001421, -25.98076211353320986, 84.99999999999994316 ) ) ;
#7970 = CARTESIAN_POINT ( 'NONE',  ( -35.50000000000000000, -111.0173113992184710, -0.7556348869410824953 ) ) ;
#7971 = ORIENTED_EDGE ( 'NONE', *, *, #8556, .F. ) ;
#7972 = ORIENTED_EDGE ( 'NONE', *, *, #13407, .F. ) ;
#7973 = CARTESIAN_POINT ( 'NONE',  ( -36.52652403469556930, -113.0245472910329880, 8.722274454178450043 ) ) ;
#7974 = AXIS2_PLACEMENT_3D ( 'NONE', #14647, #24950, #3354 ) ;
#7975 = EDGE_CURVE ( 'NONE', #12363, #22667, #26970, .T. ) ;
#7976 = AXIS2_PLACEMENT_3D ( 'NONE', #13009, #25667, #9442 ) ;
#7977 = DIRECTION ( 'NONE',  ( -1.783119874454246424E-31, -1.187911941725854497E-31, 1.000000000000000000 ) ) ;
#7978 = ORIENTED_EDGE ( 'NONE', *, *, #17902, .F. ) ;
#7979 = ORIENTED_EDGE ( 'NONE', *, *, #9211, .T. ) ;
#7980 = AXIS2_PLACEMENT_3D ( 'NONE', #28486, #25970, #25802 ) ;
#7981 = CARTESIAN_POINT ( 'NONE',  ( -34.50000000000000000, -113.0140978167137717, -0.6411448143358797758 ) ) ;
#7982 = SHAPE_REPRESENTATION ( 'spur gear_iso_ISO - Spur gear 2M 50T 20PA 8FW ---S50A75H50L22.0R1', ( #21307 ), #32275 ) ;
#7983 = DIRECTION ( 'NONE',  ( 0.000000000000000000, 9.406921877466749789E-15, -1.000000000000000000 ) ) ;
#7984 = DIRECTION ( 'NONE',  ( -1.000000000000000000, -1.836970198721029934E-16, -0.000000000000000000 ) ) ;
#7985 = ADVANCED_FACE ( 'NONE', ( #16480, #24256 ), #7852, .T. ) ;
#7986 = CARTESIAN_POINT ( 'NONE',  ( -44.00000000000000000, 0.000000000000000000, 0.000000000000000000 ) ) ;
#7987 = CARTESIAN_POINT ( 'NONE',  ( -37.98402046630260287, -114.9929510916434339, 12.74811950270164118 ) ) ;
#7988 = EDGE_CURVE ( 'NONE', #29170, #2115, #9048, .T. ) ;
#7989 = DIRECTION ( 'NONE',  ( -1.000000000000000000, 0.000000000000000000, 0.000000000000000000 ) ) ;
#7990 = CARTESIAN_POINT ( 'NONE',  ( 7.999999999999992895, -0.6505223195679143977, -51.99593080916758936 ) ) ;
#7991 = CARTESIAN_POINT ( 'NONE',  ( -34.50000000000000000, -112.9486715495423681, -1.623175561345890472 ) ) ;
#7992 = CARTESIAN_POINT ( 'NONE',  ( -34.51922597003733273, -115.9929510916434481, 12.86289566494349224 ) ) ;
#7993 = DIRECTION ( 'NONE',  ( -1.000000000000000000, 0.000000000000000000, 0.000000000000000000 ) ) ;
#7994 = EDGE_CURVE ( 'NONE', #1847, #33885, #29756, .T. ) ;
#7995 = CARTESIAN_POINT ( 'NONE',  ( 0.000000000000000000, -12.46108038583323285, 15.64357617738992801 ) ) ;
#7996 = EDGE_LOOP ( 'NONE', ( #33121, #30769, #32061, #33696 ) ) ;
#7997 = CARTESIAN_POINT ( 'NONE',  ( -35.50000000000000711, -114.0998638248492085, 9.511920366020609308 ) ) ;
#7998 = CARTESIAN_POINT ( 'NONE',  ( 4.000000000000003553, 13.56094713063571078, 50.20060470671747055 ) ) ;
#7999 = DIRECTION ( 'NONE',  ( 0.000000000000000000, 0.000000000000000000, 1.000000000000000000 ) ) ;
#8000 = EDGE_CURVE ( 'NONE', #25742, #28491, #13111, .T. ) ;
#8001 = DIRECTION ( 'NONE',  ( -1.000000000000000000, 0.000000000000000000, 0.000000000000000000 ) ) ;
#8002 = DIRECTION ( 'NONE',  ( 0.000000000000000000, -0.8660254037844385966, -0.5000000000000001110 ) ) ;
#8003 = ORIENTED_EDGE ( 'NONE', *, *, #14371, .F. ) ;
#8004 = PLANE ( 'NONE',  #29158 ) ;
#8005 = DIRECTION ( 'NONE',  ( 1.000000000000000000, 0.000000000000000000, 0.000000000000000000 ) ) ;
#8006 = FACE_OUTER_BOUND ( 'NONE', #15206, .T. ) ;
#8007 = DIRECTION ( 'NONE',  ( -1.000000000000000000, 0.000000000000000000, 0.000000000000000000 ) ) ;
#8008 = AXIS2_PLACEMENT_3D ( 'NONE', #14237, #33678, #9013 ) ;
#8009 = FACE_OUTER_BOUND ( 'NONE', #27018, .T. ) ;
#8010 = DIRECTION ( 'NONE',  ( -1.000000000000000000, 0.000000000000000000, 0.000000000000000000 ) ) ;
#8011 = ORIENTED_EDGE ( 'NONE', *, *, #10778, .T. ) ;
#8012 = ORIENTED_EDGE ( 'NONE', *, *, #7362, .T. ) ;
#8013 = CARTESIAN_POINT ( 'NONE',  ( -42.49999999999999289, -25.98076211353322051, 84.99999999999992895 ) ) ;
#8014 = CARTESIAN_POINT ( 'NONE',  ( 7.999999999999992895, -44.61570720899084819, -14.73072383765613935 ) ) ;
#8015 = LINE ( 'NONE', #20969, #34667 ) ;
#8016 = VERTEX_POINT ( 'NONE', #2312 ) ;
#8017 = CARTESIAN_POINT ( 'NONE',  ( -36.11231047232249125, -115.9754527089670262, 7.277725545821551734 ) ) ;
#8018 = ORIENTED_EDGE ( 'NONE', *, *, #21518, .F. ) ;
#8019 =( NAMED_UNIT ( * ) SI_UNIT ( $, .STERADIAN. ) SOLID_ANGLE_UNIT ( ) );
#8020 = ORIENTED_EDGE ( 'NONE', *, *, #20272, .F. ) ;
#8021 = VERTEX_POINT ( 'NONE', #13969 ) ;
#8022 = DIRECTION ( 'NONE',  ( 0.000000000000000000, 0.000000000000000000, -1.000000000000000000 ) ) ;
#8023 = APPLICATION_CONTEXT ( 'automotive_design' ) ;
#8024 = VECTOR ( 'NONE', #27137, 1000.000000000000000 ) ;
#8025 = EDGE_CURVE ( 'NONE', #10671, #27661, #1581, .T. ) ;
#8026 = CARTESIAN_POINT ( 'NONE',  ( 0.000000000000000000, 0.000000000000000000, 49.10000000000000142 ) ) ;
#8027 = EDGE_LOOP ( 'NONE', ( #23701, #29739, #6628, #19444 ) ) ;
#8028 = ORIENTED_EDGE ( 'NONE', *, *, #11988, .F. ) ;
#8029 = VECTOR ( 'NONE', #3403, 1000.000000000000000 ) ;
#8030 = EDGE_CURVE ( 'NONE', #13101, #26981, #5184, .T. ) ;
#8031 = CARTESIAN_POINT ( 'NONE',  ( 8.000000000000000000, 0.000000000000000000, 0.000000000000000000 ) ) ;
#8032 = CARTESIAN_POINT ( 'NONE',  ( -34.50000000000001421, -16.18172400785637777, 71.02756813566458050 ) ) ;
#8033 = CIRCLE ( 'NONE', #1151, 19.99999999999998579 ) ;
#8034 = EDGE_CURVE ( 'NONE', #27440, #30478, #8104, .T. ) ;
#8035 = DIRECTION ( 'NONE',  ( 0.000000000000000000, 0.000000000000000000, -1.000000000000000000 ) ) ;
#8036 = CIRCLE ( 'NONE', #28754, 47.49900000000001654 ) ;
#8037 = CARTESIAN_POINT ( 'NONE',  ( -1.799999999999996048, 0.000000000000000000, 0.000000000000000000 ) ) ;
#8038 = CARTESIAN_POINT ( 'NONE',  ( 7.999999999999992895, 0.000000000000000000, 0.000000000000000000 ) ) ;
#8039 = DIRECTION ( 'NONE',  ( 0.000000000000000000, -0.7705132427757949154, 0.6374239897486828621 ) ) ;
#8040 = CARTESIAN_POINT ( 'NONE',  ( -38.92341863475394348, -115.9929510916434481, 13.10177712753322155 ) ) ;
#8041 = FACE_OUTER_BOUND ( 'NONE', #10730, .T. ) ;
#8042 = PLANE ( 'NONE',  #28773 ) ;
#8043 = CARTESIAN_POINT ( 'NONE',  ( -34.49999999999998579, -12.31102132296306451, 91.73752798680880005 ) ) ;
#8044 = CYLINDRICAL_SURFACE ( 'NONE', #31922, 3.799999999999999822 ) ;
#8045 = CYLINDRICAL_SURFACE ( 'NONE', #22235, 6.765000000000044977 ) ;
#8046 = ORIENTED_EDGE ( 'NONE', *, *, #21473, .T. ) ;
#8047 = EDGE_CURVE ( 'NONE', #11561, #19855, #21893, .T. ) ;
#8048 = CARTESIAN_POINT ( 'NONE',  ( -34.97545270896703329, -114.7691647218148745, 2.590225545821551734 ) ) ;
#8049 = CARTESIAN_POINT ( 'NONE',  ( 8.000000000000000000, 16.71027810728552154, -2.620268201066000113 ) ) ;
#8050 = DIRECTION ( 'NONE',  ( 0.000000000000000000, 0.000000000000000000, 1.000000000000000000 ) ) ;
#8051 = DIRECTION ( 'NONE',  ( 1.000000000000000000, -5.339440136655842133E-16, 1.047965281155515476E-16 ) ) ;
#8052 = ORIENTED_EDGE ( 'NONE', *, *, #33644, .T. ) ;
#8053 = VECTOR ( 'NONE', #24481, 1000.000000000000000 ) ;
#8054 = VERTEX_POINT ( 'NONE', #11269 ) ;
#8055 = CARTESIAN_POINT ( 'NONE',  ( 0.000000000000000000, 0.000000000000000000, 0.000000000000000000 ) ) ;
#8056 = VERTEX_POINT ( 'NONE', #22071 ) ;
#8057 = VERTEX_POINT ( 'NONE', #27498 ) ;
#8058 = CIRCLE ( 'NONE', #7490, 10.50000000000000178 ) ;
#8059 = AXIS2_PLACEMENT_3D ( 'NONE', #14029, #17562, #25026 ) ;
#8060 = DIRECTION ( 'NONE',  ( -1.734723475976807094E-16, 1.000000000000000000, 0.000000000000000000 ) ) ;
#8061 = CARTESIAN_POINT ( 'NONE',  ( 8.000000000000000000, 0.000000000000000000, 0.000000000000000000 ) ) ;
#8062 = PRODUCT_CONTEXT ( 'NONE', #12385, 'mechanical' ) ;
#8063 = CYLINDRICAL_SURFACE ( 'NONE', #27127, 10.99999999999999289 ) ;
#8064 = ORIENTED_EDGE ( 'NONE', *, *, #32592, .T. ) ;
#8065 = EDGE_LOOP ( 'NONE', ( #4448, #10738 ) ) ;
#8066 = EDGE_CURVE ( 'NONE', #29366, #1167, #19401, .T. ) ;
#8067 = DIRECTION ( 'NONE',  ( 1.000000000000000000, -0.000000000000000000, 0.000000000000000000 ) ) ;
#8068 = DIRECTION ( 'NONE',  ( 0.000000000000000000, -0.9659258262890689783, 0.2588190451025185190 ) ) ;
#8069 = ORIENTED_EDGE ( 'NONE', *, *, #28275, .T. ) ;
#8070 = CARTESIAN_POINT ( 'NONE',  ( 115.0000000000000000, 81.48267994499606459, 30.15054357219658954 ) ) ;
#8071 = VECTOR ( 'NONE', #17588, 1000.000000000000000 ) ;
#8072 = CARTESIAN_POINT ( 'NONE',  ( -34.50000000000000000, -112.0140978167138712, -0.3747823525984256832 ) ) ;
#8073 = CARTESIAN_POINT ( 'NONE',  ( -37.52454134262690388, -114.9929510916434339, 14.11837420659362152 ) ) ;
#8074 = LINE ( 'NONE', #35463, #29789 ) ;
#8075 = CARTESIAN_POINT ( 'NONE',  ( -35.50000000000000000, -113.9929510916434339, 10.50625754673588474 ) ) ;
#8076 = CARTESIAN_POINT ( 'NONE',  ( 50.00000000000000000, -59.99999999999997158, -25.00000000000000000 ) ) ;
#8077 = EDGE_CURVE ( 'NONE', #10012, #20656, #19361, .T. ) ;
#8078 = VECTOR ( 'NONE', #34498, 1000.000000000000114 ) ;
#8079 = CARTESIAN_POINT ( 'NONE',  ( -34.50000000000000000, -114.9929510916434339, 12.26648026267477221 ) ) ;
#8080 = DIRECTION ( 'NONE',  ( 1.000000000000000000, -0.000000000000000000, -0.000000000000000000 ) ) ;
#8081 = CARTESIAN_POINT ( 'NONE',  ( 0.000000000000000000, 0.000000000000000000, 60.90000000000001279 ) ) ;
#8082 = DIRECTION ( 'NONE',  ( -1.000000000000000000, 0.000000000000000000, 0.000000000000000000 ) ) ;
#8083 = DIRECTION ( 'NONE',  ( 0.000000000000000000, 0.000000000000000000, 1.000000000000000000 ) ) ;
#8084 = DIRECTION ( 'NONE',  ( 0.000000000000000000, 0.000000000000000000, -1.000000000000000000 ) ) ;
#8085 = CARTESIAN_POINT ( 'NONE',  ( 8.000000000000000000, -14.71414642875948608, -9.471478019455300768 ) ) ;
#8086 = ORIENTED_EDGE ( 'NONE', *, *, #19839, .T. ) ;
#8087 = CARTESIAN_POINT ( 'NONE',  ( -34.49999999999998579, -24.48076211353304643, 71.08058909292488181 ) ) ;
#8088 = ORIENTED_EDGE ( 'NONE', *, *, #31543, .T. ) ;
#8089 = CARTESIAN_POINT ( 'NONE',  ( -34.02454729103298092, -115.3019030900506294, 1.597274454178448932 ) ) ;
#8090 = DIRECTION ( 'NONE',  ( 0.000000000000000000, 0.8443279255020164076, -0.5358267949789946583 ) ) ;
#8091 = ORIENTED_EDGE ( 'NONE', *, *, #12062, .T. ) ;
#8092 = VERTEX_POINT ( 'NONE', #33576 ) ;
#8093 = FACE_OUTER_BOUND ( 'NONE', #21092, .T. ) ;
#8094 = CARTESIAN_POINT ( 'NONE',  ( 0.000000000000000000, 0.000000000000000000, 0.000000000000000000 ) ) ;
#8095 = CIRCLE ( 'NONE', #12711, 4.000000000000003553 ) ;
#8096 = EDGE_LOOP ( 'NONE', ( #29389, #28425, #12580, #34605 ) ) ;
#8097 = CARTESIAN_POINT ( 'NONE',  ( -33.97545270896702618, -112.8166217158120475, 7.409774454178449155 ) ) ;
#8098 = FACE_OUTER_BOUND ( 'NONE', #17463, .T. ) ;
#8099 = DIRECTION ( 'NONE',  ( -1.000000000000000000, 0.000000000000000000, 0.000000000000000000 ) ) ;
#8100 = ORIENTED_EDGE ( 'NONE', *, *, #3412, .T. ) ;
#8101 = ORIENTED_EDGE ( 'NONE', *, *, #10457, .T. ) ;
#8102 = CARTESIAN_POINT ( 'NONE',  ( 0.000000000000000000, -47.00885577955408223, -6.806061952192771436 ) ) ;
#8103 = AXIS2_PLACEMENT_3D ( 'NONE', #11198, #22170, #15875 ) ;
#8104 = CIRCLE ( 'NONE', #28803, 22.00000000000000000 ) ;
#8105 = AXIS2_PLACEMENT_3D ( 'NONE', #183, #8466, #27741 ) ;
#8106 = DIRECTION ( 'NONE',  ( 0.000000000000000000, 0.000000000000000000, 1.000000000000000000 ) ) ;
#8107 = ORIENTED_EDGE ( 'NONE', *, *, #25788, .T. ) ;
#8108 = ORIENTED_EDGE ( 'NONE', *, *, #3550, .F. ) ;
#8109 = CARTESIAN_POINT ( 'NONE',  ( -34.50000000000000000, -111.0140978167138570, -0.1247823525984260717 ) ) ;
#8110 = EDGE_CURVE ( 'NONE', #31137, #10989, #22413, .T. ) ;
#8111 = EDGE_CURVE ( 'NONE', #12890, #18651, #9959, .T. ) ;
#8112 = DIRECTION ( 'NONE',  ( 0.000000000000000000, 0.000000000000000000, 1.000000000000000000 ) ) ;
#8113 = EDGE_LOOP ( 'NONE', ( #28621, #12995, #16890, #23449 ) ) ;
#8114 = CARTESIAN_POINT ( 'NONE',  ( -35.50000000000000711, -114.9929517792218689, 10.50900788599415314 ) ) ;
#8115 = CARTESIAN_POINT ( 'NONE',  ( -34.50000000000000000, -113.9929510916434339, 10.85830208992344303 ) ) ;
#8116 = LINE ( 'NONE', #7945, #23499 ) ;
#8117 = AXIS2_PLACEMENT_3D ( 'NONE', #1942, #26241, #4290 ) ;
#8118 = DIRECTION ( 'NONE',  ( 1.000000000000000000, 0.000000000000000000, 0.000000000000000000 ) ) ;
#8119 = EDGE_CURVE ( 'NONE', #4873, #33119, #6759, .T. ) ;
#8120 = CARTESIAN_POINT ( 'NONE',  ( -34.50000000000000000, -113.9929510916434339, 11.91443571948720148 ) ) ;
#8121 = CYLINDRICAL_SURFACE ( 'NONE', #34381, 22.00000000000000000 ) ;
#8122 = CARTESIAN_POINT ( 'NONE',  ( -38.00000000000000711, -115.9929510916434481, 12.39849696637031151 ) ) ;
#8123 = DIRECTION ( 'NONE',  ( -1.000000000000000000, 0.000000000000000000, 0.000000000000000000 ) ) ;
#8124 = CARTESIAN_POINT ( 'NONE',  ( 0.000000000000000000, 15.92965478239641008, -15.17386234660366284 ) ) ;
#8125 = ORIENTED_EDGE ( 'NONE', *, *, #34786, .T. ) ;
#8126 = VECTOR ( 'NONE', #28828, 1000.000000000000000 ) ;
#8127 = COLOUR_RGB ( '', 0.31764706, 0.68627451, 0.89019608) ;
#8128 = CARTESIAN_POINT ( 'NONE',  ( 8.000000000000007105, -9.433698091065103597, 1.111908866155073117 ) ) ;
#8129 = DIRECTION ( 'NONE',  ( -0.000000000000000000, 0.000000000000000000, -1.000000000000000000 ) ) ;
#8130 = AXIS2_PLACEMENT_3D ( 'NONE', #18110, #26595, #4815 ) ;
#8131 = LINE ( 'NONE', #2048, #26651 ) ;
#8132 = VERTEX_POINT ( 'NONE', #8482 ) ;
#8133 = LINE ( 'NONE', #30110, #384 ) ;
#8134 = ORIENTED_EDGE ( 'NONE', *, *, #32143, .F. ) ;
#8135 = CARTESIAN_POINT ( 'NONE',  ( -35.50000000000000000, -113.3822401464312719, 0.9191614010536472978 ) ) ;
#8136 = DIRECTION ( 'NONE',  ( 0.1305261922200512403, -0.9914448613738104932, 6.326001338775677127E-32 ) ) ;
#8137 = CARTESIAN_POINT ( 'NONE',  ( -35.97545270896702618, -113.6450488405582604, 4.409774454178449155 ) ) ;
#8138 = CARTESIAN_POINT ( 'NONE',  ( -35.50000000000000711, -114.9929510916434339, 10.61627146648203812 ) ) ;
#8139 = FACE_OUTER_BOUND ( 'NONE', #13605, .T. ) ;
#8140 = EDGE_CURVE ( 'NONE', #11039, #21916, #30349, .T. ) ;
#8141 = VERTEX_POINT ( 'NONE', #8651 ) ;
#8142 = CARTESIAN_POINT ( 'NONE',  ( -35.50000000000000000, -111.0141129414446652, 0.9205922128478062350 ) ) ;
#8143 = ORIENTED_EDGE ( 'NONE', *, *, #29104, .T. ) ;
#8144 = EDGE_LOOP ( 'NONE', ( #30816, #21870, #34875, #29555 ) ) ;
#8145 = CARTESIAN_POINT ( 'NONE',  ( -38.45611840935523418, -115.3723087153909432, 3.566024454178448710 ) ) ;
#8146 = LINE ( 'NONE', #15891, #9494 ) ;
#8147 = VERTEX_POINT ( 'NONE', #19618 ) ;
#8148 = VERTEX_POINT ( 'NONE', #30280 ) ;
#8149 = CARTESIAN_POINT ( 'NONE',  ( -34.50000000000000000, -115.0140978167138712, -0.6247823525983134951 ) ) ;
#8150 = CARTESIAN_POINT ( 'NONE',  ( 7.999999999999992895, -32.00046193115173310, 34.40241257139674502 ) ) ;
#8151 = EDGE_CURVE ( 'NONE', #128, #29395, #35031, .T. ) ;
#8152 = EDGE_CURVE ( 'NONE', #5415, #27865, #5957, .T. ) ;
#8153 = EDGE_CURVE ( 'NONE', #4619, #17814, #10219, .T. ) ;
#8154 = VECTOR ( 'NONE', #21438, 1000.000000000000000 ) ;
#8155 = AXIS2_PLACEMENT_3D ( 'NONE', #12361, #9667, #20624 ) ;
#8156 = DIRECTION ( 'NONE',  ( -1.000000000000000000, 0.000000000000000000, -0.000000000000000000 ) ) ;
#8157 = FACE_OUTER_BOUND ( 'NONE', #27335, .T. ) ;
#8158 = CARTESIAN_POINT ( 'NONE',  ( -35.50000000000000000, -113.9929510916435618, 10.50625754673588474 ) ) ;
#8159 = CARTESIAN_POINT ( 'NONE',  ( -2.321707774797454604, -4.824281976789094095, -0.7999999999999951594 ) ) ;
#8160 = CARTESIAN_POINT ( 'NONE',  ( 0.000000000000000000, 0.000000000000000000, 0.000000000000000000 ) ) ;
#8161 = ADVANCED_FACE ( 'NONE', ( #5438 ), #14802, .T. ) ;
#8162 = CARTESIAN_POINT ( 'NONE',  ( -34.50000000000000000, -114.1807644833817648, -1.624782352598427959 ) ) ;
#8163 = EDGE_CURVE ( 'NONE', #19841, #26766, #2081, .T. ) ;
#8164 = CARTESIAN_POINT ( 'NONE',  ( -37.52454134262689678, -115.9929510916434481, 14.11837420659362152 ) ) ;
#8165 = DIRECTION ( 'NONE',  ( 0.000000000000000000, 0.000000000000000000, -1.000000000000000000 ) ) ;
#8166 = VECTOR ( 'NONE', #22378, 1000.000000000000000 ) ;
#8167 = CARTESIAN_POINT ( 'NONE',  ( 7.999999999999992895, -13.85708833600001277, 45.43276465116660745 ) ) ;
#8168 = ORIENTED_EDGE ( 'NONE', *, *, #25979, .F. ) ;
#8169 = CARTESIAN_POINT ( 'NONE',  ( -37.89983305244309264, -115.9929510916434481, 12.92579853460519423 ) ) ;
#8170 = CYLINDRICAL_SURFACE ( 'NONE', #16517, 20.00000000000000355 ) ;
#8171 = DIRECTION ( 'NONE',  ( 0.000000000000000000, 0.000000000000000000, 1.000000000000000000 ) ) ;
#8172 = CARTESIAN_POINT ( 'NONE',  ( 0.000000000000000000, -19.74581912682808493, -48.10512059033414545 ) ) ;
#8173 = CARTESIAN_POINT ( 'NONE',  ( 7.999999999999992895, 40.47821179127715396, 32.64221760512774040 ) ) ;
#8174 = ORIENTED_EDGE ( 'NONE', *, *, #11371, .F. ) ;
#8175 = DIRECTION ( 'NONE',  ( 0.000000000000000000, -0.8443279255020087470, -0.5358267949790064266 ) ) ;
#8176 = FACE_OUTER_BOUND ( 'NONE', #18389, .T. ) ;
#8177 = AXIS2_PLACEMENT_3D ( 'NONE', #34987, #13718, #10308 ) ;
#8178 = CARTESIAN_POINT ( 'NONE',  ( 0.000000000000000000, 16.31134495048485178, 6.336799421339877725 ) ) ;
#8179 = DIRECTION ( 'NONE',  ( 0.000000000000000000, 0.000000000000000000, 1.000000000000000000 ) ) ;
#8180 = CIRCLE ( 'NONE', #7589, 3.799999999999999822 ) ;
#8181 = DIRECTION ( 'NONE',  ( 1.000000000000000000, -0.000000000000000000, 0.000000000000000000 ) ) ;
#8182 = FACE_OUTER_BOUND ( 'NONE', #12820, .T. ) ;
#8183 = ADVANCED_FACE ( 'NONE', ( #32800 ), #8121, .T. ) ;
#8184 = ORIENTED_EDGE ( 'NONE', *, *, #23202, .T. ) ;
#8185 = ORIENTED_EDGE ( 'NONE', *, *, #8641, .F. ) ;
#8186 = SHAPE_REPRESENTATION ( 'spur gear_iso_ISO - Spur gear 2M 20T 20PA 8FW ---S20A75H50L8.0S1', ( #21307 ), #30547 ) ;
#8187 = CARTESIAN_POINT ( 'NONE',  ( 70.00000000000001421, -30.47068043442695284, 93.33026027086508236 ) ) ;
#8188 = DIRECTION ( 'NONE',  ( 0.000000000000000000, 0.000000000000000000, 1.000000000000000000 ) ) ;
#8189 = EDGE_CURVE ( 'NONE', #11629, #10719, #32562, .T. ) ;
#8190 = FACE_OUTER_BOUND ( 'NONE', #29567, .T. ) ;
#8191 = ORIENTED_EDGE ( 'NONE', *, *, #19560, .T. ) ;
#8192 = CARTESIAN_POINT ( 'NONE',  ( -38.45611840935523418, -112.6276912846090568, 6.433975545821550845 ) ) ;
#8193 = ORIENTED_EDGE ( 'NONE', *, *, #9856, .F. ) ;
#8194 = EDGE_CURVE ( 'NONE', #32016, #14718, #1443, .T. ) ;
#8195 = ITEM_DEFINED_TRANSFORMATION ( 'NONE', 'NONE', #33400,  #21307 ) ;
#8197 = ORIENTED_EDGE ( 'NONE', *, *, #5932, .T. ) ;
#8196 = VECTOR ( 'NONE', #28328, 1000.000000000000000 ) ;
#8198 = ORIENTED_EDGE ( 'NONE', *, *, #759, .T. ) ;
#8199 = CARTESIAN_POINT ( 'NONE',  ( 0.000000000000000000, -2.710505431213761085E-17, 55.00000000000000000 ) ) ;
#8200 = EDGE_CURVE ( 'NONE', #30516, #15107, #10814, .T. ) ;
#8201 = ADVANCED_FACE ( 'NONE', ( #28106 ), #3625, .F. ) ;
#8202 = CYLINDRICAL_SURFACE ( 'NONE', #5871, 3.799999999999999822 ) ;
#8203 = VERTEX_POINT ( 'NONE', #6309 ) ;
#8204 = AXIS2_PLACEMENT_3D ( 'NONE', #16443, #35381, #11067 ) ;
#8205 = CARTESIAN_POINT ( 'NONE',  ( -35.50000000000000711, -114.9929510916434339, 10.51725893871048889 ) ) ;
#8206 = CIRCLE ( 'NONE', #3619, 4.000000000000000000 ) ;
#8207 = CARTESIAN_POINT ( 'NONE',  ( 8.000000000000000000, -16.71027810728550733, 4.579731798933884157 ) ) ;
#8208 = DIRECTION ( 'NONE',  ( -1.000000000000000000, -0.000000000000000000, -0.000000000000000000 ) ) ;
#8209 = ADVANCED_FACE ( 'NONE', ( #25941 ), #12066, .T. ) ;
#8210 = CARTESIAN_POINT ( 'NONE',  ( -2.000000000000001776, 4.724999999999993427, 0.000000000000000000 ) ) ;
#8211 = LINE ( 'NONE', #19189, #14522 ) ;
#8212 = CARTESIAN_POINT ( 'NONE',  ( 3.872983346207517386, -1.000000000000028644, 55.00000000000000711 ) ) ;
#8213 = CARTESIAN_POINT ( 'NONE',  ( -37.43749999999998579, -115.9929510916434481, 14.11852480586265024 ) ) ;
#8214 = CARTESIAN_POINT ( 'NONE',  ( 0.000000000000000000, -2.710505431213761085E-17, 45.99999999999998579 ) ) ;
#8215 = CARTESIAN_POINT ( 'NONE',  ( 0.000000000000000000, 0.000000000000000000, -55.00000000000000000 ) ) ;
#8216 = CIRCLE ( 'NONE', #21990, 14.70000000000000107 ) ;
#8217 = DIRECTION ( 'NONE',  ( 0.000000000000000000, 0.000000000000000000, -1.000000000000000000 ) ) ;
#8218 = DIRECTION ( 'NONE',  ( 0.000000000000000000, -6.245004513516508695E-15, -1.000000000000000000 ) ) ;
#8219 = CIRCLE ( 'NONE', #32956, 2.999999999999999112 ) ;
#8220 = CARTESIAN_POINT ( 'NONE',  ( -46.00000000000000000, -25.98076211353320275, 73.99999999999992895 ) ) ;
#8221 = ORIENTED_EDGE ( 'NONE', *, *, #8194, .F. ) ;
#8222 = CARTESIAN_POINT ( 'NONE',  ( -37.88768952767750875, -112.0245472910329880, 8.027725545821549957 ) ) ;
#8223 = DIRECTION ( 'NONE',  ( -1.000000000000000000, -1.836970198721029934E-16, -0.000000000000000000 ) ) ;
#8224 = LINE ( 'NONE', #27514, #1524 ) ;
#8225 = DIRECTION ( 'NONE',  ( -0.000000000000000000, 0.000000000000000000, -1.000000000000000000 ) ) ;
#8226 = EDGE_CURVE ( 'NONE', #14995, #4091, #902, .T. ) ;
#8227 = ORIENTED_EDGE ( 'NONE', *, *, #22056, .T. ) ;
#8228 = ORIENTED_EDGE ( 'NONE', *, *, #29602, .F. ) ;
#8229 = EDGE_CURVE ( 'NONE', #4771, #35305, #5565, .T. ) ;
#8230 = DIRECTION ( 'NONE',  ( 1.000000000000000000, 0.000000000000000000, 0.000000000000000000 ) ) ;
#8231 = AXIS2_PLACEMENT_3D ( 'NONE', #20104, #34354, #28769 ) ;
#8232 = DIRECTION ( 'NONE',  ( 0.000000000000000000, -0.8660254037844327124, -0.5000000000000104361 ) ) ;
#8233 = ORIENTED_EDGE ( 'NONE', *, *, #11682, .T. ) ;
#8234 = ORIENTED_EDGE ( 'NONE', *, *, #24865, .F. ) ;
#8235 = CARTESIAN_POINT ( 'NONE',  ( 8.000000000000000000, 5.482169781018835231, 16.00140663693125376 ) ) ;
#8236 = DIRECTION ( 'NONE',  ( -1.000000000000000000, 0.000000000000000000, 0.000000000000000000 ) ) ;
#8237 = ADVANCED_FACE ( 'NONE', ( #11884 ), #20684, .F. ) ;
#8238 = EDGE_CURVE ( 'NONE', #9311, #33836, #23039, .T. ) ;
#8239 = DIRECTION ( 'NONE',  ( 1.367164536213226704E-17, -0.6749244146946962175, 0.7378868710371677686 ) ) ;
#8240 = DIRECTION ( 'NONE',  ( 1.000000000000000000, -0.000000000000000000, -0.000000000000000000 ) ) ;
#8241 = ORIENTED_EDGE ( 'NONE', *, *, #29513, .F. ) ;
#8242 = ORIENTED_EDGE ( 'NONE', *, *, #24674, .T. ) ;
#8243 = AXIS2_PLACEMENT_3D ( 'NONE', #28057, #22448, #11479 ) ;
#8244 = DIRECTION ( 'NONE',  ( 0.000000000000000000, -0.8660254037844432595, 0.4999999999999920619 ) ) ;
#8245 = CARTESIAN_POINT ( 'NONE',  ( -34.49999999999998579, -37.28532556477447457, 93.25874355921401104 ) ) ;
#8246 = ORIENTED_EDGE ( 'NONE', *, *, #33739, .F. ) ;
#8247 = DIRECTION ( 'NONE',  ( 0.000000000000000000, -0.3090169943749546677, 0.9510565162951511997 ) ) ;
#8248 = CARTESIAN_POINT ( 'NONE',  ( -34.50000000000000000, -112.0141059978162019, -0.6575071456984691309 ) ) ;
#8249 = CARTESIAN_POINT ( 'NONE',  ( -38.98077402996267438, -114.9929510916434339, 12.86289566494346204 ) ) ;
#8250 = AXIS2_PLACEMENT_3D ( 'NONE', #20231, #11983, #17361 ) ;
#8251 = CARTESIAN_POINT ( 'NONE',  ( -35.50000000000000000, -113.9929510916434339, 10.50625754673609258 ) ) ;
#8252 = DIRECTION ( 'NONE',  ( 1.000000000000000000, 0.000000000000000000, 0.000000000000000000 ) ) ;
#8253 = CARTESIAN_POINT ( 'NONE',  ( -34.80050084267117683, -114.9929510916434339, 13.54034599209289169 ) ) ;
#8254 = CARTESIAN_POINT ( 'NONE',  ( 0.000000000000000000, 0.000000000000000000, 0.000000000000000000 ) ) ;
#8255 = CARTESIAN_POINT ( 'NONE',  ( -1.000000000000014655, -4.808326913196006913, 0.000000000000000000 ) ) ;
#8256 = LINE ( 'NONE', #9452, #23092 ) ;
#8257 = CARTESIAN_POINT ( 'NONE',  ( 0.000000000000000000, 0.000000000000000000, 65.00000000000000000 ) ) ;
#8258 = DIRECTION ( 'NONE',  ( -1.174092375852890260E-15, 4.222049128630259891E-16, 1.000000000000000000 ) ) ;
#8259 = LINE ( 'NONE', #16882, #26706 ) ;
#8260 = AXIS2_PLACEMENT_3D ( 'NONE', #3392, #5724, #10953 ) ;
#8261 = ORIENTED_EDGE ( 'NONE', *, *, #15867, .F. ) ;
#8262 = CARTESIAN_POINT ( 'NONE',  ( -3.799999999999999822, 4.382607293638566128E-16, 45.10000000000000142 ) ) ;
#8263 = ORIENTED_EDGE ( 'NONE', *, *, #31691, .T. ) ;
#8264 = CARTESIAN_POINT ( 'NONE',  ( -36.94073759706866156, -111.0000000000000284, 4.128524454178449155 ) ) ;
#8265 = PLANE ( 'NONE',  #1428 ) ;
#8266 = ORIENTED_EDGE ( 'NONE', *, *, #16639, .F. ) ;
#8267 = CIRCLE ( 'NONE', #32415, 20.00000000000000711 ) ;
#8268 = ORIENTED_EDGE ( 'NONE', *, *, #31688, .T. ) ;
#8269 = EDGE_CURVE ( 'NONE', #31708, #22574, #3255, .T. ) ;
#8270 = CYLINDRICAL_SURFACE ( 'NONE', #10261, 20.00000000000000711 ) ;
#8271 = LINE ( 'NONE', #32417, #10577 ) ;
#8272 = ORIENTED_EDGE ( 'NONE', *, *, #13218, .F. ) ;
#8273 = CARTESIAN_POINT ( 'NONE',  ( -35.69809690994941320, -116.9754527089670546, 4.277725545821552622 ) ) ;
#8274 = DIRECTION ( 'NONE',  ( -1.000000000000000000, 0.000000000000000000, 0.000000000000000000 ) ) ;
#8275 = CIRCLE ( 'NONE', #10006, 3.799999999999999822 ) ;
#8276 = DIRECTION ( 'NONE',  ( 0.000000000000000000, -0.2588190451025342842, 0.9659258262890646485 ) ) ;
#8277 = AXIS2_PLACEMENT_3D ( 'NONE', #25412, #2614, #3629 ) ;
#8278 = VERTEX_POINT ( 'NONE', #12423 ) ;
#8279 = ORIENTED_EDGE ( 'NONE', *, *, #6699, .T. ) ;
#8280 = CARTESIAN_POINT ( 'NONE',  ( -34.49999999999998579, -3.784235812937200460, 96.08311962715481513 ) ) ;
#8281 = CARTESIAN_POINT ( 'NONE',  ( 4.000000000000003553, 19.35373470438998211, -10.46102064772319729 ) ) ;
#8282 = ORIENTED_EDGE ( 'NONE', *, *, #19989, .T. ) ;
#8283 = VERTEX_POINT ( 'NONE', #14401 ) ;
#8284 = CARTESIAN_POINT ( 'NONE',  ( -34.50000000000000000, -115.6584342456100671, -2.522673865603758614 ) ) ;
#8285 = DIRECTION ( 'NONE',  ( -1.000000000000000000, 0.000000000000000000, 0.000000000000000000 ) ) ;
#8286 = ORIENTED_EDGE ( 'NONE', *, *, #18141, .F. ) ;
#8287 = CARTESIAN_POINT ( 'NONE',  ( -36.01562499999996447, -114.9929510916434339, 13.11852480586264669 ) ) ;
#8288 = CARTESIAN_POINT ( 'NONE',  ( -34.50075263804418313, -113.9929510916434339, 12.66759465831979981 ) ) ;
#8289 = CARTESIAN_POINT ( 'NONE',  ( 4.000000000000003553, 12.30077720129095553, 50.52416135122086871 ) ) ;
#8290 = CARTESIAN_POINT ( 'NONE',  ( 7.999999999999992895, 0.000000000000000000, 0.000000000000000000 ) ) ;
#8291 = CARTESIAN_POINT ( 'NONE',  ( -34.50000000000000000, -113.9929510916434339, 10.50625754673587409 ) ) ;
#8292 = CARTESIAN_POINT ( 'NONE',  ( 4.000000000000003553, 5.871425383722286284, -51.66745943012276854 ) ) ;
#8293 = CARTESIAN_POINT ( 'NONE',  ( -35.50000000000000711, -114.9929510916434339, 10.51725893871048889 ) ) ;
#8294 = DIRECTION ( 'NONE',  ( 1.000000000000000000, 0.000000000000000000, 0.000000000000000000 ) ) ;
#8296 = AXIS2_PLACEMENT_3D ( 'NONE', #14332, #8580, #3554 ) ;
#8295 = DIRECTION ( 'NONE',  ( 0.000000000000000000, 0.000000000000000000, -1.000000000000000000 ) ) ;
#8297 = EDGE_LOOP ( 'NONE', ( #2862, #573, #20752, #12298 ) ) ;
#8298 = ORIENTED_EDGE ( 'NONE', *, *, #21808, .F. ) ;
#8299 = CARTESIAN_POINT ( 'NONE',  ( -3.799999999999999822, 4.653657836759942730E-16, -44.50000000000000000 ) ) ;
#8300 = FACE_OUTER_BOUND ( 'NONE', #27249, .T. ) ;
#8301 = CIRCLE ( 'NONE', #21526, 20.00000000000000711 ) ;
#8302 = ORIENTED_EDGE ( 'NONE', *, *, #17452, .T. ) ;
#8303 = CARTESIAN_POINT ( 'NONE',  ( 8.000000000000000000, -16.31134495048480559, -6.336799421339987859 ) ) ;
#8304 = ORIENTED_EDGE ( 'NONE', *, *, #12355, .F. ) ;
#8305 = EDGE_CURVE ( 'NONE', #19752, #16680, #31517, .T. ) ;
#8306 = CARTESIAN_POINT ( 'NONE',  ( -35.50000000000000000, -113.0140978167138712, 0.0002176474015660057743 ) ) ;
#8307 = PLANE ( 'NONE',  #8103 ) ;
#8308 = CARTESIAN_POINT ( 'NONE',  ( -37.97545270896701908, -113.5265240346955977, 2.347274454178448710 ) ) ;
#8309 = DIRECTION ( 'NONE',  ( -1.000000000000000000, 0.000000000000000000, 0.000000000000000000 ) ) ;
#8310 = VERTEX_POINT ( 'NONE', #31680 ) ;
#8311 = CARTESIAN_POINT ( 'NONE',  ( 0.000000000000000000, 6.071532165918824830E-15, 1.000000000000000000 ) ) ;
#8312 = CARTESIAN_POINT ( 'NONE',  ( -35.50000000000000711, -112.0577668799241309, 1.173706424699810569 ) ) ;
#8313 = ORIENTED_EDGE ( 'NONE', *, *, #31545, .F. ) ;
#8314 = EDGE_LOOP ( 'NONE', ( #5168, #3251 ) ) ;
#8315 = CARTESIAN_POINT ( 'NONE',  ( -36.23083527818512550, -116.0245472910329880, 4.784774454178448266 ) ) ;
#8316 = EDGE_CURVE ( 'NONE', #17379, #21593, #10159, .T. ) ;
#8317 =( LENGTH_UNIT ( ) NAMED_UNIT ( * ) SI_UNIT ( .MILLI., .METRE. ) );
#8318 = CARTESIAN_POINT ( 'NONE',  ( 0.9999999999999453770, -6.008326913195871199, -0.7999999999999951594 ) ) ;
#8319 = EDGE_LOOP ( 'NONE', ( #8356, #14772, #14837, #5605 ) ) ;
#8320 = ORIENTED_EDGE ( 'NONE', *, *, #17121, .T. ) ;
#8321 = EDGE_CURVE ( 'NONE', #31925, #29341, #30291, .T. ) ;
#8322 = CARTESIAN_POINT ( 'NONE',  ( -34.50000000000000000, -115.0140978167138712, -0.6247823525984403936 ) ) ;
#8323 = DIRECTION ( 'NONE',  ( 0.000000000000000000, 0.000000000000000000, 1.000000000000000000 ) ) ;
#8324 = CLOSED_SHELL ( 'NONE', ( #1799, #15420, #31769, #33982, #29528, #14528, #24619, #31935, #27603, #13865, #31230, #20887, #16427, #13702, #19364, #14350, #11423, #21763, #22242, #21858, #23404, #20012, #23630, #5790, #7131, #26916, #4196, #31512, #26336, #33474, #31847, #24639, #16961, #11526, #22695, #12314, #19457, #30116, #26209, #5130, #14091, #1830, #5995, #6038, #13669, #22633, #34345, #23850, #10438, #19451, #2933, #3731, #11647, #14987, #2969, #7053, #16765, #18335, #3998, #104, #23820 ) ) ;
#8325 = CIRCLE ( 'NONE', #10054, 14.00000000000000000 ) ;
#8326 = DIRECTION ( 'NONE',  ( -1.000000000000000000, 0.000000000000000000, 0.000000000000000000 ) ) ;
#8327 = AXIS2_PLACEMENT_3D ( 'NONE', #35430, #16498, #11460 ) ;
#8328 = DIRECTION ( 'NONE',  ( 0.000000000000000000, 0.000000000000000000, -1.000000000000000000 ) ) ;
#8329 = AXIS2_PLACEMENT_3D ( 'NONE', #29422, #4596, #6420 ) ;
#8330 = CARTESIAN_POINT ( 'NONE',  ( -35.50000000000000000, -113.9929510916434339, 12.59652202191340464 ) ) ;
#8331 = DIRECTION ( 'NONE',  ( -1.000000000000000000, 0.000000000000000000, 0.000000000000000000 ) ) ;
#8332 = CARTESIAN_POINT ( 'NONE',  ( -2.321707774797454604, -4.824281976789094095, -0.7999999999999951594 ) ) ;
#8333 = CARTESIAN_POINT ( 'NONE',  ( -34.50000000000000000, -111.0140978167138570, -0.4685323525984296800 ) ) ;
#8334 = ADVANCED_FACE ( 'NONE', ( #11704 ), #9002, .T. ) ;
#8335 = CARTESIAN_POINT ( 'NONE',  ( -38.99984940073100148, -115.9929510916434481, 12.64306614848957544 ) ) ;
#8336 = DIRECTION ( 'NONE',  ( 0.000000000000000000, 0.9848077530122073542, 0.1736481776669338839 ) ) ;
#8337 = LINE ( 'NONE', #27804, #31249 ) ;
#8338 = CYLINDRICAL_SURFACE ( 'NONE', #800, 20.00000000000000711 ) ;
#8339 = ORIENTED_EDGE ( 'NONE', *, *, #35310, .F. ) ;
#8340 = CARTESIAN_POINT ( 'NONE',  ( -37.93687354226506869, -115.9929510916434481, 12.87038173996323565 ) ) ;
#8341 = CARTESIAN_POINT ( 'NONE',  ( 0.000000000000000000, 19.74581912682842244, 48.10512059033400334 ) ) ;
#8342 = SURFACE_SIDE_STYLE ('',( #24753 ) ) ;
#8343 = DIRECTION ( 'NONE',  ( 0.000000000000000000, -0.2588190451025194072, -0.9659258262890686453 ) ) ;
#8344 = DIRECTION ( 'NONE',  ( 0.000000000000000000, 0.000000000000000000, 1.000000000000000000 ) ) ;
#8345 = EDGE_LOOP ( 'NONE', ( #23372, #22145, #34646, #17959 ) ) ;
#8346 = DIRECTION ( 'NONE',  ( 0.000000000000000000, 0.000000000000000000, -1.000000000000000000 ) ) ;
#8347 = CARTESIAN_POINT ( 'NONE',  ( 0.000000000000000000, -2.710505431213761085E-17, -55.00000000000000000 ) ) ;
#8348 = EDGE_CURVE ( 'NONE', #9156, #19278, #15104, .T. ) ;
#8349 = DIRECTION ( 'NONE',  ( 1.000000000000000000, -0.000000000000000000, -0.000000000000000000 ) ) ;
#8350 = DIRECTION ( 'NONE',  ( 0.000000000000000000, 0.000000000000000000, 1.000000000000000000 ) ) ;
#8351 = EDGE_CURVE ( 'NONE', #5217, #15608, #9723, .T. ) ;
#8352 = EDGE_CURVE ( 'NONE', #8849, #29301, #22787, .T. ) ;
#8353 = CARTESIAN_POINT ( 'NONE',  ( 0.000000000000000000, -5.871425383721907920, 51.66745943012281117 ) ) ;
#8354 = CARTESIAN_POINT ( 'NONE',  ( -3.413765605486555721, -14.29811891091961584, 0.000000000000000000 ) ) ;
#8355 = CIRCLE ( 'NONE', #22156, 2.999999999999988898 ) ;
#8356 = ORIENTED_EDGE ( 'NONE', *, *, #24674, .F. ) ;
#8357 = DIRECTION ( 'NONE',  ( -1.000000000000000000, -0.000000000000000000, -0.000000000000000000 ) ) ;
#8358 = DIRECTION ( 'NONE',  ( -1.000000000000000000, 0.000000000000000000, 0.000000000000000000 ) ) ;
#8359 = CARTESIAN_POINT ( 'NONE',  ( 7.999999999999992895, 47.00885577955413908, 6.806061952192451692 ) ) ;
#8360 = EDGE_LOOP ( 'NONE', ( #16899, #29006, #18947, #21415 ) ) ;
#8361 = CARTESIAN_POINT ( 'NONE',  ( -35.99999999999999289, -113.9407375970686758, 2.496475545821551290 ) ) ;
#8362 = EDGE_CURVE ( 'NONE', #35474, #31629, #12526, .T. ) ;
#8363 = ORIENTED_EDGE ( 'NONE', *, *, #13737, .F. ) ;
#8364 = EDGE_CURVE ( 'NONE', #17651, #15054, #34577, .T. ) ;
#8365 = SURFACE_SIDE_STYLE ('',( #100 ) ) ;
#8366 = CIRCLE ( 'NONE', #29644, 3.799999999999999822 ) ;
#8367 = ORIENTED_EDGE ( 'NONE', *, *, #714, .F. ) ;
#8368 = ORIENTED_EDGE ( 'NONE', *, *, #31705, .F. ) ;
#8369 = PLANE ( 'NONE',  #3965 ) ;
#8370 = CARTESIAN_POINT ( 'NONE',  ( 0.000000000000000000, 0.000000000000000000, 60.00000000000000000 ) ) ;
#8371 = AXIS2_PLACEMENT_3D ( 'NONE', #4218, #3503, #1318 ) ;
#8372 = CARTESIAN_POINT ( 'NONE',  ( -35.50000000000000711, -114.1091535596544873, 9.513028657562415447 ) ) ;
#8373 = DIRECTION ( 'NONE',  ( -1.000000000000000000, -0.000000000000000000, 0.000000000000000000 ) ) ;
#8374 = DIRECTION ( 'NONE',  ( -0.000000000000000000, 0.000000000000000000, -1.000000000000000000 ) ) ;
#8375 = AXIS2_PLACEMENT_3D ( 'NONE', #30144, #5480, #16434 ) ;
#8376 = ADVANCED_FACE ( 'NONE', ( #24307 ), #1988, .T. ) ;
#8377 = AXIS2_PLACEMENT_3D ( 'NONE', #31480, #34007, #28420 ) ;
#8378 = DIRECTION ( 'NONE',  ( 0.000000000000000000, -0.9510565162951565288, 0.3090169943749384029 ) ) ;
#8379 = FACE_OUTER_BOUND ( 'NONE', #34810, .T. ) ;
#8380 = VECTOR ( 'NONE', #3913, 1000.000000000000000 ) ;
#8381 = CIRCLE ( 'NONE', #824, 7.800000000000051337 ) ;
#8382 = PRODUCT_DEFINITION ( 'UNKNOWN', '', #32202, #61 ) ;
#8383 = CARTESIAN_POINT ( 'NONE',  ( 0.000000000000000000, -39.78933988720095982, -24.98727647985043987 ) ) ;
#8384 = CARTESIAN_POINT ( 'NONE',  ( -39.00000000000000000, -115.9929510916434481, 12.60752341388803721 ) ) ;
#8385 = CARTESIAN_POINT ( 'NONE',  ( -44.00000000000000000, 0.000000000000000000, 0.000000000000000000 ) ) ;
#8386 = CIRCLE ( 'NONE', #11275, 20.00000000000000711 ) ;
#8387 = CARTESIAN_POINT ( 'NONE',  ( 115.0000000000000000, 81.48267994499606459, 22.65054357219660019 ) ) ;
#8388 = AXIS2_PLACEMENT_3D ( 'NONE', #23362, #15424, #32005 ) ;
#8389 = CARTESIAN_POINT ( 'NONE',  ( 0.000000000000000000, 0.000000000000000000, 0.000000000000000000 ) ) ;
#8390 = LINE ( 'NONE', #3373, #34819 ) ;
#8391 = ADVANCED_FACE ( 'NONE', ( #4531 ), #12965, .T. ) ;
#8392 = FACE_OUTER_BOUND ( 'NONE', #34971, .T. ) ;
#8393 = SURFACE_STYLE_FILL_AREA ( #9859 ) ;
#8394 = ORIENTED_EDGE ( 'NONE', *, *, #8882, .T. ) ;
#8395 = ADVANCED_FACE ( 'NONE', ( #9892 ), #34947, .T. ) ;
#8396 = EDGE_CURVE ( 'NONE', #23042, #14072, #29134, .T. ) ;
#8397 = CARTESIAN_POINT ( 'NONE',  ( -39.02454729103295961, -113.2308352781851539, 6.340225545821550845 ) ) ;
#8398 = CARTESIAN_POINT ( 'NONE',  ( 0.000000000000000000, 25.61928775981107265, -45.25098998563451147 ) ) ;
#8399 = FACE_OUTER_BOUND ( 'NONE', #24805, .T. ) ;
#8400 = CARTESIAN_POINT ( 'NONE',  ( 8.000000000000007105, 3.268936481846368203, -13.61301047812914256 ) ) ;
#8401 = EDGE_LOOP ( 'NONE', ( #19385, #30084, #29604, #9343 ) ) ;
#8402 = ORIENTED_EDGE ( 'NONE', *, *, #11892, .F. ) ;
#8404 = DIRECTION ( 'NONE',  ( 0.000000000000000000, -1.000000000000000000, 0.000000000000000000 ) ) ;
#8403 = PRODUCT_DEFINITION_SHAPE ( 'NONE', 'NONE',  #35642 ) ;
#8405 = CIRCLE ( 'NONE', #19317, 47.49900000000001654 ) ;
#8406 = DIRECTION ( 'NONE',  ( -1.000000000000000000, 0.000000000000000000, 0.000000000000000000 ) ) ;
#8407 = EDGE_LOOP ( 'NONE', ( #20741, #3838, #26322, #9175 ) ) ;
#8408 = ORIENTED_EDGE ( 'NONE', *, *, #15624, .T. ) ;
#8409 = VECTOR ( 'NONE', #8123, 1000.000000000000000 ) ;
#8410 = CIRCLE ( 'NONE', #29145, 3.799999999999999822 ) ;
#8411 = EDGE_CURVE ( 'NONE', #16728, #9474, #29788, .T. ) ;
#8412 = CIRCLE ( 'NONE', #9579, 20.00000000000000711 ) ;
#8413 = DIRECTION ( 'NONE',  ( 0.000000000000000000, 0.000000000000000000, 1.000000000000000000 ) ) ;
#8414 = DIRECTION ( 'NONE',  ( -1.000000000000000000, -1.734723475976807094E-16, 0.000000000000000000 ) ) ;
#8415 = CIRCLE ( 'NONE', #3840, 4.000000000000000000 ) ;
#8416 = DIRECTION ( 'NONE',  ( 1.000000000000000000, -0.000000000000000000, -0.000000000000000000 ) ) ;
#8418 = ORIENTED_EDGE ( 'NONE', *, *, #9445, .F. ) ;
#8417 = CIRCLE ( 'NONE', #17014, 8.000000000000003553 ) ;
#8419 = ORIENTED_EDGE ( 'NONE', *, *, #877, .T. ) ;
#8420 = CARTESIAN_POINT ( 'NONE',  ( 7.999999999999992895, 0.000000000000000000, 0.000000000000000000 ) ) ;
#8421 = CARTESIAN_POINT ( 'NONE',  ( -49.99999999999999289, -26.99999999999999645, 113.9999999999999858 ) ) ;
#8422 = ORIENTED_EDGE ( 'NONE', *, *, #25928, .F. ) ;
#8423 = CARTESIAN_POINT ( 'NONE',  ( 0.000000000000000000, 0.000000000000000000, 55.00000000000000000 ) ) ;
#8424 = ADVANCED_FACE ( 'NONE', ( #13326 ), #10616, .T. ) ;
#8425 = AXIS2_PLACEMENT_3D ( 'NONE', #15592, #1947, #5001 ) ;
#8426 = CARTESIAN_POINT ( 'NONE',  ( -34.50000000000000000, -115.1446187476384040, -1.616767172155725740 ) ) ;
#8427 = ADVANCED_FACE ( 'NONE', ( #21573 ), #15812, .T. ) ;
#8428 = CARTESIAN_POINT ( 'NONE',  ( -36.07812499999994316, -114.9929510916434339, 14.11852480586264846 ) ) ;
#8429 = VECTOR ( 'NONE', #4545, 1000.000000000000000 ) ;
#8430 = EDGE_CURVE ( 'NONE', #13072, #6142, #26658, .T. ) ;
#8431 = CARTESIAN_POINT ( 'NONE',  ( -35.50000000000000000, -113.9743717753924699, 10.50403980422039396 ) ) ;
#8432 = DIRECTION ( 'NONE',  ( 0.000000000000000000, 0.000000000000000000, 1.000000000000000000 ) ) ;
#8433 = CARTESIAN_POINT ( 'NONE',  ( -36.06250000000002132, -114.9929510916434339, 14.11852480586264846 ) ) ;
#8434 = DIRECTION ( 'NONE',  ( 0.02857142857142376188, 0.9995917534020517525, 3.884870526907702485E-16 ) ) ;
#8435 = ORIENTED_EDGE ( 'NONE', *, *, #4246, .T. ) ;
#8436 = AXIS2_PLACEMENT_3D ( 'NONE', #33251, #8570, #5877 ) ;
#8437 = DIRECTION ( 'NONE',  ( 0.000000000000000000, 0.000000000000000000, 1.000000000000000000 ) ) ;
#8438 = VERTEX_POINT ( 'NONE', #2187 ) ;
#8439 = VECTOR ( 'NONE', #24541, 1000.000000000000000 ) ;
#8440 = CARTESIAN_POINT ( 'NONE',  ( 7.999999999999992895, 0.000000000000000000, 0.000000000000000000 ) ) ;
#8441 = CARTESIAN_POINT ( 'NONE',  ( 7.999999999999992895, 17.08890430202750110, 43.76671000081951490 ) ) ;
#8442 = ORIENTED_EDGE ( 'NONE', *, *, #11324, .T. ) ;
#8443 = FACE_OUTER_BOUND ( 'NONE', #17658, .T. ) ;
#8444 = ORIENTED_EDGE ( 'NONE', *, *, #12646, .T. ) ;
#8445 = EDGE_CURVE ( 'NONE', #29017, #29018, #13156, .T. ) ;
#8446 = CARTESIAN_POINT ( 'NONE',  ( -33.97545270896702618, -112.8166217158120475, 2.909774454178449155 ) ) ;
#8447 = EDGE_CURVE ( 'NONE', #11290, #7845, #18357, .T. ) ;
#8448 = CIRCLE ( 'NONE', #25705, 4.000000000000000000 ) ;
#8449 = DIRECTION ( 'NONE',  ( 0.000000000000000000, 0.000000000000000000, 1.000000000000000000 ) ) ;
#8450 = CARTESIAN_POINT ( 'NONE',  ( -35.50000000000000711, -115.8137639216009234, -1.239329810084483841 ) ) ;
#8451 = CIRCLE ( 'NONE', #19360, 12.55910585664918422 ) ;
#8452 = EDGE_LOOP ( 'NONE', ( #1959, #4903, #28912, #5813 ) ) ;
#8453 = EDGE_LOOP ( 'NONE', ( #17555, #18112, #6736, #22714 ) ) ;
#8454 = DIRECTION ( 'NONE',  ( 0.000000000000000000, 0.000000000000000000, 1.000000000000000000 ) ) ;
#8455 = DIRECTION ( 'NONE',  ( -1.734723475976806848E-16, -0.5000000000000032196, 0.8660254037844368202 ) ) ;
#8456 = ORIENTED_EDGE ( 'NONE', *, *, #7552, .T. ) ;
#8457 = AXIS2_PLACEMENT_3D ( 'NONE', #13974, #13804, #16302 ) ;
#8458 = DIRECTION ( 'NONE',  ( 0.000000000000000000, -0.9848077530122096857, 0.1736481776669208665 ) ) ;
#8459 = AXIS2_PLACEMENT_3D ( 'NONE', #35199, #10697, #13758 ) ;
#8460 = FACE_OUTER_BOUND ( 'NONE', #20580, .T. ) ;
#8461 = ORIENTED_EDGE ( 'NONE', *, *, #16484, .F. ) ;
#8462 = VERTEX_POINT ( 'NONE', #7721 ) ;
#8463 = CARTESIAN_POINT ( 'NONE',  ( 3.799999999999999822, 0.000000000000000000, 60.00000000000000000 ) ) ;
#8464 = AXIS2_PLACEMENT_3D ( 'NONE', #21684, #24760, #19159 ) ;
#8465 = FILL_AREA_STYLE ('',( #24856 ) ) ;
#8466 = DIRECTION ( 'NONE',  ( 1.000000000000000000, -5.339440136655842133E-16, -1.047965281155519420E-16 ) ) ;
#8467 = ORIENTED_EDGE ( 'NONE', *, *, #269, .T. ) ;
#8468 = ORIENTED_EDGE ( 'NONE', *, *, #16956, .T. ) ;
#8469 = CARTESIAN_POINT ( 'NONE',  ( -34.50000000000000000, -117.0140978167138854, 0.6252176474015650465 ) ) ;
#8470 = AXIS2_PLACEMENT_3D ( 'NONE', #17303, #1119, #6686 ) ;
#8471 = CIRCLE ( 'NONE', #25134, 14.00000000000000000 ) ;
#8472 = CARTESIAN_POINT ( 'NONE',  ( 8.000000000000000000, 0.000000000000000000, 0.000000000000000000 ) ) ;
#8473 = ORIENTED_EDGE ( 'NONE', *, *, #12415, .T. ) ;
#8474 = AXIS2_PLACEMENT_3D ( 'NONE', #22220, #14292, #11248 ) ;
#8475 = CARTESIAN_POINT ( 'NONE',  ( -35.50000000000000711, -114.9929510916434339, 12.59102132592610523 ) ) ;
#8476 = EDGE_CURVE ( 'NONE', #10703, #14470, #23452, .T. ) ;
#8477 = ADVANCED_FACE ( 'NONE', ( #1632 ), #29360, .T. ) ;
#8478 = CARTESIAN_POINT ( 'NONE',  ( -34.50000000000000000, -113.9929510916434339, 10.94631322572069365 ) ) ;
#8479 = CYLINDRICAL_SURFACE ( 'NONE', #16605, 4.000000000000000000 ) ;
#8480 = PLANE ( 'NONE',  #30618 ) ;
#8481 = CARTESIAN_POINT ( 'NONE',  ( -34.50000000000000000, -113.9929510916434339, 10.56126450660895699 ) ) ;
#8482 = CARTESIAN_POINT ( 'NONE',  ( 1.599999999999990763, -3.455569164145799535E-16, -4.980000000000017302 ) ) ;
#8483 = CARTESIAN_POINT ( 'NONE',  ( -35.50000000000000711, -114.1068310684433129, 9.512752019463897923 ) ) ;
#8484 = VECTOR ( 'NONE', #27415, 1000.000000000000000 ) ;
#8485 = FACE_OUTER_BOUND ( 'NONE', #5298, .T. ) ;
#8486 = DIRECTION ( 'NONE',  ( -1.000000000000000000, 0.000000000000000000, 0.000000000000000000 ) ) ;
#8487 = AXIS2_PLACEMENT_3D ( 'NONE', #19782, #30795, #24047 ) ;
#8488 = EDGE_LOOP ( 'NONE', ( #22300, #14641, #7734, #30352 ) ) ;
#8489 = ORIENTED_EDGE ( 'NONE', *, *, #25488, .F. ) ;
#8490 = CARTESIAN_POINT ( 'NONE',  ( -10.00000000000000000, 0.000000000000000000, 0.000000000000000000 ) ) ;
#8491 = DIRECTION ( 'NONE',  ( -1.000000000000000000, 0.000000000000000000, 0.000000000000000000 ) ) ;
#8492 = AXIS2_PLACEMENT_3D ( 'NONE', #29840, #5181, #16120 ) ;
#8493 = CIRCLE ( 'NONE', #32069, 7.199999999999986855 ) ;
#8494 = ORIENTED_EDGE ( 'NONE', *, *, #33317, .F. ) ;
#8495 = AXIS2_PLACEMENT_3D ( 'NONE', #2509, #8414, #30396 ) ;
#8496 = DIRECTION ( 'NONE',  ( 0.000000000000000000, -0.9510565162951500895, -0.3090169943749581649 ) ) ;
#8497 = ORIENTED_EDGE ( 'NONE', *, *, #27350, .T. ) ;
#8498 = APPLICATION_CONTEXT ( 'automotive_design' ) ;
#8499 = CARTESIAN_POINT ( 'NONE',  ( -35.50000000000000711, -115.6286452741999113, -1.424448457485488095 ) ) ;
#8500 = DIRECTION ( 'NONE',  ( 0.000000000000000000, 0.000000000000000000, 1.000000000000000000 ) ) ;
#8501 = CARTESIAN_POINT ( 'NONE',  ( -37.05926240293131713, -115.9999999999999858, 1.878524454178448710 ) ) ;
#8502 = AXIS2_PLACEMENT_3D ( 'NONE', #1, #10987, #21951 ) ;
#8503 = CARTESIAN_POINT ( 'NONE',  ( 0.000000000000000000, -2.710505431213761085E-17, 45.10000000000000142 ) ) ;
#8504 = ORIENTED_EDGE ( 'NONE', *, *, #24020, .F. ) ;
#8505 =( NAMED_UNIT ( * ) SI_UNIT ( $, .STERADIAN. ) SOLID_ANGLE_UNIT ( ) );
#8506 = CARTESIAN_POINT ( 'NONE',  ( -35.50000000000000000, -116.9501796819249222, -1.143161139954000260 ) ) ;
#8507 = VERTEX_POINT ( 'NONE', #23586 ) ;
#8508 = ORIENTED_EDGE ( 'NONE', *, *, #2944, .F. ) ;
#8509 = CARTESIAN_POINT ( 'NONE',  ( -35.54388159064475872, -112.6276912846090568, 8.816024454178448266 ) ) ;
#8510 = FACE_OUTER_BOUND ( 'NONE', #22264, .T. ) ;
#8511 = ORIENTED_EDGE ( 'NONE', *, *, #12960, .F. ) ;
#8512 = ORIENTED_EDGE ( 'NONE', *, *, #188, .T. ) ;
#8513 = CARTESIAN_POINT ( 'NONE',  ( -34.50000000000000000, -112.0154707866092707, 0.9357013553229778235 ) ) ;
#8514 = DIRECTION ( 'NONE',  ( 0.000000000000000000, 0.000000000000000000, -1.000000000000000000 ) ) ;
#8515 = CARTESIAN_POINT ( 'NONE',  ( 3.799999999999999822, 4.653657836759942730E-16, -49.10000000000000142 ) ) ;
#8516 = CIRCLE ( 'NONE', #29821, 20.00000000000001066 ) ;
#8517 = EDGE_CURVE ( 'NONE', #17838, #7584, #10446, .T. ) ;
#8518 = CARTESIAN_POINT ( 'NONE',  ( -35.50000000000000000, -113.9929510916434339, 10.52000928670414126 ) ) ;
#8519 = CARTESIAN_POINT ( 'NONE',  ( 3.872983346207416133, 1.000000000000001110, 38.00000000000000000 ) ) ;
#8520 = DIRECTION ( 'NONE',  ( 0.000000000000000000, -1.000000000000000000, 0.000000000000000000 ) ) ;
#8521 = AXIS2_PLACEMENT_3D ( 'NONE', #31086, #28213, #8404 ) ;
#8522 = CARTESIAN_POINT ( 'NONE',  ( -34.50000000000000000, -112.3070160848889429, 2.749963775944984867 ) ) ;
#8523 = CARTESIAN_POINT ( 'NONE',  ( -35.50000000000000000, -114.1556834383649459, 8.511484393387789282 ) ) ;
#8524 = CARTESIAN_POINT ( 'NONE',  ( -9.999999999999994671, 0.000000000000000000, 0.000000000000000000 ) ) ;
#8525 = CARTESIAN_POINT ( 'NONE',  ( 7.999999999999992895, 0.000000000000000000, 0.000000000000000000 ) ) ;
#8526 = ORIENTED_EDGE ( 'NONE', *, *, #546, .T. ) ;
#8527 = ADVANCED_FACE ( 'NONE', ( #31860 ), #5052, .T. ) ;
#8528 = FACE_OUTER_BOUND ( 'NONE', #27433, .T. ) ;
#8529 = DIRECTION ( 'NONE',  ( -1.000000000000000000, 0.000000000000000000, 0.000000000000000000 ) ) ;
#8530 = LINE ( 'NONE', #6012, #30066 ) ;
#8531 = ORIENTED_EDGE ( 'NONE', *, *, #20685, .T. ) ;
#8532 = CARTESIAN_POINT ( 'NONE',  ( -39.49999999999999289, -12.00833024919777081, 94.79903810567661537 ) ) ;
#8533 = DIRECTION ( 'NONE',  ( 0.000000000000000000, 0.000000000000000000, -1.000000000000000000 ) ) ;
#8534 = DIRECTION ( 'NONE',  ( 0.000000000000000000, 0.000000000000000000, 1.000000000000000000 ) ) ;
#8535 = CARTESIAN_POINT ( 'NONE',  ( 0.000000000000000000, -8.725776631572617958, -3.753907720749127819 ) ) ;
#8536 = CONTEXT_DEPENDENT_SHAPE_REPRESENTATION ( #19762, #3770 ) ;
#8537 = CIRCLE ( 'NONE', #497, 6.000000000000002665 ) ;
#8538 = DIRECTION ( 'NONE',  ( 0.000000000000000000, 0.000000000000000000, -1.000000000000000000 ) ) ;
#8539 = DIRECTION ( 'NONE',  ( 1.836970198721029934E-16, -1.000000000000000000, 0.000000000000000000 ) ) ;
#8540 = ORIENTED_EDGE ( 'NONE', *, *, #23757, .F. ) ;
#8541 = CIRCLE ( 'NONE', #5150, 22.00000000000000000 ) ;
#8542 = CARTESIAN_POINT ( 'NONE',  ( 3.799999999999999822, -2.710505431213761085E-17, 30.00000000000000000 ) ) ;
#8543 = DIRECTION ( 'NONE',  ( 1.000000000000000000, 0.000000000000000000, -0.000000000000000000 ) ) ;
#8544 = DIRECTION ( 'NONE',  ( -1.000000000000000000, 0.000000000000000000, 0.000000000000000000 ) ) ;
#8545 = ORIENTED_EDGE ( 'NONE', *, *, #3781, .F. ) ;
#8546 = CARTESIAN_POINT ( 'NONE',  ( -37.97545270896702618, -114.4734759653044023, 6.152725545821551734 ) ) ;
#8547 = ORIENTED_EDGE ( 'NONE', *, *, #17533, .T. ) ;
#8548 = ORIENTED_EDGE ( 'NONE', *, *, #7090, .F. ) ;
#8549 = ORIENTED_EDGE ( 'NONE', *, *, #25774, .F. ) ;
#8550 = DIRECTION ( 'NONE',  ( -1.000000000000000000, 0.000000000000000000, 0.000000000000000000 ) ) ;
#8551 = CARTESIAN_POINT ( 'NONE',  ( -35.50000000000000711, -115.1770117227680998, -1.611965039240062181 ) ) ;
#8552 = CYLINDRICAL_SURFACE ( 'NONE', #7025, 3.799999999999999822 ) ;
#8553 = EDGE_CURVE ( 'NONE', #2578, #27197, #35551, .T. ) ;
#8554 = CARTESIAN_POINT ( 'NONE',  ( -35.50000000000000711, -114.5636144531578680, 9.676196722963288366 ) ) ;
#8555 = DIRECTION ( 'NONE',  ( 1.000000000000000000, 0.000000000000000000, -0.000000000000000000 ) ) ;
#8556 = EDGE_CURVE ( 'NONE', #22699, #26100, #14156, .T. ) ;
#8557 = VECTOR ( 'NONE', #13096, 1000.000000000000000 ) ;
#8558 = CARTESIAN_POINT ( 'NONE',  ( 7.999999999999992895, 0.000000000000000000, 0.000000000000000000 ) ) ;
#8559 = CARTESIAN_POINT ( 'NONE',  ( 4.000000000000003553, -50.95304419620817526, -10.38206564895716255 ) ) ;
#8560 = DIRECTION ( 'NONE',  ( -1.000000000000000000, 0.000000000000000000, 0.000000000000000000 ) ) ;
#8561 = AXIS2_PLACEMENT_3D ( 'NONE', #5823, #22364, #25447 ) ;
#8562 = CARTESIAN_POINT ( 'NONE',  ( 0.000000000000000000, 0.000000000000000000, 0.000000000000000000 ) ) ;
#8563 = EDGE_CURVE ( 'NONE', #28842, #9210, #8985, .T. ) ;
#8564 = CARTESIAN_POINT ( 'NONE',  ( -36.07812499999994316, -115.9929510916434481, 14.11852480586265024 ) ) ;
#8565 = CARTESIAN_POINT ( 'NONE',  ( 0.000000000000000000, -1.000000000000001554, 38.00000000000000000 ) ) ;
#8566 = EDGE_CURVE ( 'NONE', #28118, #17419, #11494, .T. ) ;
#8567 = DIRECTION ( 'NONE',  ( 0.000000000000000000, 0.000000000000000000, 1.000000000000000000 ) ) ;
#8568 = DIRECTION ( 'NONE',  ( 0.000000000000000000, 0.000000000000000000, -1.000000000000000000 ) ) ;
#8569 = CARTESIAN_POINT ( 'NONE',  ( -27.00000000000000000, 45.00000000000000000, 0.000000000000000000 ) ) ;
#8570 = DIRECTION ( 'NONE',  ( -1.000000000000000000, -0.000000000000000000, 0.000000000000000000 ) ) ;
#8571 = CARTESIAN_POINT ( 'NONE',  ( 0.000000000000000000, 0.000000000000000000, 0.000000000000000000 ) ) ;
#8572 = ORIENTED_EDGE ( 'NONE', *, *, #31314, .T. ) ;
#8573 = CARTESIAN_POINT ( 'NONE',  ( -38.37230871539094323, -115.4561184093552413, 9.058975545821551734 ) ) ;
#8574 = CYLINDRICAL_SURFACE ( 'NONE', #18688, 11.00000000000000000 ) ;
#8575 = DIRECTION ( 'NONE',  ( -1.226634733346697831E-16, 0.9659258262890715319, -0.2588190451025083605 ) ) ;
#8576 = CARTESIAN_POINT ( 'NONE',  ( 7.999999999999992895, 0.000000000000000000, 0.000000000000000000 ) ) ;
#8577 = ORIENTED_EDGE ( 'NONE', *, *, #13892, .F. ) ;
#8578 = ORIENTED_EDGE ( 'NONE', *, *, #8796, .T. ) ;
#8579 = CARTESIAN_POINT ( 'NONE',  ( -34.49999999999998579, -29.27980021920982523, 82.28589838486210795 ) ) ;
#8580 = DIRECTION ( 'NONE',  ( -1.000000000000000000, -0.000000000000000000, -0.000000000000000000 ) ) ;
#8581 = ORIENTED_EDGE ( 'NONE', *, *, #5481, .T. ) ;
#8582 = ORIENTED_EDGE ( 'NONE', *, *, #14899, .T. ) ;
#8583 = EDGE_CURVE ( 'NONE', #33867, #30988, #956, .T. ) ;
#8584 = VECTOR ( 'NONE', #10609, 1000.000000000000000 ) ;
#8585 = DIRECTION ( 'NONE',  ( 0.000000000000000000, -0.5877852522924801315, 0.8090169943749422332 ) ) ;
#8586 = DIRECTION ( 'NONE',  ( 0.000000000000000000, 0.4999999999999948375, 0.8660254037844415942 ) ) ;
#8587 = DIRECTION ( 'NONE',  ( 0.000000000000000000, 0.000000000000000000, -1.000000000000000000 ) ) ;
#8588 = CARTESIAN_POINT ( 'NONE',  ( -39.49999999999999289, -11.24969279549607748, 111.5585998451919778 ) ) ;
#8589 = ORIENTED_EDGE ( 'NONE', *, *, #4009, .T. ) ;
#8590 = ORIENTED_EDGE ( 'NONE', *, *, #6279, .F. ) ;
#8591 = EDGE_CURVE ( 'NONE', #34626, #28884, #379, .T. ) ;
#8592 = CARTESIAN_POINT ( 'NONE',  ( 0.000000000000000000, -18.62763138773848581, -2.494040418455559127 ) ) ;
#8593 = EDGE_CURVE ( 'NONE', #26100, #18471, #30872, .T. ) ;
#8594 = EDGE_CURVE ( 'NONE', #33466, #8628, #2708, .T. ) ;
#8595 = FACE_OUTER_BOUND ( 'NONE', #21731, .T. ) ;
#8596 = ORIENTED_EDGE ( 'NONE', *, *, #6169, .T. ) ;
#8597 = FACE_OUTER_BOUND ( 'NONE', #31992, .T. ) ;
#8598 = DIRECTION ( 'NONE',  ( -1.000000000000000000, 0.000000000000000000, 0.000000000000000000 ) ) ;
#8599 = CARTESIAN_POINT ( 'NONE',  ( -35.61121590948313553, -114.9929510916434339, 14.07058620477040733 ) ) ;
#8600 = CARTESIAN_POINT ( 'NONE',  ( -35.50000000000000000, -113.9929510916434339, 10.52000928670414126 ) ) ;
#8601 = CARTESIAN_POINT ( 'NONE',  ( 8.000000000000000000, 3.872983346207417021, 0.9999999999999985567 ) ) ;
#8602 = ADVANCED_FACE ( 'NONE', ( #19419 ), #30417, .T. ) ;
#8603 = CARTESIAN_POINT ( 'NONE',  ( -35.90191880024783444, -114.9929510916434339, 14.11551573851448893 ) ) ;
#8604 = DIRECTION ( 'NONE',  ( 0.000000000000000000, 0.000000000000000000, 1.000000000000000000 ) ) ;
#8605 = ADVANCED_FACE ( 'NONE', ( #30235 ), #5574, .T. ) ;
#8606 = DIRECTION ( 'NONE',  ( 0.000000000000000000, 0.1253332335642974860, 0.9921147013144787641 ) ) ;
#8607 = CARTESIAN_POINT ( 'NONE',  ( 0.000000000000000000, 25.61928775981044026, 45.25098998563487385 ) ) ;
#8608 = CIRCLE ( 'NONE', #1173, 22.00000000000000000 ) ;
#8609 = DIRECTION ( 'NONE',  ( 0.000000000000000000, -0.9048270524660146918, -0.4257792915650830956 ) ) ;
#8610 = DIRECTION ( 'NONE',  ( 0.000000000000000000, 0.000000000000000000, -1.000000000000000000 ) ) ;
#8611 = ORIENTED_EDGE ( 'NONE', *, *, #29961, .F. ) ;
#8612 = DIRECTION ( 'NONE',  ( 0.000000000000000000, -0.1253332335643113082, 0.9921147013144769877 ) ) ;
#8613 = VERTEX_POINT ( 'NONE', #33110 ) ;
#8614 = AXIS2_PLACEMENT_3D ( 'NONE', #26035, #17737, #644 ) ;
#8615 = PRODUCT_DEFINITION_FORMATION_WITH_SPECIFIED_SOURCE ( 'ANY', '', #18142, .NOT_KNOWN. ) ;
#8616 = CARTESIAN_POINT ( 'NONE',  ( -34.00000000000000000, -114.0592624029313242, 7.503524454178450043 ) ) ;
#8617 = AXIS2_PLACEMENT_3D ( 'NONE', #320, #5561, #32923 ) ;
#8618 = DIRECTION ( 'NONE',  ( 0.000000000000000000, 0.000000000000000000, 1.000000000000000000 ) ) ;
#8619 = CARTESIAN_POINT ( 'NONE',  ( -35.50000000000000711, -114.5974311500472425, -1.624782352598427959 ) ) ;
#8620 = ORIENTED_EDGE ( 'NONE', *, *, #13808, .F. ) ;
#8621 = VERTEX_POINT ( 'NONE', #329 ) ;
#8622 = CARTESIAN_POINT ( 'NONE',  ( 8.000000000000000000, 14.18878633068160866, 6.236773481718133283 ) ) ;
#8623 = DIRECTION ( 'NONE',  ( -1.000000000000000000, 0.000000000000000000, -0.000000000000000000 ) ) ;
#8624 = ORIENTED_EDGE ( 'NONE', *, *, #35054, .T. ) ;
#8625 = EDGE_CURVE ( 'NONE', #13147, #25713, #5400, .T. ) ;
#8626 = DIRECTION ( 'NONE',  ( 1.000000000000000000, 0.000000000000000000, -0.000000000000000000 ) ) ;
#8627 = DIRECTION ( 'NONE',  ( -1.047965281155519790E-16, -6.938893903907192632E-17, -1.000000000000000000 ) ) ;
#8628 = VERTEX_POINT ( 'NONE', #16347 ) ;
#8630 = EDGE_LOOP ( 'NONE', ( #10739, #30864, #30559, #26776 ) ) ;
#8629 = EDGE_CURVE ( 'NONE', #577, #27296, #11315, .T. ) ;
#8631 = CARTESIAN_POINT ( 'NONE',  ( 0.000000000000000000, 0.000000000000000000, 0.000000000000000000 ) ) ;
#8632 = AXIS2_PLACEMENT_3D ( 'NONE', #15902, #27266, #35558 ) ;
#8633 = EDGE_CURVE ( 'NONE', #22893, #14025, #3227, .T. ) ;
#8634 =( NAMED_UNIT ( * ) PLANE_ANGLE_UNIT ( ) SI_UNIT ( $, .RADIAN. ) );
#8635 = LINE ( 'NONE', #8807, #1231 ) ;
#8636 = VERTEX_POINT ( 'NONE', #2532 ) ;
#8637 = VERTEX_POINT ( 'NONE', #10798 ) ;
#8638 = CIRCLE ( 'NONE', #28184, 10.50000000000000178 ) ;
#8639 = CARTESIAN_POINT ( 'NONE',  ( -35.50000000000000000, -113.8814751941374652, 2.992951091643117678 ) ) ;
#8640 = ADVANCED_BREP_SHAPE_REPRESENTATION ( '', ( #22482, #21307 ), #21360 ) ;
#8641 = EDGE_CURVE ( 'NONE', #30224, #9823, #29729, .T. ) ;
#8642 = AXIS2_PLACEMENT_3D ( 'NONE', #31209, #6017, #9418 ) ;
#8643 = CIRCLE ( 'NONE', #9803, 52.00000000000000711 ) ;
#8644 = ORIENTED_EDGE ( 'NONE', *, *, #35432, .F. ) ;
#8645 = EDGE_CURVE ( 'NONE', #17521, #14609, #21757, .T. ) ;
#8646 = CARTESIAN_POINT ( 'NONE',  ( -35.50000000000000711, -114.9929510916434339, 12.39849696637031506 ) ) ;
#8647 = CARTESIAN_POINT ( 'NONE',  ( -34.50000000000000000, -113.9929510916434339, 11.38636890470581164 ) ) ;
#8648 = CARTESIAN_POINT ( 'NONE',  ( -39.00000000000000711, -114.9929510916434339, 10.50625754673587231 ) ) ;
#8649 = DIRECTION ( 'NONE',  ( -1.000000000000000000, 0.000000000000000000, 0.000000000000000000 ) ) ;
#8650 = CARTESIAN_POINT ( 'NONE',  ( -34.50000000000000000, -113.9929510916434339, 10.50625754673586876 ) ) ;
#8651 = CARTESIAN_POINT ( 'NONE',  ( 2.600000000000004974, -12.74999999999999822, -1.200000000000006617 ) ) ;
#8652 = CARTESIAN_POINT ( 'NONE',  ( -35.50000000000000711, -114.9929510916434339, 11.38636890470581164 ) ) ;
#8653 = FACE_OUTER_BOUND ( 'NONE', #25871, .T. ) ;
#8654 = CARTESIAN_POINT ( 'NONE',  ( -34.49999999999998579, -27.48076211353314591, 80.99999999999988631 ) ) ;
#8655 = ORIENTED_EDGE ( 'NONE', *, *, #1703, .T. ) ;
#8656 = VERTEX_POINT ( 'NONE', #3052 ) ;
#8657 = AXIS2_PLACEMENT_3D ( 'NONE', #3222, #8598, #31108 ) ;
#8658 = CARTESIAN_POINT ( 'NONE',  ( 1.498621416870377088, 0.000000000000000000, 0.000000000000000000 ) ) ;
#8659 = CARTESIAN_POINT ( 'NONE',  ( 0.000000000000000000, -13.55483219355720337, -11.06713717293254362 ) ) ;
#8660 = ORIENTED_EDGE ( 'NONE', *, *, #7952, .F. ) ;
#8661 = DIRECTION ( 'NONE',  ( 0.000000000000000000, -6.938893903907204958E-17, -1.000000000000000000 ) ) ;
#8662 = ORIENTED_EDGE ( 'NONE', *, *, #8840, .F. ) ;
#8663 = CARTESIAN_POINT ( 'NONE',  ( -35.50000000000000000, -113.0349311500474982, -0.6247823525985715110 ) ) ;
#8664 = CARTESIAN_POINT ( 'NONE',  ( 4.000000000000003553, -19.74581912682874929, 48.10512059033386834 ) ) ;
#8665 = CARTESIAN_POINT ( 'NONE',  ( -36.94073759706868287, -112.0000000000000142, 5.628524454178449155 ) ) ;
#8666 = CIRCLE ( 'NONE', #34568, 7.199999999999998401 ) ;
#8667 = PRESENTATION_LAYER_ASSIGNMENT (  '', '', ( #17268 ) ) ;
#8668 = AXIS2_PLACEMENT_3D ( 'NONE', #10999, #16903, #28267 ) ;
#8669 = DIRECTION ( 'NONE',  ( -1.000000000000000000, 0.000000000000000000, 0.000000000000000000 ) ) ;
#8670 = ADVANCED_FACE ( 'NONE', ( #22292 ), #10974, .T. ) ;
#8671 = ORIENTED_EDGE ( 'NONE', *, *, #197, .F. ) ;
#8672 = EDGE_CURVE ( 'NONE', #27894, #21954, #14190, .T. ) ;
#8673 = DIRECTION ( 'NONE',  ( -1.000000000000000000, 6.056754644426116516E-31, -1.734723475976807094E-16 ) ) ;
#8674 = CARTESIAN_POINT ( 'NONE',  ( -35.50000000000000711, -112.0140978167138712, 0.7189676474015718188 ) ) ;
#8675 = VERTEX_POINT ( 'NONE', #8777 ) ;
#8676 = EDGE_LOOP ( 'NONE', ( #1244, #15355, #1148, #22106 ) ) ;
#8677 = CARTESIAN_POINT ( 'NONE',  ( -35.00000000000000000, -114.0592624029313242, 6.003524454178450043 ) ) ;
#8678 = CARTESIAN_POINT ( 'NONE',  ( 44.00000000000000000, -3.999999999999977351, 0.000000000000000000 ) ) ;
#8679 = VERTEX_POINT ( 'NONE', #22819 ) ;
#8680 = VERTEX_POINT ( 'NONE', #12208 ) ;
#8681 = CARTESIAN_POINT ( 'NONE',  ( -34.50000000000000000, -112.0140978167138712, 0.2502176474015765373 ) ) ;
#8682 = CARTESIAN_POINT ( 'NONE',  ( 7.999999999999992895, -44.47301969247457976, 16.68249143361895293 ) ) ;
#8683 = CIRCLE ( 'NONE', #18454, 9.999999999999994671 ) ;
#8684 = B_SPLINE_CURVE_WITH_KNOTS ( 'NONE', 3,
 ( #9227, #29529, #3844, #11934, #31191, #14804, #25811, #4698, #24125, #26471, #18526, #23758, #22904, #12108, #31853, #32041, #12957, #15454, #34938, #1806, #18349, #10263, #12780, #4863, #35116, #15806, #10439, #21398, #32395, #28319, #14615, #20183, #16164, #16529, #5739, #16697, #2521, #33281, #8072, #29696, #24299, #5566, #10965, #8248, #17215, #10610, #16339, #3044, #27182, #2876, #21751, #32927, #24999, #13838, #18698, #13490, #7897, #21932, #24650, #19224, #30228, #27540, #24825, #27354, #149, #11316, #35460, #11140, #14005, #5392, #35289, #22109, #18881, #33105, #19055, #10791, #324, #8426, #19411, #24473, #2702, #30411, #27709, #22285, #5041, #15990, #27004, #2350, #13670, #13320, #21567, #32563, #29878, #5224, #32744, #30054, #20276, #8950, #5906, #33619, #14520, #11833 ),
 .UNSPECIFIED., .F., .F.,
 ( 4, 2, 2, 2, 2, 2, 2, 2, 2, 2, 2, 2, 2, 2, 2, 2, 2, 2, 2, 2, 2, 2, 2, 2, 2, 2, 2, 2, 2, 2, 2, 2, 2, 2, 2, 2, 2, 2, 2, 2, 2, 2, 2, 2, 2, 2, 2, 2, 2, 2, 4 ),
 ( 0.000000000000000000, 0.05194669433742771930, 0.07792004150614158242, 0.09090671509049851051, 0.09740005188267697456, 0.1038933886748554386, 0.1123700156520060500, 0.1208466426291566476, 0.1377998965834578704, 0.1717064044920602883, 0.2056129124006627062, 0.2225661663549639291, 0.2310427933321145266, 0.2395194203092651519, 0.2482763131408625423, 0.2570332059724599327, 0.2745469916356546580, 0.3095745629620442196, 0.3446021342884337813, 0.3621159199516285621, 0.3708728127832259247, 0.3796297056148233429, 0.3887999023441631730, 0.3979700990735030031, 0.4163104925321826633, 0.4529912794495420392, 0.4896720663669014151, 0.5080124598255810753, 0.5171826565549209054, 0.5263528532842607355, 0.5380287103930572190, 0.5497045675018538136, 0.5730562817194468916, 0.6197597101546329368, 0.6664631385898189819, 0.6898148528074120600, 0.7014907099162086546, 0.7131665670250051381, 0.7223367637543449682, 0.7315069604836847983, 0.7498473539423643475, 0.7865281408597235568, 0.8232089277770826552, 0.8415493212357623154, 0.8507195179651021455, 0.8598897146944418646, 0.8686466075260392827, 0.8774035003576365899, 0.8949172860208314262, 0.9299448573472208768, 1.000000000000000000 ),
 .UNSPECIFIED. ) ;
#8685 = ORIENTED_EDGE ( 'NONE', *, *, #8152, .F. ) ;
#8686 = DIRECTION ( 'NONE',  ( 0.000000000000000000, -0.9048270524660235736, 0.4257792915650639998 ) ) ;
#8687 = CARTESIAN_POINT ( 'NONE',  ( -35.50025087934803736, -113.9929510916434339, 12.63488142334835196 ) ) ;
#8688 = LINE ( 'NONE', #31016, #17855 ) ;
#8689 = CYLINDRICAL_SURFACE ( 'NONE', #18221, 8.000000000000014211 ) ;
#8690 = VECTOR ( 'NONE', #12080, 1000.000000000000000 ) ;
#8691 = VECTOR ( 'NONE', #18340, 1000.000000000000000 ) ;
#8692 = CARTESIAN_POINT ( 'NONE',  ( -34.50000000000000000, -112.8690837874180062, 2.872105769100646189 ) ) ;
#8693 = CARTESIAN_POINT ( 'NONE',  ( -35.50000000000000000, -114.1185248058629611, 8.507048908356933836 ) ) ;
#8694 = DIRECTION ( 'NONE',  ( -1.000000000000000000, 0.000000000000000000, 0.000000000000000000 ) ) ;
#8695 = APPLICATION_CONTEXT ( 'automotive_design' ) ;
#8696 = DIRECTION ( 'NONE',  ( 0.000000000000000000, 0.000000000000000000, -1.000000000000000000 ) ) ;
#8697 = VERTEX_POINT ( 'NONE', #28414 ) ;
#8698 = DIRECTION ( 'NONE',  ( -1.000000000000000000, 0.000000000000000000, 0.000000000000000000 ) ) ;
#8699 = DIRECTION ( 'NONE',  ( -1.000000000000000000, -0.000000000000000000, -0.000000000000000000 ) ) ;
#8700 = FACE_OUTER_BOUND ( 'NONE', #10948, .T. ) ;
#8701 = ORIENTED_EDGE ( 'NONE', *, *, #26688, .F. ) ;
#8702 = DIRECTION ( 'NONE',  ( -1.000000000000000000, -1.836970198721029934E-16, -0.000000000000000000 ) ) ;
#8703 = CARTESIAN_POINT ( 'NONE',  ( 0.000000000000000000, -2.710505431213761085E-17, -30.00000000000000711 ) ) ;
#8704 = DIRECTION ( 'NONE',  ( 1.734723475976807094E-16, -1.000000000000000000, 0.000000000000000000 ) ) ;
#8705 = CARTESIAN_POINT ( 'NONE',  ( 4.000000000000003553, 25.61928775981044026, 45.25098998563487385 ) ) ;
#8706 = PLANE ( 'NONE',  #20438 ) ;
#8707 = CARTESIAN_POINT ( 'NONE',  ( -10.00000000000000000, 0.000000000000000000, 0.000000000000000000 ) ) ;
#8708 = VERTEX_POINT ( 'NONE', #25903 ) ;
#8709 = EDGE_CURVE ( 'NONE', #17425, #20467, #23390, .T. ) ;
#8710 = FILL_AREA_STYLE_COLOUR ( '', #29124 ) ;
#8711 = DIRECTION ( 'NONE',  ( 1.000000000000000000, -4.625929269271460867E-15, -1.156482317317865217E-15 ) ) ;
#8712 = DIRECTION ( 'NONE',  ( -1.000000000000000000, 0.000000000000000000, 0.000000000000000000 ) ) ;
#8713 = ORIENTED_EDGE ( 'NONE', *, *, #14812, .F. ) ;
#8714 = CARTESIAN_POINT ( 'NONE',  ( -38.02454729103295961, -113.6450488405582462, 3.340225545821551290 ) ) ;
#8715 = ORIENTED_EDGE ( 'NONE', *, *, #4390, .T. ) ;
#8716 = VECTOR ( 'NONE', #12647, 1000.000000000000000 ) ;
#8717 = AXIS2_PLACEMENT_3D ( 'NONE', #28223, #28756, #28393 ) ;
#8718 = ORIENTED_EDGE ( 'NONE', *, *, #8805, .T. ) ;
#8719 = ORIENTED_EDGE ( 'NONE', *, *, #6638, .T. ) ;
#8720 = CARTESIAN_POINT ( 'NONE',  ( -4.121423858225413461, -12.61643262889540473, -1.200000000000006617 ) ) ;
#8721 = EDGE_CURVE ( 'NONE', #1074, #18771, #7859, .T. ) ;
#8722 = CARTESIAN_POINT ( 'NONE',  ( -35.50000000000000711, -116.0140978167138712, 0.0002176474015577116276 ) ) ;
#8723 = CARTESIAN_POINT ( 'NONE',  ( 3.799999999999999822, -2.710505431213761085E-17, -45.89999999999999858 ) ) ;
#8724 = CARTESIAN_POINT ( 'NONE',  ( -35.50000000000000711, -114.3464919575557843, 9.568884482464163455 ) ) ;
#8725 = DIRECTION ( 'NONE',  ( -1.000000000000000000, -0.000000000000000000, -0.000000000000000000 ) ) ;
#8726 = CARTESIAN_POINT ( 'NONE',  ( -35.50000000000000711, -116.0140978167138712, 0.8752176474015622709 ) ) ;
#8727 = CARTESIAN_POINT ( 'NONE',  ( -34.50000000000000000, -114.9929296450195721, 10.49869535309826674 ) ) ;
#8728 = DIRECTION ( 'NONE',  ( 0.000000000000000000, 0.000000000000000000, -1.000000000000000000 ) ) ;
#8729 = CARTESIAN_POINT ( 'NONE',  ( 55.00000000000000000, 20.00000000000001776, 120.0000000000000000 ) ) ;
#8730 = VECTOR ( 'NONE', #26778, 1000.000000000000000 ) ;
#8731 = CARTESIAN_POINT ( 'NONE',  ( -35.50000000000000000, -115.9382890315277308, 10.02636389016632812 ) ) ;
#8733 = CARTESIAN_POINT ( 'NONE',  ( -35.50000000000000711, -112.0140978167138712, 0.5627176474015717078 ) ) ;
#8732 = CIRCLE ( 'NONE', #33472, 47.49900000000001654 ) ;
#8734 = LINE ( 'NONE', #640, #13616 ) ;
#8735 = CARTESIAN_POINT ( 'NONE',  ( 8.000000000000000000, 0.000000000000000000, 0.000000000000000000 ) ) ;
#8736 = CARTESIAN_POINT ( 'NONE',  ( 8.000000000000007105, 9.604183132802452505, 5.908880290975567995 ) ) ;
#8737 =( REPRESENTATION_RELATIONSHIP ('NONE','NONE', #26607, #2005 ) REPRESENTATION_RELATIONSHIP_WITH_TRANSFORMATION ( #28870 )SHAPE_REPRESENTATION_RELATIONSHIP( ) );
#8738 = DIRECTION ( 'NONE',  ( 0.000000000000000000, 0.5877852522924682521, 0.8090169943749511150 ) ) ;
#8739 = ORIENTED_EDGE ( 'NONE', *, *, #31053, .T. ) ;
#8740 = CARTESIAN_POINT ( 'NONE',  ( -36.25098837183130485, -114.6652019342044184, 2.683975545821551734 ) ) ;
#8741 = CARTESIAN_POINT ( 'NONE',  ( 4.000000000000000000, 4.898587196589412829E-16, 55.00000000000000000 ) ) ;
#8742 = DIRECTION ( 'NONE',  ( 1.000000000000000000, 0.000000000000000000, 0.000000000000000000 ) ) ;
#8743 = CARTESIAN_POINT ( 'NONE',  ( -4.000000000000000000, 0.000000000000000000, -55.00000000000000000 ) ) ;
#8744 = ORIENTED_EDGE ( 'NONE', *, *, #1787, .F. ) ;
#8745 = STYLED_ITEM ( 'NONE', ( #7814 ), #22652 ) ;
#8746 = ORIENTED_EDGE ( 'NONE', *, *, #30806, .T. ) ;
#8747 = ADVANCED_FACE ( 'NONE', ( #14710, #19922 ), #28771, .F. ) ;
#8748 = CARTESIAN_POINT ( 'NONE',  ( 50.00000000000000000, 20.00000000000001776, -15.00000000000001421 ) ) ;
#8749 = DIRECTION ( 'NONE',  ( 0.000000000000000000, 0.000000000000000000, 1.000000000000000000 ) ) ;
#8750 = EDGE_LOOP ( 'NONE', ( #3635, #10679, #31101, #8018 ) ) ;
#8751 = ADVANCED_FACE ( 'NONE', ( #25724 ), #34178, .T. ) ;
#8752 = AXIS2_PLACEMENT_3D ( 'NONE', #13622, #16123, #27140 ) ;
#8753 = EDGE_LOOP ( 'NONE', ( #23857, #22410, #26439, #21904 ) ) ;
#8754 = CARTESIAN_POINT ( 'NONE',  ( 8.000000000000000000, 16.71027810728549667, 2.620268201066223934 ) ) ;
#8755 = CIRCLE ( 'NONE', #13385, 20.00000000000000355 ) ;
#8756 = FACE_OUTER_BOUND ( 'NONE', #15675, .T. ) ;
#8757 = EDGE_CURVE ( 'NONE', #10721, #15971, #20106, .T. ) ;
#8758 = CIRCLE ( 'NONE', #31187, 7.000000000000006217 ) ;
#8759 = PRODUCT_CONTEXT ( 'NONE', #14221, 'mechanical' ) ;
#8760 = DIRECTION ( 'NONE',  ( -1.000000000000000000, 0.000000000000000000, 0.000000000000000000 ) ) ;
#8761 = ORIENTED_EDGE ( 'NONE', *, *, #1582, .T. ) ;
#8762 = VERTEX_POINT ( 'NONE', #1232 ) ;
#8763 = DIRECTION ( 'NONE',  ( 1.000000000000000000, -0.000000000000000000, -0.000000000000000000 ) ) ;
#8764 = CYLINDRICAL_SURFACE ( 'NONE', #8617, 47.49900000000001654 ) ;
#8765 = VERTEX_POINT ( 'NONE', #31115 ) ;
#8766 = CYLINDRICAL_SURFACE ( 'NONE', #10920, 8.000000000000000000 ) ;
#8767 = VECTOR ( 'NONE', #32807, 1000.000000000000000 ) ;
#8768 = CARTESIAN_POINT ( 'NONE',  ( -34.50000000000000000, -115.0140978167138712, 0.0002176474015577929428 ) ) ;
#8769 = CARTESIAN_POINT ( 'NONE',  ( 7.999999999999992895, 0.000000000000000000, 0.000000000000000000 ) ) ;
#8770 = DIRECTION ( 'NONE',  ( 0.02040816326530617286, -0.9997917317482359900, 9.329158281316450075E-32 ) ) ;
#8771 = UNCERTAINTY_MEASURE_WITH_UNIT (LENGTH_MEASURE( 1.000000000000000082E-05 ), #6997, 'distance_accuracy_value', 'NONE');
#8772 = CARTESIAN_POINT ( 'NONE',  ( -34.50000000000000000, -114.2899554544714960, 8.528375582263644006 ) ) ;
#8773 = AXIS2_PLACEMENT_3D ( 'NONE', #25824, #5840, #14279 ) ;
#8774 = DIRECTION ( 'NONE',  ( -1.000000000000000000, -1.734723475976807094E-16, 0.000000000000000000 ) ) ;
#8775 = DIRECTION ( 'NONE',  ( 0.000000000000000000, 0.000000000000000000, 1.000000000000000000 ) ) ;
#8776 = CARTESIAN_POINT ( 'NONE',  ( -37.37500000000009237, -114.9929510916434339, 14.11852480586264846 ) ) ;
#8777 = CARTESIAN_POINT ( 'NONE',  ( -4.000000000000000000, 0.000000000000000000, 36.00000000000000000 ) ) ;
#8778 = EDGE_CURVE ( 'NONE', #6914, #11298, #10753, .T. ) ;
#8779 = CARTESIAN_POINT ( 'NONE',  ( 50.00005079999998969, 0.000000000000000000, 11.00000000000000000 ) ) ;
#8780 = CARTESIAN_POINT ( 'NONE',  ( 8.000000000000007105, 9.433698091065215507, 1.111908866155128628 ) ) ;
#8781 = DIRECTION ( 'NONE',  ( -1.000000000000000000, 0.000000000000000000, 0.000000000000000000 ) ) ;
#8782 = CIRCLE ( 'NONE', #17387, 52.00000000000000711 ) ;
#8783 = ORIENTED_EDGE ( 'NONE', *, *, #32390, .T. ) ;
#8784 = CIRCLE ( 'NONE', #19692, 20.00000000000000711 ) ;
#8785 = CARTESIAN_POINT ( 'NONE',  ( -2.321707774797454604, -4.824281976789094095, 0.000000000000000000 ) ) ;
#8786 = ORIENTED_EDGE ( 'NONE', *, *, #17935, .T. ) ;
#8787 = CARTESIAN_POINT ( 'NONE',  ( -34.83677480945819838, -111.9205845034225462, 2.816024454178448710 ) ) ;
#8788 = DIRECTION ( 'NONE',  ( 0.000000000000000000, 0.9510565162951544194, -0.3090169943749449533 ) ) ;
#8789 = CARTESIAN_POINT ( 'NONE',  ( -35.50000000000000711, -112.0460568841087223, -0.8839717462762063382 ) ) ;
#8790 = ORIENTED_EDGE ( 'NONE', *, *, #34637, .T. ) ;
#8791 = ORIENTED_EDGE ( 'NONE', *, *, #35444, .T. ) ;
#8792 = EDGE_CURVE ( 'NONE', #4315, #28212, #9325, .T. ) ;
#8793 = FACE_OUTER_BOUND ( 'NONE', #14540, .T. ) ;
#8794 = CARTESIAN_POINT ( 'NONE',  ( 8.000000000000007105, 5.679790370316031733, 7.613867765417614564 ) ) ;
#8795 = ADVANCED_FACE ( 'NONE', ( #17587 ), #20282, .T. ) ;
#8796 = EDGE_CURVE ( 'NONE', #27467, #32382, #24561, .T. ) ;
#8797 = VERTEX_POINT ( 'NONE', #1056 ) ;
#8798 = AXIS2_PLACEMENT_3D ( 'NONE', #32389, #27348, #24646 ) ;
#8799 = CIRCLE ( 'NONE', #20874, 19.99999999999998579 ) ;
#8800 = CARTESIAN_POINT ( 'NONE',  ( 8.000000000000000000, 0.000000000000000000, 0.000000000000000000 ) ) ;
#8801 = DIRECTION ( 'NONE',  ( -1.000000000000000000, 0.000000000000000000, 0.000000000000000000 ) ) ;
#8802 = ORIENTED_EDGE ( 'NONE', *, *, #30564, .T. ) ;
#8803 = VERTEX_POINT ( 'NONE', #12381 ) ;
#8804 = CARTESIAN_POINT ( 'NONE',  ( 7.999999999999992895, 11.90021268425554624, 45.45261810511217959 ) ) ;
#8805 = EDGE_CURVE ( 'NONE', #4061, #11629, #22809, .T. ) ;
#8806 = EDGE_CURVE ( 'NONE', #18916, #11231, #1404, .T. ) ;
#8807 = CARTESIAN_POINT ( 'NONE',  ( -42.49999999999999289, -27.48076211353314591, 80.99999999999987210 ) ) ;
#8808 = ORIENTED_EDGE ( 'NONE', *, *, #2029, .F. ) ;
#8809 = ORIENTED_EDGE ( 'NONE', *, *, #973, .F. ) ;
#8810 = CARTESIAN_POINT ( 'NONE',  ( -35.50000000000000000, -111.0278007905855588, 1.116632271043183078 ) ) ;
#8811 = CIRCLE ( 'NONE', #28952, 3.799999999999999822 ) ;
#8812 = CIRCLE ( 'NONE', #25512, 5.000000000000004441 ) ;
#8813 = AXIS2_PLACEMENT_3D ( 'NONE', #15349, #26361, #9966 ) ;
#8814 = ORIENTED_EDGE ( 'NONE', *, *, #21209, .F. ) ;
#8815 = CARTESIAN_POINT ( 'NONE',  ( -35.87040530316090070, -114.9929510916434339, 13.10254527216545917 ) ) ;
#8816 = CARTESIAN_POINT ( 'NONE',  ( -38.81062062679291813, -113.9929510916434339, 13.37409560816442244 ) ) ;
#8817 = FACE_BOUND ( 'NONE', #12432, .T. ) ;
#8818 = DIRECTION ( 'NONE',  ( -1.000000000000000000, -0.000000000000000000, 0.000000000000000000 ) ) ;
#8819 = CARTESIAN_POINT ( 'NONE',  ( -34.50000000000000000, -113.9929510916434623, 10.50436693183592141 ) ) ;
#8820 = CARTESIAN_POINT ( 'NONE',  ( -38.25557080230232998, -114.9929510916434339, 13.92914543265419525 ) ) ;
#8821 = EDGE_CURVE ( 'NONE', #33549, #28885, #27999, .T. ) ;
#8822 = CARTESIAN_POINT ( 'NONE',  ( -35.50000000000000711, -114.6604609523327838, 9.751889438017201428 ) ) ;
#8823 = CARTESIAN_POINT ( 'NONE',  ( -4.000000000000000000, -2.710505431213761085E-17, 55.00000000000000000 ) ) ;
#8824 = AXIS2_PLACEMENT_3D ( 'NONE', #5910, #3224, #9680 ) ;
#8825 = CARTESIAN_POINT ( 'NONE',  ( 7.999999999999992895, -44.75336757549767697, -14.30704879393654494 ) ) ;
#8826 = ORIENTED_EDGE ( 'NONE', *, *, #5401, .T. ) ;
#8827 = PRODUCT_DEFINITION ( 'UNKNOWN', '', #7463, #25263 ) ;
#8828 = ORIENTED_EDGE ( 'NONE', *, *, #28851, .F. ) ;
#8829 = EDGE_CURVE ( 'NONE', #17787, #21028, #31292, .T. ) ;
#8830 = CARTESIAN_POINT ( 'NONE',  ( -90.00000000000002842, -4.694161725993254197E-16, -6.765000000000038760 ) ) ;
#8831 = LINE ( 'NONE', #23595, #14532 ) ;
#8832 = VERTEX_POINT ( 'NONE', #6616 ) ;
#8833 = DIRECTION ( 'NONE',  ( 0.000000000000000000, 0.000000000000000000, 1.000000000000000000 ) ) ;
#8834 = ORIENTED_EDGE ( 'NONE', *, *, #30037, .F. ) ;
#8835 = AXIS2_PLACEMENT_3D ( 'NONE', #23240, #34055, #23055 ) ;
#8836 = VECTOR ( 'NONE', #26744, 1000.000000000000000 ) ;
#8837 = CARTESIAN_POINT ( 'NONE',  ( -35.50000000000000000, -115.0140978167140986, -0.6247823525984417259 ) ) ;
#8838 = CARTESIAN_POINT ( 'NONE',  ( 0.000000000000000000, 0.000000000000000000, 0.000000000000000000 ) ) ;
#8839 = CARTESIAN_POINT ( 'NONE',  ( -37.05926240293131713, -115.9999999999999858, 4.878524454178449155 ) ) ;
#8840 = EDGE_CURVE ( 'NONE', #1331, #17998, #14769, .T. ) ;
#8841 = EDGE_CURVE ( 'NONE', #7873, #32273, #856, .T. ) ;
#8842 = EDGE_LOOP ( 'NONE', ( #16318, #22400, #16945, #8526, #8582, #10420 ) ) ;
#8843 = DIRECTION ( 'NONE',  ( 0.000000000000000000, -0.5735764363510502672, 0.8191520442889889120 ) ) ;
#8844 = ORIENTED_EDGE ( 'NONE', *, *, #15774, .F. ) ;
#8845 = AXIS2_PLACEMENT_3D ( 'NONE', #30562, #24812, #14337 ) ;
#8846 = CARTESIAN_POINT ( 'NONE',  ( 7.999999999999992895, -22.82995208772657492, -41.06517797613687293 ) ) ;
#8847 = CARTESIAN_POINT ( 'NONE',  ( -35.50000000000000711, -112.0414288467712112, 1.115164475686276191 ) ) ;
#8848 = ORIENTED_EDGE ( 'NONE', *, *, #16902, .T. ) ;
#8849 = VERTEX_POINT ( 'NONE', #17769 ) ;
#8850 = CARTESIAN_POINT ( 'NONE',  ( -38.37230871539094323, -112.5438815906447729, 8.441024454178448266 ) ) ;
#8851 = FILL_AREA_STYLE ('',( #25435 ) ) ;
#8852 = EDGE_CURVE ( 'NONE', #31771, #8899, #14182, .T. ) ;
#8853 = CARTESIAN_POINT ( 'NONE',  ( 0.000000000000000000, 8.053585752062575764, -46.81126742072014224 ) ) ;
#8855 = ORIENTED_EDGE ( 'NONE', *, *, #19173, .T. ) ;
#8854 = AXIS2_PLACEMENT_3D ( 'NONE', #8525, #14445, #32351 ) ;
#8856 = ORIENTED_EDGE ( 'NONE', *, *, #31967, .F. ) ;
#8857 = CARTESIAN_POINT ( 'NONE',  ( -34.50000000000000000, -115.0140978167138712, -0.4997823525984417259 ) ) ;
#8858 = CARTESIAN_POINT ( 'NONE',  ( -34.49999999999998579, -18.23076211353320275, 77.24999999999991473 ) ) ;
#8859 = ORIENTED_EDGE ( 'NONE', *, *, #22905, .T. ) ;
#8860 = ORIENTED_EDGE ( 'NONE', *, *, #29343, .T. ) ;
#8861 = CARTESIAN_POINT ( 'NONE',  ( 3.872983346207416133, 1.000000000000001110, 55.00000000000000000 ) ) ;
#8862 = AXIS2_PLACEMENT_3D ( 'NONE', #32727, #18504, #4677 ) ;
#8863 = CARTESIAN_POINT ( 'NONE',  ( -35.50000000000000000, -113.9929510916434339, 10.50763272073269405 ) ) ;
#8864 = VECTOR ( 'NONE', #32758, 1000.000000000000000 ) ;
#8865 = CARTESIAN_POINT ( 'NONE',  ( 0.000000000000000000, 8.605879768205412006, -12.89022243466699535 ) ) ;
#8866 = DIRECTION ( 'NONE',  ( 1.000000000000000000, -0.000000000000000000, -0.000000000000000000 ) ) ;
#8867 = CARTESIAN_POINT ( 'NONE',  ( -34.50000000000000000, -116.0140978167138712, -0.3122823525984417259 ) ) ;
#8868 = ADVANCED_FACE ( 'NONE', ( #18662 ), #20814, .T. ) ;
#8869 = CARTESIAN_POINT ( 'NONE',  ( -35.50000000000000000, -114.2207110452431635, 8.519246492191951958 ) ) ;
#8870 = FACE_OUTER_BOUND ( 'NONE', #25063, .T. ) ;
#8871 = EDGE_CURVE ( 'NONE', #31100, #6235, #21363, .T. ) ;
#8872 = DIRECTION ( 'NONE',  ( -1.783119874454246424E-31, -1.187911941725854497E-31, 1.000000000000000000 ) ) ;
#8873 = EDGE_CURVE ( 'NONE', #6113, #34165, #28563, .T. ) ;
#8874 = DIRECTION ( 'NONE',  ( 0.000000000000000000, 0.000000000000000000, -1.000000000000000000 ) ) ;
#8875 = DIRECTION ( 'NONE',  ( 0.000000000000000000, 1.000000000000000000, 0.000000000000000000 ) ) ;
#8876 = CARTESIAN_POINT ( 'NONE',  ( 7.999999999999992895, -5.667686777401384823, -46.64153600743608763 ) ) ;
#8877 = ORIENTED_EDGE ( 'NONE', *, *, #15601, .T. ) ;
#8878 = CARTESIAN_POINT ( 'NONE',  ( -4.000000000000000000, -2.710505431213761085E-17, 55.00000000000000000 ) ) ;
#8879 = CARTESIAN_POINT ( 'NONE',  ( -2.321707774797454604, -4.824281976789094095, -0.7999999999999951594 ) ) ;
#8880 = CYLINDRICAL_SURFACE ( 'NONE', #418, 4.872650870659778199 ) ;
#8881 = LINE ( 'NONE', #33914, #9213 ) ;
#8882 = EDGE_CURVE ( 'NONE', #3424, #29247, #31637, .T. ) ;
#8883 = CONTEXT_DEPENDENT_SHAPE_REPRESENTATION ( #2795, #9221 ) ;
#8884 = ADVANCED_FACE ( 'NONE', ( #23720 ), #10036, .T. ) ;
#8885 = CARTESIAN_POINT ( 'NONE',  ( -34.49999999999998579, -25.98076211353320986, 84.99999999999994316 ) ) ;
#8886 = DIRECTION ( 'NONE',  ( 1.000000000000000000, 0.000000000000000000, 0.000000000000000000 ) ) ;
#8887 = ORIENTED_EDGE ( 'NONE', *, *, #26894, .F. ) ;
#8888 = CIRCLE ( 'NONE', #10631, 19.99999999999998579 ) ;
#8889 = CARTESIAN_POINT ( 'NONE',  ( 7.999999999999992895, 42.60732521687570795, 19.80331771201672453 ) ) ;
#8890 = CIRCLE ( 'NONE', #16921, 8.000000000000001776 ) ;
#8891 = CARTESIAN_POINT ( 'NONE',  ( 7.999999999999992895, 43.83938735307269496, 18.28286404005814703 ) ) ;
#8892 = CARTESIAN_POINT ( 'NONE',  ( 0.000000000000000000, -42.60732521687556584, -19.80331771201704427 ) ) ;
#8893 = EDGE_LOOP ( 'NONE', ( #23925, #10419, #34822, #18139 ) ) ;
#8894 = CARTESIAN_POINT ( 'NONE',  ( -35.99999999999999289, -113.9407375970686758, 3.996475545821551734 ) ) ;
#8895 = ORIENTED_EDGE ( 'NONE', *, *, #10063, .T. ) ;
#8896 = CIRCLE ( 'NONE', #18095, 20.00000000000000711 ) ;
#8897 =( NAMED_UNIT ( * ) PLANE_ANGLE_UNIT ( ) SI_UNIT ( $, .RADIAN. ) );
#8898 = ORIENTED_EDGE ( 'NONE', *, *, #11982, .F. ) ;
#8899 = VERTEX_POINT ( 'NONE', #32002 ) ;
#8900 = CYLINDRICAL_SURFACE ( 'NONE', #6252, 4.800000000000000711 ) ;
#8901 = CARTESIAN_POINT ( 'NONE',  ( -35.50000000000000711, -116.0141056290913610, -0.5935324770972248976 ) ) ;
#8902 = DIRECTION ( 'NONE',  ( 0.000000000000000000, 0.4999999999999948930, 0.8660254037844415942 ) ) ;
#8903 = AXIS2_PLACEMENT_3D ( 'NONE', #14052, #5624, #28 ) ;
#8904 = CARTESIAN_POINT ( 'NONE',  ( -35.50000000000000711, -114.0650276068786582, 9.507762098804159123 ) ) ;
#8905 = CARTESIAN_POINT ( 'NONE',  ( 4.000000000000003553, 21.80633394113450052, -2.912696353505896063 ) ) ;
#8906 = CARTESIAN_POINT ( 'NONE',  ( -90.00000000000002842, 0.000000000000000000, 6.938893903907228378E-15 ) ) ;
#8907 = CARTESIAN_POINT ( 'NONE',  ( -34.50000000000000000, -114.0650276068786582, 9.507762098804159123 ) ) ;
#8908 = CYLINDRICAL_SURFACE ( 'NONE', #23751, 3.799999999999999822 ) ;
#8909 = EDGE_CURVE ( 'NONE', #29036, #26218, #7304, .T. ) ;
#8910 = PRODUCT ( 'spur gear_iso_ISO - Spur gear 2M 50T 20PA 8FW ---S50A75H50L22.0R1', 'spur gear_iso_ISO - Spur gear 2M 50T 20PA 8FW ---S50A75H50L22.0R1', '', ( #12010 ) ) ;
#8911 = VECTOR ( 'NONE', #28200, 1000.000000000000000 ) ;
#8912 = CARTESIAN_POINT ( 'NONE',  ( 7.999999999999992895, 43.83938735307295076, -18.28286404005752175 ) ) ;
#8913 = CARTESIAN_POINT ( 'NONE',  ( -39.00000000000000000, -115.9929510916434481, 11.91443571948719615 ) ) ;
#8914 = CARTESIAN_POINT ( 'NONE',  ( -35.50000000000000711, -112.6605569508015350, 1.812590711673265575 ) ) ;
#8915 = DIRECTION ( 'NONE',  ( -1.000000000000000000, 0.000000000000000000, 0.000000000000000000 ) ) ;
#8916 = AXIS2_PLACEMENT_3D ( 'NONE', #11079, #16636, #22045 ) ;
#8917 = DIRECTION ( 'NONE',  ( 0.000000000000000000, -1.000000000000000000, 0.000000000000000000 ) ) ;
#8918 = DIRECTION ( 'NONE',  ( -1.000000000000000000, 0.000000000000000000, 0.000000000000000000 ) ) ;
#8919 = CARTESIAN_POINT ( 'NONE',  ( 8.000000000000000000, -16.31134495048487310, 6.336799421339755156 ) ) ;
#8920 = CIRCLE ( 'NONE', #35395, 4.000000000000000000 ) ;
#8921 = FACE_OUTER_BOUND ( 'NONE', #8113, .T. ) ;
#8922 = CARTESIAN_POINT ( 'NONE',  ( 0.000000000000000000, 0.000000000000000000, -31.10000000000000142 ) ) ;
#8923 = VERTEX_POINT ( 'NONE', #32182 ) ;
#8924 = CARTESIAN_POINT ( 'NONE',  ( -36.33479806579560289, -113.2509883718313262, 9.808975545821553510 ) ) ;
#8925 = DIRECTION ( 'NONE',  ( -0.000000000000000000, 0.2588190451025275673, -0.9659258262890664248 ) ) ;
#8926 = CARTESIAN_POINT ( 'NONE',  ( 0.000000000000000000, 0.000000000000000000, -0.7999999999999951594 ) ) ;
#8927 = DIRECTION ( 'NONE',  ( -1.000000000000000000, 0.000000000000000000, 0.000000000000000000 ) ) ;
#8928 = VERTEX_POINT ( 'NONE', #26433 ) ;
#8929 = AXIS2_PLACEMENT_3D ( 'NONE', #23590, #4709, #13331 ) ;
#8930 = ORIENTED_EDGE ( 'NONE', *, *, #18067, .T. ) ;
#8931 = DIRECTION ( 'NONE',  ( -1.000000000000000000, 0.000000000000000000, -0.000000000000000000 ) ) ;
#8932 = CARTESIAN_POINT ( 'NONE',  ( 4.000000000000000000, 4.898587196589412829E-16, -65.00000000000000000 ) ) ;
#8933 = EDGE_LOOP ( 'NONE', ( #15478, #4467, #5066, #10130 ) ) ;
#8934 = CARTESIAN_POINT ( 'NONE',  ( -37.05926240293133134, -116.9999999999999858, 7.878524454178450043 ) ) ;
#8935 = VERTEX_POINT ( 'NONE', #34712 ) ;
#8936 = DIRECTION ( 'NONE',  ( -1.174092375852890260E-15, 4.222049128630259891E-16, 1.000000000000000000 ) ) ;
#8937 = CARTESIAN_POINT ( 'NONE',  ( 0.000000000000000000, 0.000000000000000000, -32.00000000000000000 ) ) ;
#8938 = APPLICATION_PROTOCOL_DEFINITION ( 'draft international standard', 'automotive_design', 1998, #24379 ) ;
#8939 = VECTOR ( 'NONE', #24663, 1000.000000000000000 ) ;
#8940 = CYLINDRICAL_SURFACE ( 'NONE', #21908, 19.99999999999998579 ) ;
#8941 = ORIENTED_EDGE ( 'NONE', *, *, #13862, .T. ) ;
#8942 = ORIENTED_EDGE ( 'NONE', *, *, #25274, .T. ) ;
#8943 = DIRECTION ( 'NONE',  ( -1.000000000000000000, -0.000000000000000000, -0.000000000000000000 ) ) ;
#8944 = DIRECTION ( 'NONE',  ( -1.000000000000000000, 4.524158825347490025E-15, 1.174092375852883357E-15 ) ) ;
#8945 = ORIENTED_EDGE ( 'NONE', *, *, #6811, .F. ) ;
#8946 = DIRECTION ( 'NONE',  ( -1.000000000000000000, 0.000000000000000000, -0.000000000000000000 ) ) ;
#8947 = CIRCLE ( 'NONE', #12407, 19.99999999999998579 ) ;
#8948 = CARTESIAN_POINT ( 'NONE',  ( -34.50000000000000000, -114.1807644833817648, -0.6247823525984269599 ) ) ;
#8949 = LINE ( 'NONE', #17051, #16731 ) ;
#8950 = CARTESIAN_POINT ( 'NONE',  ( -34.50000000000000000, -116.0140978167138712, -0.1247823525984439463 ) ) ;
#8951 = APPLICATION_CONTEXT ( 'automotive_design' ) ;
#8952 = EDGE_CURVE ( 'NONE', #32982, #9372, #6975, .T. ) ;
#8953 = CARTESIAN_POINT ( 'NONE',  ( -34.50000000000000000, -115.9915791193162420, 10.43066258751475139 ) ) ;
#8954 = PLANE ( 'NONE',  #30663 ) ;
#8955 = CARTESIAN_POINT ( 'NONE',  ( 0.000000000000000000, -26.17370628620682638, 39.63700417846155233 ) ) ;
#8956 = CARTESIAN_POINT ( 'NONE',  ( -37.51022648969539119, -114.9929510916434339, 14.11852173794918386 ) ) ;
#8957 = DIRECTION ( 'NONE',  ( 0.000000000000000000, 0.000000000000000000, -1.000000000000000000 ) ) ;
#8958 = DIRECTION ( 'NONE',  ( -1.000000000000000000, 0.000000000000000000, 0.000000000000000000 ) ) ;
#8959 = CARTESIAN_POINT ( 'NONE',  ( 8.000000000000000000, 0.000000000000000000, 0.000000000000000000 ) ) ;
#8960 = CARTESIAN_POINT ( 'NONE',  ( -34.49999999999998579, -9.059673409587547965, 113.4689433211305811 ) ) ;
#8961 = CIRCLE ( 'NONE', #18738, 5.000000000000011546 ) ;
#8962 = ORIENTED_EDGE ( 'NONE', *, *, #18274, .T. ) ;
#8963 = CARTESIAN_POINT ( 'NONE',  ( -26.99999999999999289, 3.122849337825751800E-15, 0.000000000000000000 ) ) ;
#8964 = EDGE_LOOP ( 'NONE', ( #26255, #29726 ) ) ;
#8965 = EDGE_CURVE ( 'NONE', #14457, #17480, #1588, .T. ) ;
#8966 = CARTESIAN_POINT ( 'NONE',  ( -38.30190309005061522, -116.9754527089670546, 6.472274454178449155 ) ) ;
#8967 = AXIS2_PLACEMENT_3D ( 'NONE', #6139, #8294, #13886 ) ;
#8968 = DIRECTION ( 'NONE',  ( 0.000000000000000000, 0.8090169943749490056, -0.5877852522924709167 ) ) ;
#8969 = CIRCLE ( 'NONE', #24492, 20.00000000000001066 ) ;
#8970 = CARTESIAN_POINT ( 'NONE',  ( -35.50000000000000711, -114.9724313160460696, -1.624792769101446765 ) ) ;
#8971 = ORIENTED_EDGE ( 'NONE', *, *, #6529, .T. ) ;
#8972 = VERTEX_POINT ( 'NONE', #34357 ) ;
#8973 = CIRCLE ( 'NONE', #9549, 8.000000000000001776 ) ;
#8974 = CARTESIAN_POINT ( 'NONE',  ( 8.000000000000000000, -12.49559743815785140, 9.169462670380546854 ) ) ;
#8975 = DIRECTION ( 'NONE',  ( -1.000000000000000000, 0.000000000000000000, 0.000000000000000000 ) ) ;
#8976 = VERTEX_POINT ( 'NONE', #28948 ) ;
#8977 = AXIS2_PLACEMENT_3D ( 'NONE', #28169, #33384, #33041 ) ;
#8978 = CIRCLE ( 'NONE', #372, 7.199999999999993072 ) ;
#8979 = CARTESIAN_POINT ( 'NONE',  ( 7.999999999999992895, 0.000000000000000000, 0.000000000000000000 ) ) ;
#8980 = ORIENTED_EDGE ( 'NONE', *, *, #15855, .T. ) ;
#8981 = ORIENTED_EDGE ( 'NONE', *, *, #26888, .F. ) ;
#8982 = CARTESIAN_POINT ( 'NONE',  ( -36.11231047232249836, -115.9754527089670262, 4.277725545821551734 ) ) ;
#8983 =( LENGTH_UNIT ( ) NAMED_UNIT ( * ) SI_UNIT ( .MILLI., .METRE. ) );
#8984 = DIRECTION ( 'NONE',  ( 0.000000000000000000, -1.000000000000000000, -1.049160758270772931E-14 ) ) ;
#8985 = CIRCLE ( 'NONE', #33719, 47.49900000000001654 ) ;
#8986 = ORIENTED_EDGE ( 'NONE', *, *, #10627, .F. ) ;
#8987 = VERTEX_POINT ( 'NONE', #29131 ) ;
#8988 = CARTESIAN_POINT ( 'NONE',  ( -35.50000000000000000, -111.0140978167138570, 0.7189676474015717078 ) ) ;
#8989 = CIRCLE ( 'NONE', #13608, 4.000000000000000000 ) ;
#8990 = DIRECTION ( 'NONE',  ( 0.000000000000000000, 0.000000000000000000, 1.000000000000000000 ) ) ;
#8991 = ORIENTED_EDGE ( 'NONE', *, *, #4036, .T. ) ;
#8992 = CARTESIAN_POINT ( 'NONE',  ( -37.48437500000004263, -114.9929510916434339, 13.11852480586264669 ) ) ;
#8993 = AXIS2_PLACEMENT_3D ( 'NONE', #8963, #3761, #20466 ) ;
#8994 = VECTOR ( 'NONE', #24587, 1000.000000000000000 ) ;
#8995 = EDGE_CURVE ( 'NONE', #6915, #6339, #23539, .T. ) ;
#8996 = CARTESIAN_POINT ( 'NONE',  ( -34.50000000000000000, -114.0000000000003411, 9.500000000000035527 ) ) ;
#8997 = EDGE_CURVE ( 'NONE', #4202, #33867, #20638, .T. ) ;
#8998 = CIRCLE ( 'NONE', #26268, 8.000000000000015987 ) ;
#8999 = FACE_OUTER_BOUND ( 'NONE', #35131, .T. ) ;
#9000 = DIRECTION ( 'NONE',  ( -1.000000000000000000, 0.000000000000000000, 0.000000000000000000 ) ) ;
#9001 = CARTESIAN_POINT ( 'NONE',  ( -36.24999999999983658, -113.9929510916434339, 14.11852480586265024 ) ) ;
#9002 = PLANE ( 'NONE',  #28056 ) ;
#9003 = CIRCLE ( 'NONE', #4993, 3.999999999999996447 ) ;
#9004 = CARTESIAN_POINT ( 'NONE',  ( -35.60016694755736921, -114.9929510916434339, 12.92579853460621209 ) ) ;
#9005 = CIRCLE ( 'NONE', #32585, 10.99999999999999822 ) ;
#9006 = DIRECTION ( 'NONE',  ( 0.000000000000000000, 0.000000000000000000, 1.000000000000000000 ) ) ;
#9007 = DIRECTION ( 'NONE',  ( 0.000000000000000000, 0.000000000000000000, 1.000000000000000000 ) ) ;
#9008 = CARTESIAN_POINT ( 'NONE',  ( -42.49999999999999289, -25.98076211353322051, 84.99999999999992895 ) ) ;
#9009 = VERTEX_POINT ( 'NONE', #13115 ) ;
#9010 = CARTESIAN_POINT ( 'NONE',  ( -37.98402046630260287, -115.9929510916434481, 12.74811950270164296 ) ) ;
#9011 = ORIENTED_EDGE ( 'NONE', *, *, #13734, .T. ) ;
#9012 = EDGE_CURVE ( 'NONE', #31306, #31368, #16489, .T. ) ;
#9013 = DIRECTION ( 'NONE',  ( 0.000000000000000000, 0.9048270524660205760, -0.4257792915650702170 ) ) ;
#9014 = CARTESIAN_POINT ( 'NONE',  ( 0.000000000000000000, 0.000000000000000000, -40.89999999999999858 ) ) ;
#9015 = EDGE_CURVE ( 'NONE', #6495, #5380, #13051, .T. ) ;
#9016 = VECTOR ( 'NONE', #23182, 1000.000000000000000 ) ;
#9017 = EDGE_LOOP ( 'NONE', ( #5341, #22353 ) ) ;
#9018 = FACE_OUTER_BOUND ( 'NONE', #9903, .T. ) ;
#9019 = EDGE_LOOP ( 'NONE', ( #34553, #11709, #7303, #17284 ) ) ;
#9020 = AXIS2_PLACEMENT_3D ( 'NONE', #32667, #5309, #5477 ) ;
#9021 = CARTESIAN_POINT ( 'NONE',  ( -35.50000000000000000, -113.0140978167138712, -0.4997823525984338988 ) ) ;
#9022 = CARTESIAN_POINT ( 'NONE',  ( 50.00005079999999680, 3.872983346207417021, -1.000000000000000000 ) ) ;
#9023 = CARTESIAN_POINT ( 'NONE',  ( -37.88768952767750164, -115.9754527089670262, 1.972274454178448710 ) ) ;
#9024 = ORIENTED_EDGE ( 'NONE', *, *, #10650, .T. ) ;
#9025 = CARTESIAN_POINT ( 'NONE',  ( -35.00000000000000000, -114.0592624029313242, 1.503524454178448710 ) ) ;
#9026 = AXIS2_PLACEMENT_3D ( 'NONE', #26604, #18303, #32348 ) ;
#9027 = AXIS2_PLACEMENT_3D ( 'NONE', #29275, #20779, #29630 ) ;
#9028 = ORIENTED_EDGE ( 'NONE', *, *, #28412, .T. ) ;
#9029 = AXIS2_PLACEMENT_3D ( 'NONE', #5638, #47, #8309 ) ;
#9030 = DIRECTION ( 'NONE',  ( 0.000000000000000000, 0.000000000000000000, 1.000000000000000000 ) ) ;
#9031 = CARTESIAN_POINT ( 'NONE',  ( -35.50000000000000711, -113.0796441757086939, 1.890140615870383956 ) ) ;
#9032 = ORIENTED_EDGE ( 'NONE', *, *, #5838, .F. ) ;
#9033 = ORIENTED_EDGE ( 'NONE', *, *, #33049, .T. ) ;
#9034 = VECTOR ( 'NONE', #23328, 1000.000000000000000 ) ;
#9035 = CARTESIAN_POINT ( 'NONE',  ( -34.97545270896703329, -113.2308352781851539, 7.409774454178451819 ) ) ;
#9036 = ADVANCED_FACE ( 'NONE', ( #23907 ), #10223, .T. ) ;
#9037 =( NAMED_UNIT ( * ) PLANE_ANGLE_UNIT ( ) SI_UNIT ( $, .RADIAN. ) );
#9038 = FACE_OUTER_BOUND ( 'NONE', #30589, .T. ) ;
#9039 = EDGE_LOOP ( 'NONE', ( #15141, #22315, #25655, #23018 ) ) ;
#9040 = VERTEX_POINT ( 'NONE', #10404 ) ;
#9041 = CARTESIAN_POINT ( 'NONE',  ( -34.50000000000000000, -115.0140978167138712, -0.5622823525984408377 ) ) ;
#9042 = CARTESIAN_POINT ( 'NONE',  ( -29.99999999999999645, -26.00000000000000000, 113.9999999999999858 ) ) ;
#9043 = VERTEX_POINT ( 'NONE', #32355 ) ;
#9044 = PRODUCT_DEFINITION_CONTEXT ( 'detailed design', #8951, 'design' ) ;
#9045 = ORIENTED_EDGE ( 'NONE', *, *, #26246, .T. ) ;
#9046 = CYLINDRICAL_SURFACE ( 'NONE', #11446, 47.49900000000001654 ) ;
#9047 = AXIS2_PLACEMENT_3D ( 'NONE', #8565, #35250, #3015 ) ;
#9048 = CIRCLE ( 'NONE', #6175, 17.49900000000001654 ) ;
#9049 = EDGE_CURVE ( 'NONE', #15222, #24982, #7886, .T. ) ;
#9050 = CARTESIAN_POINT ( 'NONE',  ( -37.75185693410092824, -113.9929510916434339, 13.05539834812634759 ) ) ;
#9051 = PLANE ( 'NONE',  #13282 ) ;
#9052 = ADVANCED_FACE ( 'NONE', ( #29489 ), #18127, .F. ) ;
#9053 = CARTESIAN_POINT ( 'NONE',  ( 7.999999999999992895, -39.78933988720095982, -24.98727647985043987 ) ) ;
#9054 = EDGE_CURVE ( 'NONE', #26454, #19047, #13625, .T. ) ;
#9055 = CARTESIAN_POINT ( 'NONE',  ( -34.50000000000000000, -116.0140978167138712, 0.0002176474015577116276 ) ) ;
#9056 = AXIS2_PLACEMENT_3D ( 'NONE', #9069, #6536, #6016 ) ;
#9057 = CARTESIAN_POINT ( 'NONE',  ( -35.50000000000000000, -115.9929510916434481, 10.51175824272318415 ) ) ;
#9058 = CARTESIAN_POINT ( 'NONE',  ( -1.566204647097432900, -6.822536405429440620, 0.000000000000000000 ) ) ;
#9059 = AXIS2_PLACEMENT_3D ( 'NONE', #30779, #2739, #25216 ) ;
#9060 = FACE_OUTER_BOUND ( 'NONE', #24648, .T. ) ;
#9061 = FACE_OUTER_BOUND ( 'NONE', #11005, .T. ) ;
#9062 = CYLINDRICAL_SURFACE ( 'NONE', #15065, 44.99999999999999289 ) ;
#9063 = AXIS2_PLACEMENT_3D ( 'NONE', #13860, #21775, #1688 ) ;
#9064 = CARTESIAN_POINT ( 'NONE',  ( 8.000000000000000000, -9.471478019455027209, -14.71414642875966017 ) ) ;
#9065 = EDGE_CURVE ( 'NONE', #32703, #656, #5622, .T. ) ;
#9066 = VERTEX_POINT ( 'NONE', #19192 ) ;
#9067 = CARTESIAN_POINT ( 'NONE',  ( 0.000000000000000000, -2.710505431213761085E-17, 45.00000000000000000 ) ) ;
#9068 = CARTESIAN_POINT ( 'NONE',  ( 0.000000000000000000, 44.61570720899074161, 14.73072383765644489 ) ) ;
#9069 = CARTESIAN_POINT ( 'NONE',  ( 0.000000000000000000, -2.710505431213761085E-17, -20.99999999999999645 ) ) ;
#9070 = CARTESIAN_POINT ( 'NONE',  ( -34.49999999999998579, -33.73076211353313880, 77.24999999999981526 ) ) ;
#9071 = LINE ( 'NONE', #3867, #26201 ) ;
#9072 = CARTESIAN_POINT ( 'NONE',  ( 5.400000000000015454, -1.000000000000002220, 30.00000000000000000 ) ) ;
#9073 = ORIENTED_EDGE ( 'NONE', *, *, #28700, .F. ) ;
#9074 = DIRECTION ( 'NONE',  ( -1.000000000000000000, 0.000000000000000000, 0.000000000000000000 ) ) ;
#9075 = CARTESIAN_POINT ( 'NONE',  ( 7.999999999999992895, -8.053585752061602321, -46.81126742072033409 ) ) ;
#9076 = DIRECTION ( 'NONE',  ( 0.000000000000000000, 0.6845471059286846183, 0.7289686274214152162 ) ) ;
#9077 = ORIENTED_EDGE ( 'NONE', *, *, #23320, .T. ) ;
#9078 = VERTEX_POINT ( 'NONE', #16127 ) ;
#9079 = CARTESIAN_POINT ( 'NONE',  ( -37.99999999999998579, -114.0592624029313242, 4.746475545821549957 ) ) ;
#9080 = AXIS2_PLACEMENT_3D ( 'NONE', #13322, #21569, #16166 ) ;
#9081 = VERTEX_POINT ( 'NONE', #10572 ) ;
#9082 = AXIS2_PLACEMENT_3D ( 'NONE', #30438, #24851, #177 ) ;
#9083 = ADVANCED_FACE ( 'NONE', ( #8041 ), #5528, .T. ) ;
#9084 = ORIENTED_EDGE ( 'NONE', *, *, #19363, .F. ) ;
#9085 = VERTEX_POINT ( 'NONE', #30191 ) ;
#9086 = CARTESIAN_POINT ( 'NONE',  ( 0.000000000000000000, -30.93515269692089120, -36.04401931830286543 ) ) ;
#9087 = ADVANCED_FACE ( 'NONE', ( #5872 ), #19535, .T. ) ;
#9088 = AXIS2_PLACEMENT_3D ( 'NONE', #32370, #8230, #35269 ) ;
#9089 = CARTESIAN_POINT ( 'NONE',  ( -35.50000000000000711, -114.9724313160460696, -1.624792769101446765 ) ) ;
#9090 = FACE_OUTER_BOUND ( 'NONE', #5688, .T. ) ;
#9091 = ADVANCED_BREP_SHAPE_REPRESENTATION ( '', ( #22543, #21307 ), #35148 ) ;
#9092 = CARTESIAN_POINT ( 'NONE',  ( -35.50000000000000711, -114.9929510916434339, 12.44250253426871033 ) ) ;
#9093 = CYLINDRICAL_SURFACE ( 'NONE', #12606, 52.00000000000000711 ) ;
#9094 = EDGE_CURVE ( 'NONE', #1605, #12650, #27673, .T. ) ;
#9095 = DIRECTION ( 'NONE',  ( -1.000000000000000000, 0.000000000000000000, 0.000000000000000000 ) ) ;
#9096 = ADVANCED_FACE ( 'NONE', ( #30541 ), #13454, .F. ) ;
#9097 = CARTESIAN_POINT ( 'NONE',  ( -34.50000000000000000, -114.9929501463477663, 10.50247632894551231 ) ) ;
#9098 = CYLINDRICAL_SURFACE ( 'NONE', #18554, 3.799999999999999822 ) ;
#9099 = CARTESIAN_POINT ( 'NONE',  ( 7.999999999999992895, 26.17370628620710349, -39.63700417846138890 ) ) ;
#9100 = EDGE_LOOP ( 'NONE', ( #10994, #22771 ) ) ;
#9101 = VECTOR ( 'NONE', #7320, 1000.000000000000000 ) ;
#9102 = CARTESIAN_POINT ( 'NONE',  ( -35.50000000000000000, -114.4680894751352156, 8.562575367713533225 ) ) ;
#9103 = CARTESIAN_POINT ( 'NONE',  ( -35.50000000000000711, -112.0577668799241309, 1.173706424699810569 ) ) ;
#9104 =( NAMED_UNIT ( * ) SI_UNIT ( $, .STERADIAN. ) SOLID_ANGLE_UNIT ( ) );
#9105 = AXIS2_PLACEMENT_3D ( 'NONE', #2393, #13716, #24695 ) ;
#9106 = CARTESIAN_POINT ( 'NONE',  ( 0.000000000000000000, 35.11945359308164427, -38.34871548465979174 ) ) ;
#9107 = AXIS2_PLACEMENT_3D ( 'NONE', #758, #19818, #14432 ) ;
#9108 = DIRECTION ( 'NONE',  ( -1.000000000000000000, 0.000000000000000000, 0.000000000000000000 ) ) ;
#9109 = DIRECTION ( 'NONE',  ( 1.000000000000000000, 0.000000000000000000, 0.000000000000000000 ) ) ;
#9110 = CARTESIAN_POINT ( 'NONE',  ( 55.00000000000000000, 20.00000000000001776, -15.00000000000001421 ) ) ;
#9111 = CARTESIAN_POINT ( 'NONE',  ( 0.000000000000000000, 15.46619997295642079, 1.007799283846740002 ) ) ;
#9112 = ORIENTED_EDGE ( 'NONE', *, *, #25441, .F. ) ;
#9113 = CARTESIAN_POINT ( 'NONE',  ( -38.02454729103295961, -113.6450488405582462, 7.840225545821554398 ) ) ;
#9114 = CARTESIAN_POINT ( 'NONE',  ( -34.49999999999998579, -25.98076211353322051, 84.99999999999992895 ) ) ;
#9115 = DIRECTION ( 'NONE',  ( 0.000000000000000000, -0.4817536741017223179, 0.8763066800438598092 ) ) ;
#9116 = ORIENTED_EDGE ( 'NONE', *, *, #22505, .T. ) ;
#9117 = ORIENTED_EDGE ( 'NONE', *, *, #34427, .T. ) ;
#9118 = LINE ( 'NONE', #8748, #10774 ) ;
#9119 = DIRECTION ( 'NONE',  ( 0.000000000000000000, 0.000000000000000000, -1.000000000000000000 ) ) ;
#9120 = ORIENTED_EDGE ( 'NONE', *, *, #22524, .T. ) ;
#9121 = CARTESIAN_POINT ( 'NONE',  ( -38.30190309005061522, -111.0245472910330022, 5.027725545821551734 ) ) ;
#9122 = ORIENTED_EDGE ( 'NONE', *, *, #29873, .F. ) ;
#9123 = EDGE_CURVE ( 'NONE', #6690, #28558, #29195, .T. ) ;
#9124 = EDGE_CURVE ( 'NONE', #24733, #12890, #410, .T. ) ;
#9125 = FACE_BOUND ( 'NONE', #28178, .T. ) ;
#9126 = DIRECTION ( 'NONE',  ( 0.000000000000000000, -6.938893903907203726E-17, -1.000000000000000000 ) ) ;
#9127 = PRODUCT_CONTEXT ( 'NONE', #5043, 'mechanical' ) ;
#9128 = DIRECTION ( 'NONE',  ( 0.000000000000000000, 0.000000000000000000, -1.000000000000000000 ) ) ;
#9129 = VERTEX_POINT ( 'NONE', #30022 ) ;
#9130 = EDGE_LOOP ( 'NONE', ( #19481, #31487, #1424, #17241 ) ) ;
#9131 = AXIS2_PLACEMENT_3D ( 'NONE', #35367, #32469, #2792 ) ;
#9132 = CARTESIAN_POINT ( 'NONE',  ( -1.600000000000004086, -12.74999999999999822, 0.000000000000000000 ) ) ;
#9133 = CARTESIAN_POINT ( 'NONE',  ( 8.000000000000007105, 9.604183132802424083, -5.908880290975567995 ) ) ;
#9134 =( BOUNDED_SURFACE ( )  B_SPLINE_SURFACE ( 3, 2, ( 
 ( #28651, #31869, #15293, #26306, #20868, #1105, #26122, #1642, #23232, #9373, #6850, #7200, #1455, #12435, #12621, #34047, #15113, #3999, #17823, #34587, #14941, #4541, #15473, #1822, #25949, #12799, #33869, #9195, #2366, #29897, #34764, #7396, #23778, #13337, #35134, #32582, #10087, #35478, #13166, #32058, #27201, #19070, #7916, #29718, #21243, #32237, #21053, #30070, #18368, #5062, #24317, #21417, #35308, #18899, #2001, #13507, #10809, #29369, #12976, #18715, #4714, #15648, #26668, #16357, #16006, #23962, #5239, #21769, #27023, #34957, #18545, #10626, #21583, #10279, #7562, #2541, #16179, #24489, #10456, #5411, #4879 ),
 ( #32765, #8089, #27371, #29546, #2721, #32412, #15824, #26845, #2197, #7731, #24141, #14200, #25202, #4047, #8787, #8446, #21947, #22122, #28078, #5925, #33296, #33462, #523, #16714, #25014, #32943, #11155, #24841, #8264, #5755, #6099, #30943, #16547, #19240, #22474, #3421, #14021, #11336, #22640, #3236, #11672, #33122, #10983, #19586, #14370, #27554, #28249, #337, #19429, #19753, #22302, #33634, #30427, #8966, #167, #25377, #27725, #30765, #2892, #13685, #13856, #30245, #3065, #27891, #8616, #30590, #11504, #19934, #5584, #689, #16887, #17069, #6276, #17244, #24665, #12389, #31124, #23367, #23547, #31298, #25735 ),
 ( #20291, #34368, #31648, #20647, #25911, #15248, #4131, #11848, #6624, #26257, #1065, #22831, #6450, #865, #17421, #28605, #15070, #28422, #6806, #17594, #3957, #14900, #12215, #6983, #3763, #17955, #23192, #31826, #14719, #12034, #7161, #26082, #1238, #23008, #28958, #34185, #9509, #12576, #20468, #4304, #31482, #1413, #17777, #28781, #9690, #1597, #34009, #9333, #14537, #34543, #9861, #20823, #18135, #3589, #25551, #33827, #9151, #20115, #18322, #21727, #10582, #29321, #21533, #26982, #13463, #34722, #2324, #24274, #5012, #21371, #18669, #24103, #15778, #29668, #26797, #15966, #35260, #7351, #18855, #5196, #1774 ),
 ( #4670, #8048, #15599, #10042, #26622, #7686, #10233, #35089, #13296, #24443, #15428, #29854, #7518, #32531, #16135, #12753, #7867, #27154, #21007, #2494, #35429, #21199, #1955, #10760, #32721, #29142, #32192, #4494, #26441, #23731, #2148, #32011, #12931, #23915, #18498, #34909, #29497, #4836, #13124, #10414, #32364, #8397, #19543, #10940, #22258, #11114, #124, #22082, #27683, #11459, #21907, #480, #3022, #11624, #32900, #19201, #22598, #30548, #5709, #8222, #22426, #19378, #30384, #28030, #13981, #33418, #33079, #5880, #16670, #24974, #8573, #16846, #30201, #5537, #30029, #296, #11286, #27851, #3193, #14150, #33255 ),
 ( #16496, #33591, #8740, #27511, #19710, #25154, #3379, #24624, #30725, #6058, #17020, #14325, #25331, #647, #19030, #5367, #16314, #27325, #2850, #2671, #13634, #35611, #13812, #24800, #17918, #34141, #6943, #17375, #6236, #14862, #9649, #22783, #33963, #28913, #17552, #1370, #11998, #20420, #1021, #31256, #9463, #31434, #20070, #11804, #19888, #22963, #9292, #6763, #28740, #17739, #25872, #31081, #1196, #15202, #33786, #1548, #26037, #9113, #12346, #4093, #4262, #14493, #15034, #23321, #34320, #12170, #20608, #3909, #6578, #20247, #31608, #26211, #6408, #17198, #12531, #23507, #28559, #23144, #8924, #30901, #28207 ),
 ( #3547, #28376, #25505, #821, #3720, #14673, #25687, #32993, #31963, #8308, #20963, #13738, #7300, #19117, #23689, #13902, #12712, #4444, #18277, #13077, #15559, #4796, #32816, #19288, #20783, #44, #12891, #27425, #24716, #18091, #30117, #8137, #26396, #5454, #30298, #26578, #29279, #11034, #16406, #2774, #1916, #21996, #5636, #16595, #21153, #27607, #35533, #7118, #23873, #2942, #4625, #29095, #1728, #31784, #34679, #34861, #10859, #10001, #2100, #10184, #32148, #7476, #18455, #34500, #29453, #9820, #15739, #15384, #26757, #24062, #21819, #740, #11553, #16764, #6324, #25245, #17116, #24890, #19986, #924, #30813 ),
 ( #25605, #3288, #17293, #14591, #8501, #9023, #33686, #27775, #30991, #9201, #16933, #11386, #3642, #28298, #11905, #5976, #22882, #33875, #20163, #22521, #31170, #25425, #33170, #27938, #6499, #22347, #19476, #3115, #22171, #14065, #14246, #11722, #25061, #28122, #565, #33512, #8839, #19801, #17474, #387, #28472, #6151, #3819, #33341, #8665, #215, #22693, #3465, #19634, #11199, #14416, #30474, #5806, #30641, #7209, #17829, #26314, #6857, #1462, #4355, #1650, #25955, #17656, #25787, #28829, #4179, #15301, #34595, #12628, #31698, #1280, #7032, #21060, #4005, #7401, #31878, #14949, #18191, #23604, #34771, #20339 ) ),
 .UNSPECIFIED., .T., .F., .F. ) 
 B_SPLINE_SURFACE_WITH_KNOTS ( ( 4, 3, 4 ),
 ( 3, 2, 2, 2, 2, 2, 2, 2, 2, 2, 2, 2, 2, 2, 2, 2, 2, 2, 2, 2, 2, 2, 2, 2, 2, 2, 2, 2, 2, 2, 2, 2, 2, 2, 2, 2, 2, 2, 2, 2, 3 ),
 ( 0.000000000000000000, 0.5000000000000000000, 1.000000000000000000 ),
 ( 0.000000000000000000, 0.02500000000000000139, 0.05000000000000000278, 0.07499999999999999722, 0.1000000000000000056, 0.1250000000000000000, 0.1499999999999999944, 0.1749999999999999889, 0.2000000000000000111, 0.2250000000000000056, 0.2500000000000000000, 0.2750000000000000222, 0.2999999999999999889, 0.3250000000000000111, 0.3499999999999999778, 0.3750000000000000000, 0.4000000000000000222, 0.4249999999999999889, 0.4500000000000000111, 0.4749999999999999778, 0.5000000000000000000, 0.5250000000000000222, 0.5500000000000000444, 0.5749999999999999556, 0.5999999999999999778, 0.6250000000000000000, 0.6500000000000000222, 0.6750000000000000444, 0.6999999999999999556, 0.7249999999999999778, 0.7500000000000000000, 0.7750000000000000222, 0.8000000000000000444, 0.8249999999999999556, 0.8499999999999999778, 0.8750000000000000000, 0.9000000000000000222, 0.9250000000000000444, 0.9499999999999999556, 0.9749999999999999778, 1.000000000000000000 ),
 .UNSPECIFIED. ) 
 GEOMETRIC_REPRESENTATION_ITEM ( )  RATIONAL_B_SPLINE_SURFACE ( (
 ( 1.000000000000000000, 0.9238795325112867385, 1.000000000000000000, 0.9238795325112867385, 1.000000000000000000, 0.9238795325112867385, 1.000000000000000000, 0.9238795325112867385, 1.000000000000000000, 0.9238795325112867385, 1.000000000000000000, 0.9238795325112867385, 1.000000000000000000, 0.9238795325112867385, 1.000000000000000000, 0.9238795325112867385, 1.000000000000000000, 0.9238795325112867385, 1.000000000000000000, 0.9238795325112867385, 1.000000000000000000, 0.9238795325112867385, 1.000000000000000000, 0.9238795325112867385, 1.000000000000000000, 0.9238795325112867385, 1.000000000000000000, 0.9238795325112867385, 1.000000000000000000, 0.9238795325112867385, 1.000000000000000000, 0.9238795325112867385, 1.000000000000000000, 0.9238795325112867385, 1.000000000000000000, 0.9238795325112867385, 1.000000000000000000, 0.9238795325112867385, 1.000000000000000000, 0.9238795325112867385, 1.000000000000000000, 0.9238795325112867385, 1.000000000000000000, 0.9238795325112867385, 1.000000000000000000, 0.9238795325112867385, 1.000000000000000000, 0.9238795325112867385, 1.000000000000000000, 0.9238795325112867385, 1.000000000000000000, 0.9238795325112867385, 1.000000000000000000, 0.9238795325112867385, 1.000000000000000000, 0.9238795325112867385, 1.000000000000000000, 0.9238795325112867385, 1.000000000000000000, 0.9238795325112867385, 1.000000000000000000, 0.9238795325112867385, 1.000000000000000000, 0.9238795325112867385, 1.000000000000000000, 0.9238795325112867385, 1.000000000000000000, 0.9238795325112867385, 1.000000000000000000, 0.9238795325112867385, 1.000000000000000000, 0.9238795325112867385, 1.000000000000000000, 0.9238795325112867385, 1.000000000000000000, 0.9238795325112867385, 1.000000000000000000, 0.9238795325112867385, 1.000000000000000000, 0.9238795325112867385, 1.000000000000000000),
 ( 0.3333333333333333703, 0.3079598441704289313, 0.3333333333333333703, 0.3079598441704289313, 0.3333333333333333703, 0.3079598441704289313, 0.3333333333333333703, 0.3079598441704289313, 0.3333333333333333703, 0.3079598441704289313, 0.3333333333333333703, 0.3079598441704289313, 0.3333333333333333703, 0.3079598441704289313, 0.3333333333333333703, 0.3079598441704289313, 0.3333333333333333703, 0.3079598441704289313, 0.3333333333333333703, 0.3079598441704289313, 0.3333333333333333703, 0.3079598441704289313, 0.3333333333333333703, 0.3079598441704289313, 0.3333333333333333703, 0.3079598441704289313, 0.3333333333333333703, 0.3079598441704289313, 0.3333333333333333703, 0.3079598441704289313, 0.3333333333333333703, 0.3079598441704289313, 0.3333333333333333703, 0.3079598441704289313, 0.3333333333333333703, 0.3079598441704289313, 0.3333333333333333703, 0.3079598441704289313, 0.3333333333333333703, 0.3079598441704289313, 0.3333333333333333703, 0.3079598441704289313, 0.3333333333333333703, 0.3079598441704289313, 0.3333333333333333703, 0.3079598441704289313, 0.3333333333333333703, 0.3079598441704289313, 0.3333333333333333703, 0.3079598441704289313, 0.3333333333333333703, 0.3079598441704289313, 0.3333333333333333703, 0.3079598441704289313, 0.3333333333333333703, 0.3079598441704289313, 0.3333333333333333703, 0.3079598441704289313, 0.3333333333333333703, 0.3079598441704289313, 0.3333333333333333703, 0.3079598441704289313, 0.3333333333333333703, 0.3079598441704289313, 0.3333333333333333703, 0.3079598441704289313, 0.3333333333333333703, 0.3079598441704289313, 0.3333333333333333703, 0.3079598441704289313, 0.3333333333333333703, 0.3079598441704289313, 0.3333333333333333703, 0.3079598441704289313, 0.3333333333333333703, 0.3079598441704289313, 0.3333333333333333703, 0.3079598441704289313, 0.3333333333333333703, 0.3079598441704289313, 0.3333333333333333703),
 ( 0.3333333333333333703, 0.3079598441704289313, 0.3333333333333333703, 0.3079598441704289313, 0.3333333333333333703, 0.3079598441704289313, 0.3333333333333333703, 0.3079598441704289313, 0.3333333333333333703, 0.3079598441704289313, 0.3333333333333333703, 0.3079598441704289313, 0.3333333333333333703, 0.3079598441704289313, 0.3333333333333333703, 0.3079598441704289313, 0.3333333333333333703, 0.3079598441704289313, 0.3333333333333333703, 0.3079598441704289313, 0.3333333333333333703, 0.3079598441704289313, 0.3333333333333333703, 0.3079598441704289313, 0.3333333333333333703, 0.3079598441704289313, 0.3333333333333333703, 0.3079598441704289313, 0.3333333333333333703, 0.3079598441704289313, 0.3333333333333333703, 0.3079598441704289313, 0.3333333333333333703, 0.3079598441704289313, 0.3333333333333333703, 0.3079598441704289313, 0.3333333333333333703, 0.3079598441704289313, 0.3333333333333333703, 0.3079598441704289313, 0.3333333333333333703, 0.3079598441704289313, 0.3333333333333333703, 0.3079598441704289313, 0.3333333333333333703, 0.3079598441704289313, 0.3333333333333333703, 0.3079598441704289313, 0.3333333333333333703, 0.3079598441704289313, 0.3333333333333333703, 0.3079598441704289313, 0.3333333333333333703, 0.3079598441704289313, 0.3333333333333333703, 0.3079598441704289313, 0.3333333333333333703, 0.3079598441704289313, 0.3333333333333333703, 0.3079598441704289313, 0.3333333333333333703, 0.3079598441704289313, 0.3333333333333333703, 0.3079598441704289313, 0.3333333333333333703, 0.3079598441704289313, 0.3333333333333333703, 0.3079598441704289313, 0.3333333333333333703, 0.3079598441704289313, 0.3333333333333333703, 0.3079598441704289313, 0.3333333333333333703, 0.3079598441704289313, 0.3333333333333333703, 0.3079598441704289313, 0.3333333333333333703, 0.3079598441704289313, 0.3333333333333333703, 0.3079598441704289313, 0.3333333333333333703),
 ( 1.000000000000000000, 0.9238795325112867385, 1.000000000000000000, 0.9238795325112867385, 1.000000000000000000, 0.9238795325112867385, 1.000000000000000000, 0.9238795325112867385, 1.000000000000000000, 0.9238795325112867385, 1.000000000000000000, 0.9238795325112867385, 1.000000000000000000, 0.9238795325112867385, 1.000000000000000000, 0.9238795325112867385, 1.000000000000000000, 0.9238795325112867385, 1.000000000000000000, 0.9238795325112867385, 1.000000000000000000, 0.9238795325112867385, 1.000000000000000000, 0.9238795325112867385, 1.000000000000000000, 0.9238795325112867385, 1.000000000000000000, 0.9238795325112867385, 1.000000000000000000, 0.9238795325112867385, 1.000000000000000000, 0.9238795325112867385, 1.000000000000000000, 0.9238795325112867385, 1.000000000000000000, 0.9238795325112867385, 1.000000000000000000, 0.9238795325112867385, 1.000000000000000000, 0.9238795325112867385, 1.000000000000000000, 0.9238795325112867385, 1.000000000000000000, 0.9238795325112867385, 1.000000000000000000, 0.9238795325112867385, 1.000000000000000000, 0.9238795325112867385, 1.000000000000000000, 0.9238795325112867385, 1.000000000000000000, 0.9238795325112867385, 1.000000000000000000, 0.9238795325112867385, 1.000000000000000000, 0.9238795325112867385, 1.000000000000000000, 0.9238795325112867385, 1.000000000000000000, 0.9238795325112867385, 1.000000000000000000, 0.9238795325112867385, 1.000000000000000000, 0.9238795325112867385, 1.000000000000000000, 0.9238795325112867385, 1.000000000000000000, 0.9238795325112867385, 1.000000000000000000, 0.9238795325112867385, 1.000000000000000000, 0.9238795325112867385, 1.000000000000000000, 0.9238795325112867385, 1.000000000000000000, 0.9238795325112867385, 1.000000000000000000, 0.9238795325112867385, 1.000000000000000000, 0.9238795325112867385, 1.000000000000000000),
 ( 0.3333333333333333703, 0.3079598441704289313, 0.3333333333333333703, 0.3079598441704289313, 0.3333333333333333703, 0.3079598441704289313, 0.3333333333333333703, 0.3079598441704289313, 0.3333333333333333703, 0.3079598441704289313, 0.3333333333333333703, 0.3079598441704289313, 0.3333333333333333703, 0.3079598441704289313, 0.3333333333333333703, 0.3079598441704289313, 0.3333333333333333703, 0.3079598441704289313, 0.3333333333333333703, 0.3079598441704289313, 0.3333333333333333703, 0.3079598441704289313, 0.3333333333333333703, 0.3079598441704289313, 0.3333333333333333703, 0.3079598441704289313, 0.3333333333333333703, 0.3079598441704289313, 0.3333333333333333703, 0.3079598441704289313, 0.3333333333333333703, 0.3079598441704289313, 0.3333333333333333703, 0.3079598441704289313, 0.3333333333333333703, 0.3079598441704289313, 0.3333333333333333703, 0.3079598441704289313, 0.3333333333333333703, 0.3079598441704289313, 0.3333333333333333703, 0.3079598441704289313, 0.3333333333333333703, 0.3079598441704289313, 0.3333333333333333703, 0.3079598441704289313, 0.3333333333333333703, 0.3079598441704289313, 0.3333333333333333703, 0.3079598441704289313, 0.3333333333333333703, 0.3079598441704289313, 0.3333333333333333703, 0.3079598441704289313, 0.3333333333333333703, 0.3079598441704289313, 0.3333333333333333703, 0.3079598441704289313, 0.3333333333333333703, 0.3079598441704289313, 0.3333333333333333703, 0.3079598441704289313, 0.3333333333333333703, 0.3079598441704289313, 0.3333333333333333703, 0.3079598441704289313, 0.3333333333333333703, 0.3079598441704289313, 0.3333333333333333703, 0.3079598441704289313, 0.3333333333333333703, 0.3079598441704289313, 0.3333333333333333703, 0.3079598441704289313, 0.3333333333333333703, 0.3079598441704289313, 0.3333333333333333703, 0.3079598441704289313, 0.3333333333333333703, 0.3079598441704289313, 0.3333333333333333703),
 ( 0.3333333333333333703, 0.3079598441704289313, 0.3333333333333333703, 0.3079598441704289313, 0.3333333333333333703, 0.3079598441704289313, 0.3333333333333333703, 0.3079598441704289313, 0.3333333333333333703, 0.3079598441704289313, 0.3333333333333333703, 0.3079598441704289313, 0.3333333333333333703, 0.3079598441704289313, 0.3333333333333333703, 0.3079598441704289313, 0.3333333333333333703, 0.3079598441704289313, 0.3333333333333333703, 0.3079598441704289313, 0.3333333333333333703, 0.3079598441704289313, 0.3333333333333333703, 0.3079598441704289313, 0.3333333333333333703, 0.3079598441704289313, 0.3333333333333333703, 0.3079598441704289313, 0.3333333333333333703, 0.3079598441704289313, 0.3333333333333333703, 0.3079598441704289313, 0.3333333333333333703, 0.3079598441704289313, 0.3333333333333333703, 0.3079598441704289313, 0.3333333333333333703, 0.3079598441704289313, 0.3333333333333333703, 0.3079598441704289313, 0.3333333333333333703, 0.3079598441704289313, 0.3333333333333333703, 0.3079598441704289313, 0.3333333333333333703, 0.3079598441704289313, 0.3333333333333333703, 0.3079598441704289313, 0.3333333333333333703, 0.3079598441704289313, 0.3333333333333333703, 0.3079598441704289313, 0.3333333333333333703, 0.3079598441704289313, 0.3333333333333333703, 0.3079598441704289313, 0.3333333333333333703, 0.3079598441704289313, 0.3333333333333333703, 0.3079598441704289313, 0.3333333333333333703, 0.3079598441704289313, 0.3333333333333333703, 0.3079598441704289313, 0.3333333333333333703, 0.3079598441704289313, 0.3333333333333333703, 0.3079598441704289313, 0.3333333333333333703, 0.3079598441704289313, 0.3333333333333333703, 0.3079598441704289313, 0.3333333333333333703, 0.3079598441704289313, 0.3333333333333333703, 0.3079598441704289313, 0.3333333333333333703, 0.3079598441704289313, 0.3333333333333333703, 0.3079598441704289313, 0.3333333333333333703),
 ( 1.000000000000000000, 0.9238795325112867385, 1.000000000000000000, 0.9238795325112867385, 1.000000000000000000, 0.9238795325112867385, 1.000000000000000000, 0.9238795325112867385, 1.000000000000000000, 0.9238795325112867385, 1.000000000000000000, 0.9238795325112867385, 1.000000000000000000, 0.9238795325112867385, 1.000000000000000000, 0.9238795325112867385, 1.000000000000000000, 0.9238795325112867385, 1.000000000000000000, 0.9238795325112867385, 1.000000000000000000, 0.9238795325112867385, 1.000000000000000000, 0.9238795325112867385, 1.000000000000000000, 0.9238795325112867385, 1.000000000000000000, 0.9238795325112867385, 1.000000000000000000, 0.9238795325112867385, 1.000000000000000000, 0.9238795325112867385, 1.000000000000000000, 0.9238795325112867385, 1.000000000000000000, 0.9238795325112867385, 1.000000000000000000, 0.9238795325112867385, 1.000000000000000000, 0.9238795325112867385, 1.000000000000000000, 0.9238795325112867385, 1.000000000000000000, 0.9238795325112867385, 1.000000000000000000, 0.9238795325112867385, 1.000000000000000000, 0.9238795325112867385, 1.000000000000000000, 0.9238795325112867385, 1.000000000000000000, 0.9238795325112867385, 1.000000000000000000, 0.9238795325112867385, 1.000000000000000000, 0.9238795325112867385, 1.000000000000000000, 0.9238795325112867385, 1.000000000000000000, 0.9238795325112867385, 1.000000000000000000, 0.9238795325112867385, 1.000000000000000000, 0.9238795325112867385, 1.000000000000000000, 0.9238795325112867385, 1.000000000000000000, 0.9238795325112867385, 1.000000000000000000, 0.9238795325112867385, 1.000000000000000000, 0.9238795325112867385, 1.000000000000000000, 0.9238795325112867385, 1.000000000000000000, 0.9238795325112867385, 1.000000000000000000, 0.9238795325112867385, 1.000000000000000000, 0.9238795325112867385, 1.000000000000000000) ) ) 
 REPRESENTATION_ITEM ( '' )  SURFACE ( )  );
#9135 = EDGE_LOOP ( 'NONE', ( #32880, #2929, #23600, #22125 ) ) ;
#9136 = DIRECTION ( 'NONE',  ( -1.000000000000000000, 0.000000000000000000, 0.000000000000000000 ) ) ;
#9137 = CARTESIAN_POINT ( 'NONE',  ( -34.50000000000000000, -115.0140978167143402, -0.6247823525984417259 ) ) ;
#9138 = CARTESIAN_POINT ( 'NONE',  ( 6.071532165918824830E-15, 1.000000000000000000, -30.00000000000000000 ) ) ;
#9139 = DIRECTION ( 'NONE',  ( 0.000000000000000000, 0.000000000000000000, 1.000000000000000000 ) ) ;
#9140 = CARTESIAN_POINT ( 'NONE',  ( -34.50000000000000000, -115.3279708130221479, 8.997521329298534098 ) ) ;
#9141 = LINE ( 'NONE', #6265, #24937 ) ;
#9142 = CARTESIAN_POINT ( 'NONE',  ( -38.45611840935523418, -115.3723087153909432, 2.066024454178448710 ) ) ;
#9143 = CARTESIAN_POINT ( 'NONE',  ( -34.50000000000000000, -114.2253558743059330, 8.519800927820798009 ) ) ;
#9144 = CARTESIAN_POINT ( 'NONE',  ( 39.30000000000000426, 7.219292880973646134E-15, 0.000000000000000000 ) ) ;
#9145 = DIRECTION ( 'NONE',  ( -0.000000000000000000, 0.000000000000000000, -1.000000000000000000 ) ) ;
#9146 = CYLINDRICAL_SURFACE ( 'NONE', #11830, 52.00000000000000711 ) ;
#9147 = DIRECTION ( 'NONE',  ( -1.000000000000000000, 0.000000000000000000, 0.000000000000000000 ) ) ;
#9148 = ORIENTED_EDGE ( 'NONE', *, *, #14940, .F. ) ;
#9149 = DIRECTION ( 'NONE',  ( 0.000000000000000000, 0.000000000000000000, 1.000000000000000000 ) ) ;
#9150 = ORIENTED_EDGE ( 'NONE', *, *, #23606, .F. ) ;
#9151 = CARTESIAN_POINT ( 'NONE',  ( -39.99999999999999289, -114.0592624029313242, 7.746475545821553510 ) ) ;
#9152 = CARTESIAN_POINT ( 'NONE',  ( 10.50000000000000178, -7.127471650355116251E-32, -1.200000000000006617 ) ) ;
#9153 = CARTESIAN_POINT ( 'NONE',  ( -35.50000000000000711, -116.0140978167138712, -0.5622823525984409487 ) ) ;
#9154 = ORIENTED_EDGE ( 'NONE', *, *, #9253, .T. ) ;
#9155 = VECTOR ( 'NONE', #7416, 1000.000000000000000 ) ;
#9156 = VERTEX_POINT ( 'NONE', #10932 ) ;
#9157 = DIRECTION ( 'NONE',  ( -1.000000000000000000, -0.000000000000000000, 0.000000000000000000 ) ) ;
#9158 = CARTESIAN_POINT ( 'NONE',  ( 8.000000000000000000, 4.460989585140964664, 16.92083251265327348 ) ) ;
#9159 = ORIENTED_EDGE ( 'NONE', *, *, #23573, .T. ) ;
#9160 = ORIENTED_EDGE ( 'NONE', *, *, #18073, .T. ) ;
#9161 = CIRCLE ( 'NONE', #13778, 47.49900000000001654 ) ;
#9162 = EDGE_CURVE ( 'NONE', #1256, #4012, #11274, .T. ) ;
#9163 = CARTESIAN_POINT ( 'NONE',  ( 0.000000000000000000, 10.62435788049443808, 13.16139124467922272 ) ) ;
#9164 = ORIENTED_EDGE ( 'NONE', *, *, #2909, .F. ) ;
#9165 = ORIENTED_EDGE ( 'NONE', *, *, #5090, .T. ) ;
#9166 = CARTESIAN_POINT ( 'NONE',  ( -37.76916472181486739, -116.0245472910329880, 7.465225545821551734 ) ) ;
#9167 = DIRECTION ( 'NONE',  ( 0.000000000000000000, 0.000000000000000000, 1.000000000000000000 ) ) ;
#9168 = LINE ( 'NONE', #20132, #23642 ) ;
#9169 = VERTEX_POINT ( 'NONE', #27317 ) ;
#9170 = EDGE_LOOP ( 'NONE', ( #9922, #6412, #7168, #12046 ) ) ;
#9171 = CARTESIAN_POINT ( 'NONE',  ( -35.50000000000000000, -113.0974311500471714, -2.624782352598442614 ) ) ;
#9172 = APPLICATION_CONTEXT ( 'automotive_design' ) ;
#9173 = EDGE_CURVE ( 'NONE', #12368, #32016, #21689, .T. ) ;
#9174 = DIRECTION ( 'NONE',  ( 0.000000000000000000, -1.000000000000000000, 0.000000000000000000 ) ) ;
#9175 = ORIENTED_EDGE ( 'NONE', *, *, #25127, .F. ) ;
#9176 = CARTESIAN_POINT ( 'NONE',  ( -37.99599240977853754, -114.9929510916434339, 12.68378527132499478 ) ) ;
#9177 = CIRCLE ( 'NONE', #13212, 11.00000000000000000 ) ;
#9178 = CARTESIAN_POINT ( 'NONE',  ( -39.00000000000000000, -113.9929510916434339, 12.53051367006571937 ) ) ;
#9179 = DIRECTION ( 'NONE',  ( 0.000000000000000000, 0.000000000000000000, 1.000000000000000000 ) ) ;
#9180 = FACE_OUTER_BOUND ( 'NONE', #32829, .T. ) ;
#9181 =( GEOMETRIC_REPRESENTATION_CONTEXT ( 3 ) GLOBAL_UNCERTAINTY_ASSIGNED_CONTEXT ( ( #20058 ) ) GLOBAL_UNIT_ASSIGNED_CONTEXT ( ( #24441, #21903, #5534 ) ) REPRESENTATION_CONTEXT ( 'NONE', 'WORKASPACE' ) );
#9182 = CYLINDRICAL_SURFACE ( 'NONE', #10032, 20.00000000000000355 ) ;
#9183 = CARTESIAN_POINT ( 'NONE',  ( -38.42182118622945808, -113.9929510916434339, 13.81802396319329773 ) ) ;
#9185 = DIRECTION ( 'NONE',  ( 0.000000000000000000, 0.8443279255020126328, 0.5358267949790005424 ) ) ;
#9184 = CIRCLE ( 'NONE', #5210, 4.000000000000014211 ) ;
#9186 = CARTESIAN_POINT ( 'NONE',  ( -35.50025087934803736, -114.9929510916434339, 12.63488142334835196 ) ) ;
#9187 = FACE_OUTER_BOUND ( 'NONE', #2718, .T. ) ;
#9188 = ORIENTED_EDGE ( 'NONE', *, *, #12717, .F. ) ;
#9189 = CARTESIAN_POINT ( 'NONE',  ( 0.000000000000000000, 0.000000000000000000, 55.00000000000000000 ) ) ;
#9190 = DIRECTION ( 'NONE',  ( 0.000000000000000000, 1.000000000000000000, 0.000000000000000000 ) ) ;
#9191 = ORIENTED_EDGE ( 'NONE', *, *, #15817, .F. ) ;
#9192 = CARTESIAN_POINT ( 'NONE',  ( -35.50000000000000711, -114.9929510916434339, 12.50851088611648088 ) ) ;
#9193 = ORIENTED_EDGE ( 'NONE', *, *, #22096, .T. ) ;
#9194 = DIRECTION ( 'NONE',  ( -1.000000000000000000, 0.000000000000000000, 0.000000000000000000 ) ) ;
#9195 = CARTESIAN_POINT ( 'NONE',  ( -37.76916472181487450, -111.9754527089670404, 4.034774454178449155 ) ) ;
#9196 = ORIENTED_EDGE ( 'NONE', *, *, #12339, .T. ) ;
#9197 = LINE ( 'NONE', #33506, #29698 ) ;
#9198 = EDGE_LOOP ( 'NONE', ( #17887, #18571, #32648, #1417, #9077, #32506, #25376, #24844, #35228, #32942, #27728, #33471, #6991, #31836, #3650, #13911 ) ) ;
#9199 = CARTESIAN_POINT ( 'NONE',  ( -34.50000000000000000, -114.1185248058627053, 1.007048908356900085 ) ) ;
#9200 = CARTESIAN_POINT ( 'NONE',  ( 3.799999999999999378, -1.702292157117525034E-14, 4.461551028240974192E-15 ) ) ;
#9201 = CARTESIAN_POINT ( 'NONE',  ( -38.97545270896704039, -113.1123104723225197, 2.347274454178448710 ) ) ;
#9202 = VECTOR ( 'NONE', #29259, 1000.000000000000000 ) ;
#9203 = VERTEX_POINT ( 'NONE', #24965 ) ;
#9204 = CARTESIAN_POINT ( 'NONE',  ( -35.00000000000000000, -114.0592624029313242, 3.003524454178448710 ) ) ;
#9205 = AXIS2_PLACEMENT_3D ( 'NONE', #16827, #28185, #11441 ) ;
#9206 = DIRECTION ( 'NONE',  ( -0.9995917534020514195, -0.02857142857143298367, 1.161550059124387962E-15 ) ) ;
#9207 = EDGE_CURVE ( 'NONE', #12104, #24884, #4473, .T. ) ;
#9208 = CARTESIAN_POINT ( 'NONE',  ( -35.50000000000000711, -112.0460568841087223, -0.8839717462762063382 ) ) ;
#9209 = ORIENTED_EDGE ( 'NONE', *, *, #33270, .T. ) ;
#9210 = VERTEX_POINT ( 'NONE', #32893 ) ;
#9211 = EDGE_CURVE ( 'NONE', #24982, #15222, #5030, .T. ) ;
#9212 = CARTESIAN_POINT ( 'NONE',  ( -39.49999999999999289, -13.10640646055107084, 90.70096189432331357 ) ) ;
#9213 = VECTOR ( 'NONE', #3864, 1000.000000000000000 ) ;
#9214 = VECTOR ( 'NONE', #17484, 1000.000000000000000 ) ;
#9215 = ITEM_DEFINED_TRANSFORMATION ( 'NONE', 'NONE', #27665,  #21307 ) ;
#9216 = DIRECTION ( 'NONE',  ( 0.000000000000000000, 0.000000000000000000, -1.000000000000000000 ) ) ;
#9217 = ORIENTED_EDGE ( 'NONE', *, *, #21129, .T. ) ;
#9218 = ORIENTED_EDGE ( 'NONE', *, *, #30407, .T. ) ;
#9219 = CARTESIAN_POINT ( 'NONE',  ( -34.50000000000000000, -112.2144317118258527, -1.239329810084414341 ) ) ;
#9220 = CARTESIAN_POINT ( 'NONE',  ( -35.50000000000000711, -112.0140978167138712, 0.5627176474015717078 ) ) ;
#9221 = PRODUCT_DEFINITION_SHAPE ( 'NONE', 'NONE',  #35629 ) ;
#9222 = ADVANCED_FACE ( 'NONE', ( #33068 ), #33245, .T. ) ;
#9223 = ORIENTED_EDGE ( 'NONE', *, *, #16151, .F. ) ;
#9224 = ORIENTED_EDGE ( 'NONE', *, *, #5332, .T. ) ;
#9225 = DIRECTION ( 'NONE',  ( -1.000000000000000000, 0.000000000000000000, 0.000000000000000000 ) ) ;
#9226 = CARTESIAN_POINT ( 'NONE',  ( -35.87040530316090070, -113.9929510916434339, 13.10254527216545917 ) ) ;
#9227 = CARTESIAN_POINT ( 'NONE',  ( -34.50000000000000000, -114.0000000000000853, 2.000000000000001776 ) ) ;
#9228 = CIRCLE ( 'NONE', #29374, 4.725000000000016520 ) ;
#9229 = DIRECTION ( 'NONE',  ( -1.000000000000000000, -0.000000000000000000, -0.000000000000000000 ) ) ;
#9230 = CARTESIAN_POINT ( 'NONE',  ( -36.06250000000000711, -113.9929510916434339, 13.11852480586264846 ) ) ;
#9231 = CARTESIAN_POINT ( 'NONE',  ( -35.50000000000000000, -115.9929510916434481, 11.91443571948720148 ) ) ;
#9232 = UNCERTAINTY_MEASURE_WITH_UNIT (LENGTH_MEASURE( 1.000000000000000082E-05 ), #1733, 'distance_accuracy_value', 'NONE');
#9233 = DIRECTION ( 'NONE',  ( -1.000000000000000000, 0.000000000000000000, 0.000000000000000000 ) ) ;
#9234 = AXIS2_PLACEMENT_3D ( 'NONE', #18128, #29314, #32357 ) ;
#9235 = FACE_OUTER_BOUND ( 'NONE', #26695, .T. ) ;
#9236 = AXIS2_PLACEMENT_3D ( 'NONE', #28869, #1873, #31915 ) ;
#9237 =( GEOMETRIC_REPRESENTATION_CONTEXT ( 3 ) GLOBAL_UNCERTAINTY_ASSIGNED_CONTEXT ( ( #31195 ) ) GLOBAL_UNIT_ASSIGNED_CONTEXT ( ( #14468, #8897, #3350 ) ) REPRESENTATION_CONTEXT ( 'NONE', 'WORKASPACE' ) );
#9238 = CYLINDRICAL_SURFACE ( 'NONE', #35545, 7.199999999999993960 ) ;
#9239 = DIRECTION ( 'NONE',  ( -1.000000000000000000, 0.000000000000000000, 0.000000000000000000 ) ) ;
#9240 = AXIS2_PLACEMENT_3D ( 'NONE', #2743, #27390, #18915 ) ;
#9241 = CARTESIAN_POINT ( 'NONE',  ( 8.000000000000007105, -5.679790370315976666, -7.613867765417642097 ) ) ;
#9242 = EDGE_CURVE ( 'NONE', #29785, #6500, #25145, .T. ) ;
#9243 = AXIS2_PLACEMENT_3D ( 'NONE', #32207, #26813, #10597 ) ;
#9244 = ORIENTED_EDGE ( 'NONE', *, *, #33270, .F. ) ;
#9245 = PLANE ( 'NONE',  #11658 ) ;
#9246 = CARTESIAN_POINT ( 'NONE',  ( 0.000000000000000000, 47.00885577955413908, 6.806061952192451692 ) ) ;
#9247 = CARTESIAN_POINT ( 'NONE',  ( 0.000000000000000000, 0.000000000000000000, -50.00000000000000000 ) ) ;
#9248 = CARTESIAN_POINT ( 'NONE',  ( 55.00000000000000000, 6.123233995736780087E-16, 5.000000000000011546 ) ) ;
#9249 = CARTESIAN_POINT ( 'NONE',  ( 0.000000000000000000, 0.000000000000000000, 0.000000000000000000 ) ) ;
#9250 = DIRECTION ( 'NONE',  ( 1.000000000000000000, -0.000000000000000000, 0.000000000000000000 ) ) ;
#9251 = ORIENTED_EDGE ( 'NONE', *, *, #1087, .T. ) ;
#9252 = DIRECTION ( 'NONE',  ( 0.000000000000000000, 0.000000000000000000, 1.000000000000000000 ) ) ;
#9253 = EDGE_CURVE ( 'NONE', #7877, #12138, #10751, .T. ) ;
#9254 = CARTESIAN_POINT ( 'NONE',  ( -34.50000000000000000, -115.6584342456100671, -2.522673865603758614 ) ) ;
#9255 = FACE_OUTER_BOUND ( 'NONE', #27517, .T. ) ;
#9256 = ORIENTED_EDGE ( 'NONE', *, *, #1089, .F. ) ;
#9257 = ORIENTED_EDGE ( 'NONE', *, *, #31533, .F. ) ;
#9258 = EDGE_CURVE ( 'NONE', #17886, #15170, #23419, .T. ) ;
#9259 = CARTESIAN_POINT ( 'NONE',  ( -35.97545270896702618, -113.6450488405582604, 4.409774454178449155 ) ) ;
#9260 = ADVANCED_FACE ( 'NONE', ( #3537 ), #14663, .T. ) ;
#9261 = ORIENTED_EDGE ( 'NONE', *, *, #14136, .F. ) ;
#9262 = ORIENTED_EDGE ( 'NONE', *, *, #32174, .T. ) ;
#9263 = ORIENTED_EDGE ( 'NONE', *, *, #16971, .T. ) ;
#9264 = DIRECTION ( 'NONE',  ( 0.000000000000000000, -1.000000000000000000, -0.000000000000000000 ) ) ;
#9265 = EDGE_CURVE ( 'NONE', #26405, #26937, #13659, .T. ) ;
#9266 = VECTOR ( 'NONE', #22881, 1000.000000000000000 ) ;
#9267 = AXIS2_PLACEMENT_3D ( 'NONE', #1080, #25924, #6643 ) ;
#9268 = CARTESIAN_POINT ( 'NONE',  ( -39.49999999999999289, -12.31102132296306451, 91.73752798680880005 ) ) ;
#9269 = EDGE_CURVE ( 'NONE', #12261, #18157, #12223, .T. ) ;
#9270 = DIRECTION ( 'NONE',  ( 0.000000000000000000, 0.000000000000000000, 1.000000000000000000 ) ) ;
#9271 = CARTESIAN_POINT ( 'NONE',  ( -35.69272627125609176, -114.9929510916434339, 13.01835785830562209 ) ) ;
#9272 = DIRECTION ( 'NONE',  ( 1.000000000000000000, -5.339440136655842133E-16, -1.047965281155519420E-16 ) ) ;
#9273 = DIRECTION ( 'NONE',  ( 0.000000000000000000, 0.000000000000000000, 1.000000000000000000 ) ) ;
#9274 = CARTESIAN_POINT ( 'NONE',  ( -34.50000000000000000, -114.9929510916434339, 10.68227981832981044 ) ) ;
#9275 = DIRECTION ( 'NONE',  ( -1.783119874454246424E-31, -1.187911941725854497E-31, 1.000000000000000000 ) ) ;
#9276 = CARTESIAN_POINT ( 'NONE',  ( 0.000000000000000000, -1.000000000000001554, -30.00000000000000000 ) ) ;
#9277 = VERTEX_POINT ( 'NONE', #34669 ) ;
#9278 = CARTESIAN_POINT ( 'NONE',  ( -35.50000000000000000, -114.7000328234681206, 8.631511418192262752 ) ) ;
#9279 = CARTESIAN_POINT ( 'NONE',  ( -35.50000000000000711, -113.0106174888879877, 1.881901162060937827 ) ) ;
#9280 = CARTESIAN_POINT ( 'NONE',  ( -44.00000000000000711, 45.00000000000000000, 5.510910596163089556E-15 ) ) ;
#9281 = CARTESIAN_POINT ( 'NONE',  ( 7.999999999999992895, 0.000000000000000000, 0.000000000000000000 ) ) ;
#9282 = EDGE_CURVE ( 'NONE', #28214, #20788, #9990, .T. ) ;
#9283 = DIRECTION ( 'NONE',  ( 1.000000000000000000, -0.000000000000000000, -0.000000000000000000 ) ) ;
#9284 = CARTESIAN_POINT ( 'NONE',  ( 70.00000000000001421, 75.33903961282865680, 25.84872029956372685 ) ) ;
#9285 = FACE_OUTER_BOUND ( 'NONE', #33390, .T. ) ;
#9286 = EDGE_CURVE ( 'NONE', #24979, #1452, #24000, .T. ) ;
#9287 = CARTESIAN_POINT ( 'NONE',  ( 0.000000000000000000, 13.24207120356965461, 14.98824707027445768 ) ) ;
#9288 = DIRECTION ( 'NONE',  ( -1.000000000000000000, 0.000000000000000000, 0.000000000000000000 ) ) ;
#9289 = VERTEX_POINT ( 'NONE', #21317 ) ;
#9291 = ADVANCED_FACE ( 'NONE', ( #32311 ), #26567, .T. ) ;
#9290 = VECTOR ( 'NONE', #1849, 1000.000000000000000 ) ;
#9292 = CARTESIAN_POINT ( 'NONE',  ( -36.33479806579560289, -113.2509883718313262, 6.808975545821551734 ) ) ;
#9293 = VECTOR ( 'NONE', #9128, 1000.000000000000000 ) ;
#9294 = CYLINDRICAL_SURFACE ( 'NONE', #23287, 13.99999999999999822 ) ;
#9295 = DIRECTION ( 'NONE',  ( 1.541976423090495140E-16, -1.000000000000000000, 0.000000000000000000 ) ) ;
#9296 = VERTEX_POINT ( 'NONE', #21141 ) ;
#9297 = ORIENTED_EDGE ( 'NONE', *, *, #19670, .T. ) ;
#9298 = PRESENTATION_STYLE_ASSIGNMENT (( #15208 ) ) ;
#9299 = DIRECTION ( 'NONE',  ( -1.000000000000000000, 0.000000000000000000, 0.000000000000000000 ) ) ;
#9300 = ORIENTED_EDGE ( 'NONE', *, *, #1342, .T. ) ;
#9301 = EDGE_CURVE ( 'NONE', #17256, #31962, #6174, .T. ) ;
#9302 = CARTESIAN_POINT ( 'NONE',  ( -35.69809690994941320, -116.9754527089670546, 2.777725545821551734 ) ) ;
#9303 = EDGE_CURVE ( 'NONE', #1167, #3384, #5317, .T. ) ;
#9304 = VERTEX_POINT ( 'NONE', #11233 ) ;
#9305 = CIRCLE ( 'NONE', #9886, 4.800000000000000711 ) ;
#9306 = DIRECTION ( 'NONE',  ( 1.000000000000000000, 0.000000000000000000, 0.000000000000000000 ) ) ;
#9307 = DIRECTION ( 'NONE',  ( -1.000000000000000000, 0.000000000000000000, -0.000000000000000000 ) ) ;
#9308 = PRODUCT_CONTEXT ( 'NONE', #8023, 'mechanical' ) ;
#9309 = ADVANCED_FACE ( 'NONE', ( #30149 ), #13936, .T. ) ;
#9310 = CARTESIAN_POINT ( 'NONE',  ( -1.498621416870293821, 0.000000000000000000, 0.000000000000000000 ) ) ;
#9311 = VERTEX_POINT ( 'NONE', #22202 ) ;
#9312 = VERTEX_POINT ( 'NONE', #16441 ) ;
#9313 = DIRECTION ( 'NONE',  ( 0.000000000000000000, -6.938893903907228378E-15, 1.000000000000000000 ) ) ;
#9314 = FACE_BOUND ( 'NONE', #11516, .T. ) ;
#9315 = EDGE_LOOP ( 'NONE', ( #15933, #15471, #33876, #33302 ) ) ;
#9316 = CIRCLE ( 'NONE', #24848, 4.000000000000000000 ) ;
#9317 = FACE_OUTER_BOUND ( 'NONE', #23780, .T. ) ;
#9318 = CARTESIAN_POINT ( 'NONE',  ( -34.50000000000000000, -112.7472371723319355, 1.839427296857320648 ) ) ;
#9319 = DIRECTION ( 'NONE',  ( -1.000000000000000000, -0.000000000000000000, -0.000000000000000000 ) ) ;
#9320 = DIRECTION ( 'NONE',  ( -1.047965281155515106E-16, 6.938893903907203726E-17, 1.000000000000000000 ) ) ;
#9321 = CARTESIAN_POINT ( 'NONE',  ( -34.50000000000000000, -115.9929510916434481, 10.72628538622835670 ) ) ;
#9322 = CARTESIAN_POINT ( 'NONE',  ( -3.160591952521663028, -3.281206521718052382, -0.7999999999999951594 ) ) ;
#9323 = CARTESIAN_POINT ( 'NONE',  ( -35.00000000000000000, -114.0592624029313953, 1.503524454178449599 ) ) ;
#9324 = CARTESIAN_POINT ( 'NONE',  ( -37.49023442168701337, -114.9929510916434339, 14.11852773550420359 ) ) ;
#9325 = LINE ( 'NONE', #28241, #2732 ) ;
#9326 = EDGE_CURVE ( 'NONE', #23698, #17749, #4959, .T. ) ;
#9327 = FACE_OUTER_BOUND ( 'NONE', #15946, .T. ) ;
#9328 = CARTESIAN_POINT ( 'NONE',  ( 2.321707774797385326, -4.824281976788927118, 0.000000000000000000 ) ) ;
#9329 = CARTESIAN_POINT ( 'NONE',  ( 8.000000000000000000, 16.53603053422211389, 8.931325931664652273 ) ) ;
#9330 = ADVANCED_FACE ( 'NONE', ( #13582 ), #8170, .T. ) ;
#9331 = DIRECTION ( 'NONE',  ( 0.000000000000000000, 0.000000000000000000, -1.000000000000000000 ) ) ;
#9332 = ORIENTED_EDGE ( 'NONE', *, *, #4442, .F. ) ;
#9333 = CARTESIAN_POINT ( 'NONE',  ( -34.02454729103297382, -112.6980969099494132, 6.902725545821551734 ) ) ;
#9334 = CARTESIAN_POINT ( 'NONE',  ( 0.000000000000000000, 14.18878633068169925, -6.236773481717946765 ) ) ;
#9335 = CARTESIAN_POINT ( 'NONE',  ( -35.50000000000000000, -113.0140978167136581, 0.8752176474015690433 ) ) ;
#9336 = ORIENTED_EDGE ( 'NONE', *, *, #21823, .F. ) ;
#9337 = ORIENTED_EDGE ( 'NONE', *, *, #27958, .F. ) ;
#9338 = CARTESIAN_POINT ( 'NONE',  ( -4.000000000000000000, 0.000000000000000000, 35.10000000000000142 ) ) ;
#9339 = CIRCLE ( 'NONE', #4197, 47.49900000000000944 ) ;
#9340 = CARTESIAN_POINT ( 'NONE',  ( -50.00000000000000000, -25.98076211353320275, 84.99999999999992895 ) ) ;
#9341 = ORIENTED_EDGE ( 'NONE', *, *, #9982, .T. ) ;
#9342 = EDGE_CURVE ( 'NONE', #15405, #17551, #13081, .T. ) ;
#9343 = ORIENTED_EDGE ( 'NONE', *, *, #6858, .T. ) ;
#9344 = CIRCLE ( 'NONE', #17965, 3.799999999999999822 ) ;
#9345 = ADVANCED_FACE ( 'NONE', ( #16626 ), #24393, .T. ) ;
#9346 = CARTESIAN_POINT ( 'NONE',  ( 0.000000000000000000, -40.47821179127737423, 32.64221760512746329 ) ) ;
#9347 = ORIENTED_EDGE ( 'NONE', *, *, #4363, .F. ) ;
#9348 = CARTESIAN_POINT ( 'NONE',  ( -38.97545270896704039, -114.8876895276775087, 6.152725545821551734 ) ) ;
#9349 = SHAPE_REPRESENTATION_RELATIONSHIP ( 'NONE' , 'NONE' ,  #30285, #487 ) ;
#9350 = CARTESIAN_POINT ( 'NONE',  ( -90.00000000000002842, -2.775557561562891351E-16, -4.000000000000007105 ) ) ;
#9351 = ORIENTED_EDGE ( 'NONE', *, *, #21110, .F. ) ;
#9352 = ORIENTED_EDGE ( 'NONE', *, *, #20078, .F. ) ;
#9353 = CARTESIAN_POINT ( 'NONE',  ( -35.50000000000000000, -117.0141134414687514, -0.5779076015960331603 ) ) ;
#9354 = DIRECTION ( 'NONE',  ( 0.000000000000000000, 0.000000000000000000, 1.000000000000000000 ) ) ;
#9355 = VERTEX_POINT ( 'NONE', #8341 ) ;
#9356 = CARTESIAN_POINT ( 'NONE',  ( -38.00000068757622529, -114.9929510916434339, 12.61439929482944855 ) ) ;
#9357 = VECTOR ( 'NONE', #21095, 1000.000000000000000 ) ;
#9358 = CARTESIAN_POINT ( 'NONE',  ( -37.74437085908086686, -113.9929510916434339, 14.09929883582536903 ) ) ;
#9359 = CIRCLE ( 'NONE', #3060, 11.00000000000001066 ) ;
#9360 = CARTESIAN_POINT ( 'NONE',  ( 0.9999999999999731326, -4.808326913196006913, 0.000000000000000000 ) ) ;
#9361 = FACE_OUTER_BOUND ( 'NONE', #9963, .T. ) ;
#9362 = CIRCLE ( 'NONE', #5379, 3.000000000000002665 ) ;
#9363 = CARTESIAN_POINT ( 'NONE',  ( -38.81062062679291813, -113.9929510916434339, 13.37409560816442244 ) ) ;
#9364 = CARTESIAN_POINT ( 'NONE',  ( 7.999999999999992895, 46.87740477351712798, 3.172455868806031809 ) ) ;
#9365 = CARTESIAN_POINT ( 'NONE',  ( -36.31249999999995026, -114.9929510916434339, 13.11852480586264669 ) ) ;
#9366 = VERTEX_POINT ( 'NONE', #7813 ) ;
#9367 = DIRECTION ( 'NONE',  ( -1.000000000000000000, 0.000000000000000000, 0.000000000000000000 ) ) ;
#9368 = CARTESIAN_POINT ( 'NONE',  ( 4.000000000000000000, 4.898587196589412829E-16, 65.00000000000000000 ) ) ;
#9369 = EDGE_CURVE ( 'NONE', #17571, #5963, #29621, .T. ) ;
#9370 = EDGE_LOOP ( 'NONE', ( #1368, #11901, #27951, #13082 ) ) ;
#9371 = CARTESIAN_POINT ( 'NONE',  ( -35.50000000000000711, -114.9656200615856818, 10.26631071845107179 ) ) ;
#9372 = VERTEX_POINT ( 'NONE', #19322 ) ;
#9373 = CARTESIAN_POINT ( 'NONE',  ( -38.97545270896704039, -113.1123104723225197, 2.347274454178448710 ) ) ;
#9374 = ORIENTED_EDGE ( 'NONE', *, *, #4078, .F. ) ;
#9375 = CIRCLE ( 'NONE', #7086, 0.5000000000000004441 ) ;
#9376 = LINE ( 'NONE', #34228, #15899 ) ;
#9377 = VERTEX_POINT ( 'NONE', #27276 ) ;
#9378 = AXIS2_PLACEMENT_3D ( 'NONE', #34124, #7457, #31946 ) ;
#9379 = CARTESIAN_POINT ( 'NONE',  ( -35.50000000000000000, -113.1807644833805426, -0.6247823525984269599 ) ) ;
#9380 = CYLINDRICAL_SURFACE ( 'NONE', #11577, 7.999999999999992895 ) ;
#9381 = CARTESIAN_POINT ( 'NONE',  ( 55.00000000000000000, 20.00000000000001776, 120.0000000000000000 ) ) ;
#9382 = ORIENTED_EDGE ( 'NONE', *, *, #29836, .F. ) ;
#9383 = CARTESIAN_POINT ( 'NONE',  ( -37.05926240293131713, -115.9999999999999858, 3.378524454178448710 ) ) ;
#9384 = CARTESIAN_POINT ( 'NONE',  ( -55.00000000000000000, 10.00000000000000888, -25.00000000000000000 ) ) ;
#9385 = AXIS2_PLACEMENT_3D ( 'NONE', #25595, #33162, #16589 ) ;
#9386 = CARTESIAN_POINT ( 'NONE',  ( -35.50000000000000711, -112.6919296022648638, -1.573728109100751116 ) ) ;
#9387 = CIRCLE ( 'NONE', #32967, 20.00000000000000355 ) ;
#9388 = ORIENTED_EDGE ( 'NONE', *, *, #15653, .T. ) ;
#9389 = VERTEX_POINT ( 'NONE', #21857 ) ;
#9390 = CYLINDRICAL_SURFACE ( 'NONE', #8470, 19.99999999999998579 ) ;
#9391 =( NAMED_UNIT ( * ) SI_UNIT ( $, .STERADIAN. ) SOLID_ANGLE_UNIT ( ) );
#9392 = CARTESIAN_POINT ( 'NONE',  ( 0.000000000000000000, 0.000000000000000000, 0.000000000000000000 ) ) ;
#9393 = ORIENTED_EDGE ( 'NONE', *, *, #20447, .F. ) ;
#9394 = VERTEX_POINT ( 'NONE', #2440 ) ;
#9395 = CARTESIAN_POINT ( 'NONE',  ( -34.50000000000000000, -114.8057644833805568, -1.624782352598427959 ) ) ;
#9396 = FACE_OUTER_BOUND ( 'NONE', #27636, .T. ) ;
#9397 = ORIENTED_EDGE ( 'NONE', *, *, #10411, .F. ) ;
#9398 = ORIENTED_EDGE ( 'NONE', *, *, #14308, .T. ) ;
#9399 = CARTESIAN_POINT ( 'NONE',  ( 1.520000000000021334, 0.000000000000000000, 0.000000000000000000 ) ) ;
#9400 = AXIS2_PLACEMENT_3D ( 'NONE', #15418, #23904, #4120 ) ;
#9401 = CARTESIAN_POINT ( 'NONE',  ( -37.49414064056232831, -113.9929510916434339, 13.11852578240983291 ) ) ;
#9402 = DIRECTION ( 'NONE',  ( -0.000000000000000000, 0.8986054237126863686, 0.4387576694191721027 ) ) ;
#9403 = DIRECTION ( 'NONE',  ( 1.000000000000000000, 0.000000000000000000, -0.000000000000000000 ) ) ;
#9404 = CARTESIAN_POINT ( 'NONE',  ( -35.50000000000000000, -113.9929510916434339, 10.56126450660895699 ) ) ;
#9405 = CARTESIAN_POINT ( 'NONE',  ( -35.50000000000000000, -115.9929510916434481, 12.39849696637031684 ) ) ;
#9406 = DIRECTION ( 'NONE',  ( 0.000000000000000000, 1.000000000000000000, 3.491564676272318479E-15 ) ) ;
#9408 = AXIS2_PLACEMENT_3D ( 'NONE', #21776, #4886, #32771 ) ;
#9407 = DIRECTION ( 'NONE',  ( -1.000000000000000000, 0.000000000000000000, 0.000000000000000000 ) ) ;
#9409 = EDGE_CURVE ( 'NONE', #3677, #19516, #2808, .T. ) ;
#9410 = AXIS2_PLACEMENT_3D ( 'NONE', #29077, #10170, #1533 ) ;
#9411 = DIRECTION ( 'NONE',  ( -1.000000000000000000, 0.000000000000000000, 0.000000000000000000 ) ) ;
#9412 = DIRECTION ( 'NONE',  ( 1.000000000000000000, 0.000000000000000000, 0.000000000000000000 ) ) ;
#9413 = CARTESIAN_POINT ( 'NONE',  ( 8.000000000000000000, 0.000000000000000000, 0.000000000000000000 ) ) ;
#9414 = EDGE_LOOP ( 'NONE', ( #10581, #5124 ) ) ;
#9415 = CARTESIAN_POINT ( 'NONE',  ( 0.000000000000000000, 19.60123832284017453, 3.973846525876500113 ) ) ;
#9416 = AXIS2_PLACEMENT_3D ( 'NONE', #10776, #11128, #30214 ) ;
#9417 = CARTESIAN_POINT ( 'NONE',  ( -35.50000000000000711, -113.0106174888879877, 1.881901162060937827 ) ) ;
#9418 = DIRECTION ( 'NONE',  ( 0.000000000000000000, 0.8660254037844398178, -0.4999999999999977796 ) ) ;
#9419 = ITEM_DEFINED_TRANSFORMATION ( 'NONE', 'NONE', #23034,  #21307 ) ;
#9420 = EDGE_CURVE ( 'NONE', #16181, #793, #29805, .T. ) ;
#9421 = CARTESIAN_POINT ( 'NONE',  ( 7.999999999999992895, -46.90537658765333617, 2.727856614654147638 ) ) ;
#9422 = CARTESIAN_POINT ( 'NONE',  ( 0.000000000000000000, 27.79676263918186052, 37.88001506494778425 ) ) ;
#9423 = ORIENTED_EDGE ( 'NONE', *, *, #19827, .T. ) ;
#9424 = DIRECTION ( 'NONE',  ( -1.000000000000000000, 0.000000000000000000, 0.000000000000000000 ) ) ;
#9425 = CARTESIAN_POINT ( 'NONE',  ( -34.50000000000000000, -117.0140814545088688, -0.6738694770610542673 ) ) ;
#9426 = LINE ( 'NONE', #23282, #18570 ) ;
#9427 = EDGE_LOOP ( 'NONE', ( #12031, #25587, #5461, #7871 ) ) ;
#9428 = EDGE_LOOP ( 'NONE', ( #5950, #16029, #26626, #26547 ) ) ;
#9429 = CARTESIAN_POINT ( 'NONE',  ( -36.64504884055823908, -115.0245472910329880, 4.784774454178448266 ) ) ;
#9430 = EDGE_LOOP ( 'NONE', ( #3803, #141, #4500, #11157 ) ) ;
#9431 = FILL_AREA_STYLE_COLOUR ( '', #28830 ) ;
#9432 = ORIENTED_EDGE ( 'NONE', *, *, #3164, .T. ) ;
#9433 = ORIENTED_EDGE ( 'NONE', *, *, #13879, .F. ) ;
#9434 = CARTESIAN_POINT ( 'NONE',  ( -35.50000000000000000, -114.9307644833806137, -0.6247823525984269599 ) ) ;
#9435 =( REPRESENTATION_RELATIONSHIP ('NONE','NONE', #26607, #2005 ) REPRESENTATION_RELATIONSHIP_WITH_TRANSFORMATION ( #20572 )SHAPE_REPRESENTATION_RELATIONSHIP( ) );
#9436 = CIRCLE ( 'NONE', #236, 20.00000000000000355 ) ;
#9437 = CARTESIAN_POINT ( 'NONE',  ( 0.000000000000000000, 39.78933988720114456, 24.98727647985016276 ) ) ;
#9438 = EDGE_CURVE ( 'NONE', #35006, #28580, #25745, .T. ) ;
#9439 = CARTESIAN_POINT ( 'NONE',  ( 8.000000000000000000, 16.59870953437680896, 10.45300502024389822 ) ) ;
#9440 = CARTESIAN_POINT ( 'NONE',  ( -35.50160444427493189, -114.9929510916434339, 12.65937477241749853 ) ) ;
#9441 = DIRECTION ( 'NONE',  ( 0.000000000000000000, 1.000000000000000000, 0.000000000000000000 ) ) ;
#9442 = DIRECTION ( 'NONE',  ( -1.000000000000000000, 0.000000000000000000, 0.000000000000000000 ) ) ;
#9443 = CARTESIAN_POINT ( 'NONE',  ( -36.03125000000004263, -114.9929510916434339, 14.11852480586264846 ) ) ;
#9444 = DIRECTION ( 'NONE',  ( -1.000000000000000000, 0.000000000000000000, -0.000000000000000000 ) ) ;
#9445 = EDGE_CURVE ( 'NONE', #19012, #7584, #3900, .T. ) ;
#9446 = EDGE_CURVE ( 'NONE', #27376, #21688, #35208, .T. ) ;
#9447 = LINE ( 'NONE', #12330, #12871 ) ;
#9448 = ORIENTED_EDGE ( 'NONE', *, *, #25398, .T. ) ;
#9449 = EDGE_CURVE ( 'NONE', #3877, #26571, #10705, .T. ) ;
#9450 = CARTESIAN_POINT ( 'NONE',  ( -39.00000000000000000, -115.9929510916434481, 12.44250253426875119 ) ) ;
#9451 = DIRECTION ( 'NONE',  ( -1.000000000000000000, 0.000000000000000000, -0.000000000000000000 ) ) ;
#9452 = CARTESIAN_POINT ( 'NONE',  ( 4.121423858225409909, -12.61643262889541894, -1.200000000000006617 ) ) ;
#9453 = DIRECTION ( 'NONE',  ( -1.000000000000000000, 0.000000000000000000, 0.000000000000000000 ) ) ;
#9454 = DIRECTION ( 'NONE',  ( -1.000000000000000000, 4.625929269271460867E-15, 1.156482317317865217E-15 ) ) ;
#9455 = DIRECTION ( 'NONE',  ( 0.000000000000000000, 0.8660254037844385966, 0.5000000000000001110 ) ) ;
#9456 = DIRECTION ( 'NONE',  ( 0.000000000000000000, 0.000000000000000000, -1.000000000000000000 ) ) ;
#9457 = CIRCLE ( 'NONE', #18086, 4.800000000000000711 ) ;
#9458 = VECTOR ( 'NONE', #1060, 1000.000000000000000 ) ;
#9459 = DIRECTION ( 'NONE',  ( 1.000000000000000000, -4.524158825347490025E-15, -1.177133787269970298E-15 ) ) ;
#9460 = DIRECTION ( 'NONE',  ( 0.000000000000000000, 0.000000000000000000, 1.000000000000000000 ) ) ;
#9461 = ORIENTED_EDGE ( 'NONE', *, *, #33761, .F. ) ;
#9462 = EDGE_CURVE ( 'NONE', #26147, #12715, #248, .T. ) ;
#9463 = CARTESIAN_POINT ( 'NONE',  ( -37.99999999999998579, -114.0592624029313242, 6.246475545821551734 ) ) ;
#9464 = CARTESIAN_POINT ( 'NONE',  ( 7.999999999999992895, 29.60891106212789126, 37.14118181634776050 ) ) ;
#9465 = DIRECTION ( 'NONE',  ( 0.000000000000000000, 0.000000000000000000, -1.000000000000000000 ) ) ;
#9466 = EDGE_CURVE ( 'NONE', #26081, #30439, #2167, .T. ) ;
#9467 = CIRCLE ( 'NONE', #26734, 9.499000000000004107 ) ;
#9468 = VERTEX_POINT ( 'NONE', #24217 ) ;
#9469 = EDGE_LOOP ( 'NONE', ( #9734, #10298, #730, #11211, #16017, #16178 ) ) ;
#9470 = LINE ( 'NONE', #34147, #30884 ) ;
#9471 = CYLINDRICAL_SURFACE ( 'NONE', #3156, 10.50000000000000178 ) ;
#9472 = ORIENTED_EDGE ( 'NONE', *, *, #33761, .T. ) ;
#9473 = CARTESIAN_POINT ( 'NONE',  ( -37.05926240293131713, -111.0000000000000284, 6.621475545821551734 ) ) ;
#9474 = VERTEX_POINT ( 'NONE', #2274 ) ;
#9475 = AXIS2_PLACEMENT_3D ( 'NONE', #30104, #8486, #19106 ) ;
#9476 = CYLINDRICAL_SURFACE ( 'NONE', #32686, 9.999999999999994671 ) ;
#9477 = CARTESIAN_POINT ( 'NONE',  ( 0.000000000000000000, -2.710505431213761085E-17, 38.00000000000000711 ) ) ;
#9478 = CYLINDRICAL_SURFACE ( 'NONE', #27533, 8.000000000000007105 ) ;
#9479 = APPLICATION_PROTOCOL_DEFINITION ( 'draft international standard', 'automotive_design', 1998, #10343 ) ;
#9480 = EDGE_CURVE ( 'NONE', #30694, #23286, #17681, .T. ) ;
#9481 = CARTESIAN_POINT ( 'NONE',  ( 0.000000000000000000, 49.65209126885784485, -15.44894276735497840 ) ) ;
#9482 = ORIENTED_EDGE ( 'NONE', *, *, #3789, .F. ) ;
#9483 = VERTEX_POINT ( 'NONE', #17504 ) ;
#9484 = AXIS2_PLACEMENT_3D ( 'NONE', #27364, #3055, #33954 ) ;
#9485 = CIRCLE ( 'NONE', #23895, 2.999999999999988898 ) ;
#9486 = DIRECTION ( 'NONE',  ( -1.783119874454246424E-31, -1.187911941725854497E-31, 1.000000000000000000 ) ) ;
#9487 = PRODUCT_RELATED_PRODUCT_CATEGORY ( 'part', '', ( #6342 ) ) ;
#9488 = DIRECTION ( 'NONE',  ( 0.000000000000000000, 0.8660254037844381525, 0.5000000000000006661 ) ) ;
#9489 = VERTEX_POINT ( 'NONE', #23087 ) ;
#9490 = CARTESIAN_POINT ( 'NONE',  ( 0.000000000000000000, 0.000000000000000000, -1.200000000000006617 ) ) ;
#9491 = CARTESIAN_POINT ( 'NONE',  ( -34.50000000000000000, -113.8159288351371714, 1.978028123174813802 ) ) ;
#9492 = DIRECTION ( 'NONE',  ( -1.047965281155519790E-16, -6.938893903907192632E-17, -1.000000000000000000 ) ) ;
#9493 = DIRECTION ( 'NONE',  ( 1.000000000000000000, -0.000000000000000000, -0.000000000000000000 ) ) ;
#9494 = VECTOR ( 'NONE', #16061, 1000.000000000000000 ) ;
#9495 = CARTESIAN_POINT ( 'NONE',  ( -34.50000000000000000, -114.7000328234681206, 8.631511418192262752 ) ) ;
#9496 = EDGE_CURVE ( 'NONE', #23013, #15452, #5064, .T. ) ;
#9497 = ADVANCED_FACE ( 'NONE', ( #9061 ), #20019, .T. ) ;
#9498 = LINE ( 'NONE', #31814, #34132 ) ;
#9499 = FACE_OUTER_BOUND ( 'NONE', #31702, .T. ) ;
#9500 = EDGE_CURVE ( 'NONE', #32704, #8928, #33217, .T. ) ;
#9501 = CARTESIAN_POINT ( 'NONE',  ( -38.99924736195578134, -114.9929510916434339, 12.66759465831984777 ) ) ;
#9502 = DIRECTION ( 'NONE',  ( 0.000000000000000000, -0.3681245526846853022, 0.9297764858882484607 ) ) ;
#9503 = CYLINDRICAL_SURFACE ( 'NONE', #20135, 17.49900000000000233 ) ;
#9504 = VECTOR ( 'NONE', #1447, 1000.000000000000000 ) ;
#9505 = DIRECTION ( 'NONE',  ( -1.000000000000000000, -0.000000000000000000, 0.000000000000000000 ) ) ;
#9506 = CARTESIAN_POINT ( 'NONE',  ( -4.000000000000000000, -2.710505431213761085E-17, 54.99999999999999289 ) ) ;
#9507 = CARTESIAN_POINT ( 'NONE',  ( 7.999999999999992895, -35.11945359308137427, 38.34871548466002622 ) ) ;
#9508 = ORIENTED_EDGE ( 'NONE', *, *, #27164, .F. ) ;
#9509 = CARTESIAN_POINT ( 'NONE',  ( -36.94073759706868287, -116.9999999999999858, 5.871475545821551734 ) ) ;
#9510 = CARTESIAN_POINT ( 'NONE',  ( 0.000000000000000000, 0.000000000000000000, 0.000000000000000000 ) ) ;
#9511 = CARTESIAN_POINT ( 'NONE',  ( -35.50000000000000000, -113.0140978167139991, 0.8595926474015699315 ) ) ;
#9512 = EDGE_CURVE ( 'NONE', #1926, #34437, #32652, .T. ) ;
#9513 = ORIENTED_EDGE ( 'NONE', *, *, #743, .T. ) ;
#9514 = ORIENTED_EDGE ( 'NONE', *, *, #21129, .F. ) ;
#9516 = DIRECTION ( 'NONE',  ( 0.000000000000000000, 0.5000000000000011102, -0.8660254037844379305 ) ) ;
#9515 = PRODUCT_DEFINITION_SHAPE ( 'NONE', 'NONE',  #35638 ) ;
#9517 = CIRCLE ( 'NONE', #22174, 3.799999999999999822 ) ;
#9518 = CARTESIAN_POINT ( 'NONE',  ( 8.000000000000000000, -13.55483219355720337, -11.06713717293254362 ) ) ;
#9519 = VERTEX_POINT ( 'NONE', #3853 ) ;
#9520 = ORIENTED_EDGE ( 'NONE', *, *, #28690, .F. ) ;
#9521 = VECTOR ( 'NONE', #27286, 1000.000000000000000 ) ;
#9522 = VECTOR ( 'NONE', #19485, 999.9999999999998863 ) ;
#9523 = CARTESIAN_POINT ( 'NONE',  ( 0.000000000000000000, 0.000000000000000000, -31.10000000000000142 ) ) ;
#9524 = CARTESIAN_POINT ( 'NONE',  ( -37.05926240293131713, -112.0000000000000142, 6.621475545821550845 ) ) ;
#9525 = DIRECTION ( 'NONE',  ( 1.000000000000000000, 0.000000000000000000, 0.000000000000000000 ) ) ;
#9526 = EDGE_CURVE ( 'NONE', #16934, #9489, #11958, .T. ) ;
#9527 = FACE_OUTER_BOUND ( 'NONE', #24949, .T. ) ;
#9529 = ORIENTED_EDGE ( 'NONE', *, *, #23165, .F. ) ;
#9528 = CONICAL_SURFACE ( 'NONE', #22189, 4.725000000000016520, 0.5675376247847534472 ) ;
#9530 = ORIENTED_EDGE ( 'NONE', *, *, #34559, .T. ) ;
#9531 = CARTESIAN_POINT ( 'NONE',  ( -35.50000000000000000, -111.0173113992184710, -0.7556348869410824953 ) ) ;
#9532 = EDGE_CURVE ( 'NONE', #34282, #1802, #3325, .T. ) ;
#9533 = CARTESIAN_POINT ( 'NONE',  ( 7.999999999999992895, 14.30000000000000071, 0.000000000000000000 ) ) ;
#9534 = UNCERTAINTY_MEASURE_WITH_UNIT (LENGTH_MEASURE( 1.000000000000000082E-05 ), #32736, 'distance_accuracy_value', 'NONE');
#9535 = CARTESIAN_POINT ( 'NONE',  ( 8.000000000000000000, -11.06713717293229138, -13.55483219355740765 ) ) ;
#9536 = VERTEX_POINT ( 'NONE', #5835 ) ;
#9537 = CARTESIAN_POINT ( 'NONE',  ( -37.99994980024369085, -114.9929510916434339, 12.62670525340494621 ) ) ;
#9538 = CARTESIAN_POINT ( 'NONE',  ( -34.50000000000000000, -114.1091535596544873, 9.513028657562415447 ) ) ;
#9539 = CIRCLE ( 'NONE', #11294, 3.799999999999999822 ) ;
#9540 = CYLINDRICAL_SURFACE ( 'NONE', #29815, 22.00000000000000000 ) ;
#9541 = EDGE_CURVE ( 'NONE', #5076, #22699, #25456, .T. ) ;
#9542 = DIRECTION ( 'NONE',  ( 0.000000000000000000, 0.000000000000000000, 1.000000000000000000 ) ) ;
#9543 = ADVANCED_FACE ( 'NONE', ( #17322 ), #16797, .T. ) ;
#9544 = CARTESIAN_POINT ( 'NONE',  ( -39.00000206272865455, -113.9929510916434339, 12.61164896875035879 ) ) ;
#9545 = DIRECTION ( 'NONE',  ( 0.000000000000000000, 0.000000000000000000, 1.000000000000000000 ) ) ;
#9546 = VECTOR ( 'NONE', #11591, 1000.000000000000000 ) ;
#9547 = CARTESIAN_POINT ( 'NONE',  ( -35.50000000000000711, -114.9929510916434339, 12.26648026267477221 ) ) ;
#9548 = ORIENTED_EDGE ( 'NONE', *, *, #8321, .F. ) ;
#9549 = AXIS2_PLACEMENT_3D ( 'NONE', #12000, #10003, #18280 ) ;
#9550 = DIRECTION ( 'NONE',  ( 0.000000000000000000, -0.9848077530122062440, -0.1736481776669401844 ) ) ;
#9551 = DIRECTION ( 'NONE',  ( 1.000000000000000000, 0.000000000000000000, 0.000000000000000000 ) ) ;
#9552 = EDGE_LOOP ( 'NONE', ( #26997, #3261, #21069, #6931 ) ) ;
#9553 = CARTESIAN_POINT ( 'NONE',  ( -35.50000000000000711, -114.9929510916434339, 10.55026311463432087 ) ) ;
#9554 = EDGE_LOOP ( 'NONE', ( #17339, #25796, #13268, #18185 ) ) ;
#9555 = CARTESIAN_POINT ( 'NONE',  ( 22.99999999999999645, -12.99999999999998224, 0.000000000000000000 ) ) ;
#9556 = AXIS2_PLACEMENT_3D ( 'NONE', #4402, #28705, #25649 ) ;
#9557 = VERTEX_POINT ( 'NONE', #1144 ) ;
#9558 = CARTESIAN_POINT ( 'NONE',  ( 0.000000000000000000, 0.000000000000000000, 55.00000000000000000 ) ) ;
#9559 = EDGE_LOOP ( 'NONE', ( #24810, #20692, #25514, #4275 ) ) ;
#9560 = CARTESIAN_POINT ( 'NONE',  ( -34.50000000000000000, -113.3822401464312719, 0.9191614010536472978 ) ) ;
#9561 = FACE_BOUND ( 'NONE', #12157, .T. ) ;
#9562 = DIRECTION ( 'NONE',  ( -1.000000000000000000, -0.000000000000000000, 0.000000000000000000 ) ) ;
#9563 = ORIENTED_EDGE ( 'NONE', *, *, #32780, .F. ) ;
#9564 = CARTESIAN_POINT ( 'NONE',  ( -35.00000000000000000, -114.0592624029313242, 6.003524454178450043 ) ) ;
#9565 = VECTOR ( 'NONE', #28280, 1000.000000000000000 ) ;
#9566 = DIRECTION ( 'NONE',  ( -1.000000000000000000, 0.000000000000000000, 0.000000000000000000 ) ) ;
#9567 = AXIS2_PLACEMENT_3D ( 'NONE', #12438, #32723, #8050 ) ;
#9568 = CARTESIAN_POINT ( 'NONE',  ( -35.50000000000000711, -112.0140978167138712, 0.2502176474015765373 ) ) ;
#9569 = ORIENTED_EDGE ( 'NONE', *, *, #26417, .F. ) ;
#9570 = ORIENTED_EDGE ( 'NONE', *, *, #29758, .F. ) ;
#9571 = CARTESIAN_POINT ( 'NONE',  ( 7.999999999999992895, 0.000000000000000000, 0.000000000000000000 ) ) ;
#9572 = CIRCLE ( 'NONE', #13585, 45.00000000000000000 ) ;
#9573 = AXIS2_PLACEMENT_3D ( 'NONE', #6055, #13459, #24440 ) ;
#9574 = ADVANCED_FACE ( 'NONE', ( #17147 ), #22552, .T. ) ;
#9575 = DIRECTION ( 'NONE',  ( 0.000000000000000000, -1.000000000000000000, 0.000000000000000000 ) ) ;
#9576 = ORIENTED_EDGE ( 'NONE', *, *, #33921, .F. ) ;
#9577 = EDGE_LOOP ( 'NONE', ( #4982, #4791, #13532, #23805 ) ) ;
#9578 = CARTESIAN_POINT ( 'NONE',  ( -34.50000000000000000, -114.6807644833805000, -1.624782352598427959 ) ) ;
#9579 = AXIS2_PLACEMENT_3D ( 'NONE', #2630, #29818, #4798 ) ;
#9580 = CARTESIAN_POINT ( 'NONE',  ( -35.50000000000000711, -112.6605569508015350, 1.812590711673265575 ) ) ;
#9581 = ADVANCED_FACE ( 'NONE', ( #33724, #8528 ), #33373, .T. ) ;
#9582 = AXIS2_PLACEMENT_3D ( 'NONE', #3187, #1190, #8917 ) ;
#9583 = ORIENTED_EDGE ( 'NONE', *, *, #33214, .T. ) ;
#9584 = EDGE_LOOP ( 'NONE', ( #18939, #501, #8942, #16858 ) ) ;
#9585 = CIRCLE ( 'NONE', #28550, 4.000000000000003553 ) ;
#9586 = CARTESIAN_POINT ( 'NONE',  ( -34.49999999999998579, -34.23950567274748380, 96.30456345124107997 ) ) ;
#9587 = AXIS2_PLACEMENT_3D ( 'NONE', #13456, #19025, #30024 ) ;
#9588 = CARTESIAN_POINT ( 'NONE',  ( -35.97955704204053262, -113.9929510916434339, 13.11812344617474402 ) ) ;
#9589 = CARTESIAN_POINT ( 'NONE',  ( 8.000000000000000000, -6.336799421339930127, 16.31134495048480915 ) ) ;
#9590 = CARTESIAN_POINT ( 'NONE',  ( -36.24999999999983658, -113.9929510916434339, 13.11852480586264846 ) ) ;
#9591 = CARTESIAN_POINT ( 'NONE',  ( -35.50000000000000000, -115.9929510916434481, 12.59652202191340464 ) ) ;
#9592 = AXIS2_PLACEMENT_3D ( 'NONE', #30756, #3411, #33624 ) ;
#9593 = CARTESIAN_POINT ( 'NONE',  ( 7.999999999999992895, -46.87740477351715640, -3.172455868805712509 ) ) ;
#9594 = CARTESIAN_POINT ( 'NONE',  ( -46.00000000000000000, 9.797174393178839462E-16, 61.99999999999999289 ) ) ;
#9595 = CIRCLE ( 'NONE', #29731, 52.00000000000000711 ) ;
#9596 = FACE_OUTER_BOUND ( 'NONE', #13868, .T. ) ;
#9597 = CYLINDRICAL_SURFACE ( 'NONE', #30079, 1.000000000000000444 ) ;
#9598 = DIRECTION ( 'NONE',  ( -1.734723475976807094E-16, -2.423959199780483078E-15, 1.000000000000000000 ) ) ;
#9599 = CIRCLE ( 'NONE', #1561, 3.999999999999994227 ) ;
#9600 = ORIENTED_EDGE ( 'NONE', *, *, #8566, .T. ) ;
#9601 = CIRCLE ( 'NONE', #14193, 3.799999999999999822 ) ;
#9602 = LINE ( 'NONE', #23093, #2117 ) ;
#9603 = CARTESIAN_POINT ( 'NONE',  ( -35.50000000000000711, -113.0974311500471714, -1.624782352598427959 ) ) ;
#9604 = CARTESIAN_POINT ( 'NONE',  ( 0.000000000000000000, -16.94522934049206597, -8.128228055639052485 ) ) ;
#9605 = CIRCLE ( 'NONE', #32610, 15.49899999999997391 ) ;
#9606 = VECTOR ( 'NONE', #22789, 1000.000000000000000 ) ;
#9607 = CARTESIAN_POINT ( 'NONE',  ( 4.000000000000000000, 4.898587196589412829E-16, -33.50000000000000711 ) ) ;
#9608 = DIRECTION ( 'NONE',  ( 0.000000000000000000, 0.9848077530122073542, 0.1736481776669339117 ) ) ;
#9609 = EDGE_LOOP ( 'NONE', ( #12803, #19796, #9972, #4988 ) ) ;
#9610 = CARTESIAN_POINT ( 'NONE',  ( 7.999999999999992895, -29.60891106212813995, 37.14118181634756866 ) ) ;
#9611 = CARTESIAN_POINT ( 'NONE',  ( -34.50000000000000000, -114.3474311500471572, -2.624782352598442614 ) ) ;
#9612 = CARTESIAN_POINT ( 'NONE',  ( 8.000000000000000000, 7.317194182740413666, -18.61340026142641690 ) ) ;
#9613 = ORIENTED_EDGE ( 'NONE', *, *, #1551, .T. ) ;
#9614 = ORIENTED_EDGE ( 'NONE', *, *, #29338, .T. ) ;
#9615 = CARTESIAN_POINT ( 'NONE',  ( -37.99999999999998579, -114.0592624029313242, 9.246475545821549957 ) ) ;
#9616 = ORIENTED_EDGE ( 'NONE', *, *, #30212, .T. ) ;
#9617 =( NAMED_UNIT ( * ) SI_UNIT ( $, .STERADIAN. ) SOLID_ANGLE_UNIT ( ) );
#9618 = AXIS2_PLACEMENT_3D ( 'NONE', #16662, #288, #22247 ) ;
#9619 = ORIENTED_EDGE ( 'NONE', *, *, #9065, .T. ) ;
#9620 = ORIENTED_EDGE ( 'NONE', *, *, #15092, .F. ) ;
#9621 = CARTESIAN_POINT ( 'NONE',  ( -34.50000000000000000, -113.0140978167140702, 0.8752176474015603835 ) ) ;
#9622 = ADVANCED_FACE ( 'NONE', ( #16968 ), #11414, .T. ) ;
#9623 = FACE_OUTER_BOUND ( 'NONE', #9428, .T. ) ;
#9624 = AXIS2_PLACEMENT_3D ( 'NONE', #15583, #7499, #8035 ) ;
#9625 = DIRECTION ( 'NONE',  ( -1.000000000000000000, -0.000000000000000000, -0.000000000000000000 ) ) ;
#9626 = AXIS2_PLACEMENT_3D ( 'NONE', #31710, #6333, #14600 ) ;
#9627 = CARTESIAN_POINT ( 'NONE',  ( -36.15625000000007816, -114.9929510916434339, 13.11852480586264669 ) ) ;
#9628 = CYLINDRICAL_SURFACE ( 'NONE', #33364, 13.99999999999999822 ) ;
#9629 = VECTOR ( 'NONE', #17200, 1000.000000000000000 ) ;
#9630 = EDGE_CURVE ( 'NONE', #22033, #14164, #7364, .T. ) ;
#9631 = DIRECTION ( 'NONE',  ( 0.000000000000000000, 0.000000000000000000, -1.000000000000000000 ) ) ;
#9632 = VECTOR ( 'NONE', #27118, 1000.000000000000000 ) ;
#9633 = CARTESIAN_POINT ( 'NONE',  ( -34.50075263804418313, -114.9929510916434339, 12.66759465831979981 ) ) ;
#9634 = DIRECTION ( 'NONE',  ( -1.000000000000000000, 0.000000000000000000, 0.000000000000000000 ) ) ;
#9635 = UNCERTAINTY_MEASURE_WITH_UNIT (LENGTH_MEASURE( 1.000000000000000082E-05 ), #19540, 'distance_accuracy_value', 'NONE');
#9636 = CARTESIAN_POINT ( 'NONE',  ( 0.000000000000000000, 16.31134495048493704, -6.336799421339641469 ) ) ;
#9637 = ORIENTED_EDGE ( 'NONE', *, *, #22684, .F. ) ;
#9638 = CARTESIAN_POINT ( 'NONE',  ( -36.03906250000000000, -115.9929510916434481, 13.11852480586264846 ) ) ;
#9639 = CARTESIAN_POINT ( 'NONE',  ( -35.50000000000000711, -112.8835768857893527, -1.616767172155725740 ) ) ;
#9640 = DIRECTION ( 'NONE',  ( 5.339440136655842133E-16, 1.000000000000000000, -1.918536189538073087E-16 ) ) ;
#9641 = DIRECTION ( 'NONE',  ( -1.000000000000000000, -1.734723475976807094E-16, 0.000000000000000000 ) ) ;
#9642 = AXIS2_PLACEMENT_3D ( 'NONE', #13544, #5275, #15868 ) ;
#9643 = DIRECTION ( 'NONE',  ( -1.000000000000000000, 0.000000000000000000, 0.000000000000000000 ) ) ;
#9644 = CARTESIAN_POINT ( 'NONE',  ( 0.000000000000000000, 0.000000000000000000, -50.00000000000000000 ) ) ;
#9645 = DIRECTION ( 'NONE',  ( 0.000000000000000000, -1.000000000000000000, 0.000000000000000000 ) ) ;
#9646 = FACE_OUTER_BOUND ( 'NONE', #20538, .T. ) ;
#9647 = ORIENTED_EDGE ( 'NONE', *, *, #3659, .T. ) ;
#9648 = CIRCLE ( 'NONE', #13137, 4.800000000000000711 ) ;
#9649 = CARTESIAN_POINT ( 'NONE',  ( -36.33479806579560289, -113.2509883718313262, 5.308975545821551734 ) ) ;
#9650 = CIRCLE ( 'NONE', #1643, 47.49900000000002365 ) ;
#9651 = CARTESIAN_POINT ( 'NONE',  ( -37.49999999999999289, -11.52052244843579309, 115.1848168619253698 ) ) ;
#9652 = VECTOR ( 'NONE', #5212, 1000.000000000000000 ) ;
#9653 = DIRECTION ( 'NONE',  ( -1.000000000000000000, -1.836970198721029934E-16, -0.000000000000000000 ) ) ;
#9654 = ORIENTED_EDGE ( 'NONE', *, *, #28275, .F. ) ;
#9655 = ORIENTED_EDGE ( 'NONE', *, *, #28317, .F. ) ;
#9656 = CARTESIAN_POINT ( 'NONE',  ( 7.999999999999992895, 47.49120266317496686, 0.8606222198176832761 ) ) ;
#9657 = CARTESIAN_POINT ( 'NONE',  ( 7.999999999999992895, 17.08890430202750110, 43.76671000081951490 ) ) ;
#9658 = VERTEX_POINT ( 'NONE', #14275 ) ;
#9659 = CARTESIAN_POINT ( 'NONE',  ( -39.97545270896702618, -115.3019030900506152, 6.152725545821551734 ) ) ;
#9660 = VERTEX_POINT ( 'NONE', #11944 ) ;
#9661 = AXIS2_PLACEMENT_3D ( 'NONE', #28427, #14026, #14542 ) ;
#9662 = DIRECTION ( 'NONE',  ( 0.000000000000000000, 0.000000000000000000, -1.000000000000000000 ) ) ;
#9663 = DIRECTION ( 'NONE',  ( -0.000000000000000000, 0.7535859266250379829, 0.6573494133204068612 ) ) ;
#9664 = EDGE_CURVE ( 'NONE', #18507, #25259, #31494, .T. ) ;
#9665 = ADVANCED_FACE ( 'NONE', ( #33906 ), #9238, .T. ) ;
#9666 = CARTESIAN_POINT ( 'NONE',  ( 7.999999999999992895, 22.43957647427161461, 41.27978878573636479 ) ) ;
#9667 = DIRECTION ( 'NONE',  ( -1.000000000000000000, -0.000000000000000000, -0.000000000000000000 ) ) ;
#9668 = ORIENTED_EDGE ( 'NONE', *, *, #29137, .F. ) ;
#9669 = VERTEX_POINT ( 'NONE', #2046 ) ;
#9670 = CARTESIAN_POINT ( 'NONE',  ( 70.00000600000001327, -25.98076211353320986, 80.99999999999992895 ) ) ;
#9671 = DIRECTION ( 'NONE',  ( 1.110223024625156540E-16, 1.000000000000000000, 0.000000000000000000 ) ) ;
#9672 = AXIS2_PLACEMENT_3D ( 'NONE', #12605, #6835, #34750 ) ;
#9673 = EDGE_CURVE ( 'NONE', #21816, #31978, #29037, .T. ) ;
#9674 = EDGE_LOOP ( 'NONE', ( #3834, #24246, #7530, #28727 ) ) ;
#9675 = DIRECTION ( 'NONE',  ( -1.000000000000000000, 0.000000000000000000, 0.000000000000000000 ) ) ;
#9676 = DIRECTION ( 'NONE',  ( 1.084202172485500613E-16, -6.938893903907203726E-17, -1.000000000000000000 ) ) ;
#9677 = DIRECTION ( 'NONE',  ( 0.000000000000000000, 0.000000000000000000, -1.000000000000000000 ) ) ;
#9678 = CIRCLE ( 'NONE', #28653, 4.000000000000003553 ) ;
#9679 = CARTESIAN_POINT ( 'NONE',  ( -35.90191880024782023, -115.9929510916434481, 14.11551573851449071 ) ) ;
#9680 = DIRECTION ( 'NONE',  ( 1.000000000000000000, 0.000000000000000000, 0.000000000000000000 ) ) ;
#9681 = CARTESIAN_POINT ( 'NONE',  ( 7.999999999999992895, 9.744342220503382279, 46.48873837489803407 ) ) ;
#9682 = CARTESIAN_POINT ( 'NONE',  ( -39.00000000000000711, -114.9929510916434339, 12.59652202191340820 ) ) ;
#9683 = CARTESIAN_POINT ( 'NONE',  ( 4.000000000000000000, 4.627536653468036720E-16, 55.00000000000000000 ) ) ;
#9684 = CIRCLE ( 'NONE', #29828, 12.55910585664918422 ) ;
#9685 = FACE_OUTER_BOUND ( 'NONE', #22148, .T. ) ;
#9686 = DIRECTION ( 'NONE',  ( -1.000000000000000000, 0.000000000000000000, 0.000000000000000000 ) ) ;
#9687 = CARTESIAN_POINT ( 'NONE',  ( -55.00000000000000000, -2.775557561562891351E-14, 110.0000000000000000 ) ) ;
#9688 = DIRECTION ( 'NONE',  ( 0.000000000000000000, 0.000000000000000000, 1.000000000000000000 ) ) ;
#9689 = VERTEX_POINT ( 'NONE', #31379 ) ;
#9690 = CARTESIAN_POINT ( 'NONE',  ( -37.05926240293131713, -111.0000000000000284, 6.621475545821551734 ) ) ;
#9691 = LINE ( 'NONE', #33635, #10115 ) ;
#9692 = ADVANCED_FACE ( 'NONE', ( #7242 ), #28691, .T. ) ;
#9693 = CARTESIAN_POINT ( 'NONE',  ( -35.50000000000000000, -113.4742757288593964, 0.9301473394660054739 ) ) ;
#9694 = ORIENTED_EDGE ( 'NONE', *, *, #5891, .F. ) ;
#9695 = VERTEX_POINT ( 'NONE', #23821 ) ;
#9696 = DIRECTION ( 'NONE',  ( -1.000000000000000000, 0.000000000000000000, 0.000000000000000000 ) ) ;
#9697 = EDGE_LOOP ( 'NONE', ( #21078, #32258, #25799, #17429 ) ) ;
#9698 = AXIS2_PLACEMENT_3D ( 'NONE', #7840, #2831, #8022 ) ;
#9699 = ORIENTED_EDGE ( 'NONE', *, *, #6816, .F. ) ;
#9700 = ORIENTED_EDGE ( 'NONE', *, *, #9816, .F. ) ;
#9701 = CIRCLE ( 'NONE', #25834, 9.999999999999994671 ) ;
#9702 = EDGE_CURVE ( 'NONE', #5670, #32263, #15333, .T. ) ;
#9703 = CYLINDRICAL_SURFACE ( 'NONE', #24037, 13.99999999999999822 ) ;
#9704 = ADVANCED_FACE ( 'NONE', ( #23461 ), #14983, .F. ) ;
#9705 = CARTESIAN_POINT ( 'NONE',  ( -38.45611840935523418, -112.6276912846090568, 7.933975545821552622 ) ) ;
#9706 = ADVANCED_FACE ( 'NONE', ( #31734 ), #6890, .T. ) ;
#9707 = CARTESIAN_POINT ( 'NONE',  ( 48.00000000000000711, 0.000000000000000000, 70.00000000000000000 ) ) ;
#9708 = DIRECTION ( 'NONE',  ( 0.000000000000000000, 0.000000000000000000, -1.000000000000000000 ) ) ;
#9709 = EDGE_LOOP ( 'NONE', ( #5273, #6714, #20331, #18873 ) ) ;
#9710 = ORIENTED_EDGE ( 'NONE', *, *, #22288, .T. ) ;
#9711 = CARTESIAN_POINT ( 'NONE',  ( -35.50000000000000000, -117.0140978167138854, 0.0002176474015578471800 ) ) ;
#9712 = DIRECTION ( 'NONE',  ( 0.000000000000000000, -0.8660254037844444808, 0.4999999999999898415 ) ) ;
#9713 = EDGE_CURVE ( 'NONE', #15438, #342, #25987, .T. ) ;
#9714 = DIRECTION ( 'NONE',  ( -1.000000000000000000, 0.000000000000000000, 0.000000000000000000 ) ) ;
#9715 = VERTEX_POINT ( 'NONE', #20736 ) ;
#9716 = CARTESIAN_POINT ( 'NONE',  ( -1.000000000000014655, -4.808326913196006913, -0.7999999999999951594 ) ) ;
#9717 = ADVANCED_FACE ( 'NONE', ( #6710 ), #12295, .T. ) ;
#9718 = CARTESIAN_POINT ( 'NONE',  ( -34.50000000000000000, -114.9929510916434339, 12.50851088611648088 ) ) ;
#9719 = CARTESIAN_POINT ( 'NONE',  ( 7.999999999999992895, 36.34385289850589373, 29.77717097092089205 ) ) ;
#9720 = CARTESIAN_POINT ( 'NONE',  ( -37.34375000000001421, -114.9929510916434339, 13.11852480586264669 ) ) ;
#9721 = CARTESIAN_POINT ( 'NONE',  ( 7.999999999999992895, -2.123073309834833111, -47.45152853935339010 ) ) ;
#9722 = CARTESIAN_POINT ( 'NONE',  ( -36.06250000000000711, -113.9929510916434339, 14.11852480586265024 ) ) ;
#9723 = LINE ( 'NONE', #33665, #19972 ) ;
#9724 = CARTESIAN_POINT ( 'NONE',  ( -37.49414064056234253, -114.9929510916434339, 13.11852578240983291 ) ) ;
#9725 = ORIENTED_EDGE ( 'NONE', *, *, #26389, .T. ) ;
#9726 = VECTOR ( 'NONE', #1302, 1000.000000000000000 ) ;
#9727 = LINE ( 'NONE', #20517, #30227 ) ;
#9728 = CYLINDRICAL_SURFACE ( 'NONE', #28409, 20.00000000000000711 ) ;
#9729 = ORIENTED_EDGE ( 'NONE', *, *, #34263, .T. ) ;
#9730 = CARTESIAN_POINT ( 'NONE',  ( -35.50000000000000711, -114.9929510916434339, 12.53051367006571581 ) ) ;
#9731 = VERTEX_POINT ( 'NONE', #26347 ) ;
#9732 = CARTESIAN_POINT ( 'NONE',  ( 50.00005079999999680, 5.400000000000021672, 1.000000000000001776 ) ) ;
#9733 = EDGE_CURVE ( 'NONE', #34692, #15039, #1864, .T. ) ;
#9734 = ORIENTED_EDGE ( 'NONE', *, *, #22366, .T. ) ;
#9735 = DIRECTION ( 'NONE',  ( -0.000000000000000000, 2.543449303551180694E-16, -1.000000000000000000 ) ) ;
#9736 = ORIENTED_EDGE ( 'NONE', *, *, #25532, .F. ) ;
#9737 = CARTESIAN_POINT ( 'NONE',  ( -34.50000000000000000, -113.1981689815712997, 0.8971895242272823756 ) ) ;
#9738 = LINE ( 'NONE', #17654, #4694 ) ;
#9739 = EDGE_CURVE ( 'NONE', #15935, #22572, #21711, .T. ) ;
#9740 = CARTESIAN_POINT ( 'NONE',  ( 7.999999999999992895, 0.000000000000000000, 0.000000000000000000 ) ) ;
#9741 = ADVANCED_FACE ( 'NONE', ( #9596 ), #23640, .T. ) ;
#9742 = ORIENTED_EDGE ( 'NONE', *, *, #6475, .F. ) ;
#9743 = CARTESIAN_POINT ( 'NONE',  ( -37.05926240293131713, -115.9999999999999858, 4.878524454178449155 ) ) ;
#9744 = FACE_BOUND ( 'NONE', #25341, .T. ) ;
#9745 = CARTESIAN_POINT ( 'NONE',  ( -35.50000000000000711, -115.8878449012421754, -1.128496220799388494 ) ) ;
#9746 = VERTEX_POINT ( 'NONE', #29231 ) ;
#9747 = VERTEX_POINT ( 'NONE', #9949 ) ;
#9748 = EDGE_CURVE ( 'NONE', #14694, #25713, #26335, .T. ) ;
#9749 = FACE_OUTER_BOUND ( 'NONE', #30910, .T. ) ;
#9750 = CIRCLE ( 'NONE', #16624, 19.99999999999998579 ) ;
#9751 = EDGE_CURVE ( 'NONE', #25349, #26576, #25175, .T. ) ;
#9752 = CARTESIAN_POINT ( 'NONE',  ( 8.000000000000000000, 2.912696353506122104, -21.80633394113446855 ) ) ;
#9753 = VERTEX_POINT ( 'NONE', #17690 ) ;
#9754 = ORIENTED_EDGE ( 'NONE', *, *, #4728, .F. ) ;
#9755 = AXIS2_PLACEMENT_3D ( 'NONE', #5904, #10963, #17224 ) ;
#9756 = CARTESIAN_POINT ( 'NONE',  ( -34.50000000000000000, -114.8474311500471572, -1.624782352598427959 ) ) ;
#9757 = CARTESIAN_POINT ( 'NONE',  ( -35.50000000000000711, -112.0140978167138712, 0.8127176474015721519 ) ) ;
#9758 = CARTESIAN_POINT ( 'NONE',  ( 8.000000000000000000, 3.678165988948591814, 15.05623113391068379 ) ) ;
#9759 = AXIS2_PLACEMENT_3D ( 'NONE', #20305, #6293, #887 ) ;
#9760 = VERTEX_POINT ( 'NONE', #4750 ) ;
#9761 = VERTEX_POINT ( 'NONE', #4576 ) ;
#9762 = CIRCLE ( 'NONE', #25885, 52.00000000000000711 ) ;
#9763 = DIRECTION ( 'NONE',  ( -1.000000000000000000, 0.000000000000000000, 0.000000000000000000 ) ) ;
#9764 = ADVANCED_FACE ( 'NONE', ( #34805 ), #1493, .F. ) ;
#9765 = CARTESIAN_POINT ( 'NONE',  ( -37.97447287825094264, -113.9929510916434339, 12.77960891308616809 ) ) ;
#9766 = CARTESIAN_POINT ( 'NONE',  ( 1.566204647097418912, -6.822536405429468154, -0.7999999999999951594 ) ) ;
#9767 = CARTESIAN_POINT ( 'NONE',  ( -35.91854304697312728, -113.9929510916434339, 13.11211614918345703 ) ) ;
#9768 = CARTESIAN_POINT ( 'NONE',  ( -35.50000000000000000, -115.9929510916434481, 10.52826033068511435 ) ) ;
#9769 = CARTESIAN_POINT ( 'NONE',  ( -34.49999999999998579, -25.01350700525237514, 84.74619386235816876 ) ) ;
#9770 = CYLINDRICAL_SURFACE ( 'NONE', #5988, 0.5000000000000004441 ) ;
#9771 = ORIENTED_EDGE ( 'NONE', *, *, #8189, .F. ) ;
#9772 = DIRECTION ( 'NONE',  ( -0.000000000000000000, 0.000000000000000000, -1.000000000000000000 ) ) ;
#9773 = CARTESIAN_POINT ( 'NONE',  ( 0.000000000000000000, -2.710505431213761085E-17, 29.09999999999999787 ) ) ;
#9774 = CARTESIAN_POINT ( 'NONE',  ( -34.49999999999998579, -27.48076211353326670, 88.99999999999994316 ) ) ;
#9775 = EDGE_CURVE ( 'NONE', #21816, #34202, #10127, .T. ) ;
#9776 = ORIENTED_EDGE ( 'NONE', *, *, #14942, .T. ) ;
#9777 = AXIS2_PLACEMENT_3D ( 'NONE', #32705, #29298, #4648 ) ;
#9778 = DIRECTION ( 'NONE',  ( -1.000000000000000000, 0.000000000000000000, 0.000000000000000000 ) ) ;
#9779 = EDGE_CURVE ( 'NONE', #16466, #22478, #4922, .T. ) ;
#9780 = CARTESIAN_POINT ( 'NONE',  ( -35.50000000000000711, -112.7472371723319355, 1.839427296857320648 ) ) ;
#9781 = FACE_OUTER_BOUND ( 'NONE', #18117, .T. ) ;
#9782 = CARTESIAN_POINT ( 'NONE',  ( 0.000000000000000000, 2.494040418455352182, 18.62763138773848937 ) ) ;
#9783 = CARTESIAN_POINT ( 'NONE',  ( 39.30000000000000426, 10.50000000000000355, 1.285879139104720436E-15 ) ) ;
#9784 = CARTESIAN_POINT ( 'NONE',  ( 50.00000000000000000, -59.99999999999997158, 120.0000000000000000 ) ) ;
#9785 = ORIENTED_EDGE ( 'NONE', *, *, #12379, .F. ) ;
#9786 = CARTESIAN_POINT ( 'NONE',  ( 0.000000000000000000, 0.000000000000000000, 0.000000000000000000 ) ) ;
#9787 = CARTESIAN_POINT ( 'NONE',  ( -34.50000000000000000, -117.0140978167138854, 0.8752176474015623819 ) ) ;
#9788 = CARTESIAN_POINT ( 'NONE',  ( 0.000000000000000000, 0.000000000000000000, 0.000000000000000000 ) ) ;
#9789 = ORIENTED_EDGE ( 'NONE', *, *, #29115, .F. ) ;
#9790 = ORIENTED_EDGE ( 'NONE', *, *, #9733, .F. ) ;
#9791 = EDGE_CURVE ( 'NONE', #4806, #5465, #13688, .T. ) ;
#9792 = CARTESIAN_POINT ( 'NONE',  ( -37.97545270896701908, -113.5265240346955977, 2.347274454178448710 ) ) ;
#9793 = PRESENTATION_STYLE_ASSIGNMENT (( #20930 ) ) ;
#9794 = ORIENTED_EDGE ( 'NONE', *, *, #9173, .F. ) ;
#9795 = EDGE_LOOP ( 'NONE', ( #16396, #26048 ) ) ;
#9796 = CARTESIAN_POINT ( 'NONE',  ( -35.50000000000000000, -115.0140978167138712, -0.6247823525983134951 ) ) ;
#9797 = DIRECTION ( 'NONE',  ( -1.000000000000000000, 0.000000000000000000, -0.000000000000000000 ) ) ;
#9798 = CARTESIAN_POINT ( 'NONE',  ( 8.000000000000007105, 0.3151488735050472778, -11.27190672109269087 ) ) ;
#9799 = CIRCLE ( 'NONE', #13269, 7.199999999999998401 ) ;
#9800 = CARTESIAN_POINT ( 'NONE',  ( -35.99386409314529800, -114.9929510916434339, 13.11852378322482515 ) ) ;
#9801 = DIRECTION ( 'NONE',  ( 0.000000000000000000, 0.5877852522924739143, -0.8090169943749470072 ) ) ;
#9802 = AXIS2_PLACEMENT_3D ( 'NONE', #10716, #32859, #14107 ) ;
#9803 = AXIS2_PLACEMENT_3D ( 'NONE', #5767, #3075, #30437 ) ;
#9804 = CARTESIAN_POINT ( 'NONE',  ( -37.62254989966454133, -114.9929510916434339, 14.11371147303758278 ) ) ;
#9805 = DIRECTION ( 'NONE',  ( -1.000000000000000000, -1.836970198721029934E-16, -0.000000000000000000 ) ) ;
#9806 = PRODUCT ( 'shaft2', 'shaft2', '', ( #8062 ) ) ;
#9807 = DIRECTION ( 'NONE',  ( 1.000000000000000000, 0.000000000000000000, 0.000000000000000000 ) ) ;
#9808 = ORIENTED_EDGE ( 'NONE', *, *, #32550, .T. ) ;
#9809 = CARTESIAN_POINT ( 'NONE',  ( -35.74814306589956203, -115.9929510916434481, 13.05539834812772781 ) ) ;
#9810 = CARTESIAN_POINT ( 'NONE',  ( -35.50000000000000711, -116.0140978167138712, -0.3122823525984417259 ) ) ;
#9811 = FACE_OUTER_BOUND ( 'NONE', #20165, .T. ) ;
#9812 = LINE ( 'NONE', #17731, #32044 ) ;
#9813 = VERTEX_POINT ( 'NONE', #32628 ) ;
#9814 = DIRECTION ( 'NONE',  ( 0.000000000000000000, 0.9672551082808337197, -0.2538061376417689030 ) ) ;
#9815 = DIRECTION ( 'NONE',  ( 0.000000000000000000, 0.000000000000000000, 1.000000000000000000 ) ) ;
#9816 = EDGE_CURVE ( 'NONE', #16768, #33264, #3337, .T. ) ;
#9817 = CARTESIAN_POINT ( 'NONE',  ( 7.999999999999992895, -2.123073309835510791, 47.45152853935334747 ) ) ;
#9818 = DIRECTION ( 'NONE',  ( 0.000000000000000000, 1.000000000000000000, 0.000000000000000000 ) ) ;
#9819 = ORIENTED_EDGE ( 'NONE', *, *, #11439, .T. ) ;
#9820 = CARTESIAN_POINT ( 'NONE',  ( -36.02454729103298092, -114.4734759653044307, 7.597274454178449155 ) ) ;
#9821 = LINE ( 'NONE', #20785, #17545 ) ;
#9822 = DIRECTION ( 'NONE',  ( -1.000000000000000000, 0.000000000000000000, 0.000000000000000000 ) ) ;
#9823 = VERTEX_POINT ( 'NONE', #16588 ) ;
#9824 = VERTEX_POINT ( 'NONE', #2579 ) ;
#9825 = SURFACE_STYLE_FILL_AREA ( #26401 ) ;
#9826 = LINE ( 'NONE', #34327, #34194 ) ;
#9827 = EDGE_LOOP ( 'NONE', ( #22446, #8185, #12994, #133 ) ) ;
#9828 = CARTESIAN_POINT ( 'NONE',  ( -34.00000000000000000, -113.9407375970686758, 6.996475545821551734 ) ) ;
#9829 = ORIENTED_EDGE ( 'NONE', *, *, #23855, .T. ) ;
#9830 = AXIS2_PLACEMENT_3D ( 'NONE', #35349, #27245, #16048 ) ;
#9831 = AXIS2_PLACEMENT_3D ( 'NONE', #34066, #6689, #17672 ) ;
#9832 = CARTESIAN_POINT ( 'NONE',  ( 0.000000000000000000, 0.000000000000000000, 55.00000000000000000 ) ) ;
#9833 = VERTEX_POINT ( 'NONE', #16041 ) ;
#9834 = CARTESIAN_POINT ( 'NONE',  ( -21.15833593587365513, -10.50833024919764469, 77.79903810567677169 ) ) ;
#9835 = CARTESIAN_POINT ( 'NONE',  ( 8.000000000000007105, -1.111908866155017606, -9.433698091065132019 ) ) ;
#9836 = DIRECTION ( 'NONE',  ( -1.174092375852890260E-15, 4.222049128630259891E-16, 1.000000000000000000 ) ) ;
#9837 = ORIENTED_EDGE ( 'NONE', *, *, #24243, .T. ) ;
#9838 = EDGE_LOOP ( 'NONE', ( #19907, #9860, #14024, #16815 ) ) ;
#9839 = CARTESIAN_POINT ( 'NONE',  ( 70.00001200000001234, -28.43894899343287364, 81.80133263040721658 ) ) ;
#9840 = CYLINDRICAL_SURFACE ( 'NONE', #29863, 6.765000000000044977 ) ;
#9841 = EDGE_LOOP ( 'NONE', ( #12343, #11070 ) ) ;
#9842 = CARTESIAN_POINT ( 'NONE',  ( -42.49999999999999289, -37.28532556477448168, 93.25874355921402525 ) ) ;
#9843 = DIRECTION ( 'NONE',  ( 0.000000000000000000, -1.000000000000000000, 0.000000000000000000 ) ) ;
#9844 = CARTESIAN_POINT ( 'NONE',  ( 7.999999999999992895, 27.79676263918241119, -37.88001506494740056 ) ) ;
#9845 = CARTESIAN_POINT ( 'NONE',  ( -37.46874999999995737, -115.9929510916434481, 14.11852480586265024 ) ) ;
#9846 = CARTESIAN_POINT ( 'NONE',  ( 7.999999999999992895, 3.872983346207420574, -1.000000000000000888 ) ) ;
#9847 = CARTESIAN_POINT ( 'NONE',  ( -38.99999999999999289, -113.9407375970686900, 5.253524454178449155 ) ) ;
#9848 = AXIS2_PLACEMENT_3D ( 'NONE', #3405, #33448, #31107 ) ;
#9849 = CARTESIAN_POINT ( 'NONE',  ( -34.50000000000000000, -115.9929510916434481, 12.53051367006571581 ) ) ;
#9851 = CARTESIAN_POINT ( 'NONE',  ( 8.000000000000000000, -3.384281271887680909, -18.48663108841362757 ) ) ;
#9850 = VECTOR ( 'NONE', #2166, 1000.000000000000000 ) ;
#9852 = CARTESIAN_POINT ( 'NONE',  ( 0.000000000000000000, -2.710505431213761085E-17, -45.89999999999999858 ) ) ;
#9853 = DIRECTION ( 'NONE',  ( -1.000000000000000000, 0.000000000000000000, 0.000000000000000000 ) ) ;
#9854 = CARTESIAN_POINT ( 'NONE',  ( 50.00005079999999680, 0.000000000000000000, 0.000000000000000000 ) ) ;
#9855 = APPLICATION_CONTEXT ( 'automotive_design' ) ;
#9856 = EDGE_CURVE ( 'NONE', #741, #26745, #19280, .T. ) ;
#9857 = EDGE_CURVE ( 'NONE', #6685, #876, #21277, .T. ) ;
#9858 = CARTESIAN_POINT ( 'NONE',  ( 0.000000000000000000, -12.49559743815772350, -9.169462670380712055 ) ) ;
#9859 = FILL_AREA_STYLE ('',( #23544 ) ) ;
#9860 = ORIENTED_EDGE ( 'NONE', *, *, #32433, .T. ) ;
#9861 = CARTESIAN_POINT ( 'NONE',  ( -34.83677480945821259, -116.0794154965774965, 7.183975545821551734 ) ) ;
#9862 = FACE_OUTER_BOUND ( 'NONE', #11515, .T. ) ;
#9863 = CARTESIAN_POINT ( 'NONE',  ( -35.50000000000000000, -113.0140978167137717, 0.8752176474015607166 ) ) ;
#9864 = ORIENTED_EDGE ( 'NONE', *, *, #9918, .T. ) ;
#9865 = ORIENTED_EDGE ( 'NONE', *, *, #8633, .F. ) ;
#9866 = LINE ( 'NONE', #10241, #33231 ) ;
#9867 = DIRECTION ( 'NONE',  ( 1.000000000000000000, -0.000000000000000000, 0.000000000000000000 ) ) ;
#9868 = ORIENTED_EDGE ( 'NONE', *, *, #35283, .T. ) ;
#9869 = EDGE_CURVE ( 'NONE', #6851, #11728, #10811, .T. ) ;
#9870 = ORIENTED_EDGE ( 'NONE', *, *, #2462, .T. ) ;
#9871 = ORIENTED_EDGE ( 'NONE', *, *, #33422, .F. ) ;
#9872 = CYLINDRICAL_SURFACE ( 'NONE', #5072, 52.00000000000000711 ) ;
#9873 = DIRECTION ( 'NONE',  ( -1.000000000000000000, 0.000000000000000000, 0.000000000000000000 ) ) ;
#9874 = PRESENTATION_LAYER_ASSIGNMENT (  '', '', ( #32297 ) ) ;
#9875 = CIRCLE ( 'NONE', #16757, 52.00000000000000711 ) ;
#9876 = DIRECTION ( 'NONE',  ( -2.363834971858864035E-17, -0.2580586765732854060, 0.9661292457250449939 ) ) ;
#9877 = CARTESIAN_POINT ( 'NONE',  ( 3.799999999999999822, -2.710505431213761085E-17, 38.90000000000000568 ) ) ;
#9878 = EDGE_LOOP ( 'NONE', ( #35020, #27480 ) ) ;
#9879 = ORIENTED_EDGE ( 'NONE', *, *, #29138, .T. ) ;
#9880 = CARTESIAN_POINT ( 'NONE',  ( -35.50000000000000000, -111.0140821919592327, -0.5779076015960634694 ) ) ;
#9881 = DIRECTION ( 'NONE',  ( 0.000000000000000000, 0.000000000000000000, -1.000000000000000000 ) ) ;
#9882 = CYLINDRICAL_SURFACE ( 'NONE', #14911, 20.00000000000000355 ) ;
#9883 = ORIENTED_EDGE ( 'NONE', *, *, #28132, .F. ) ;
#9884 = FACE_OUTER_BOUND ( 'NONE', #23105, .T. ) ;
#9885 = EDGE_CURVE ( 'NONE', #18097, #15079, #28618, .T. ) ;
#9886 = AXIS2_PLACEMENT_3D ( 'NONE', #2359, #13500, #10619 ) ;
#9887 = CARTESIAN_POINT ( 'NONE',  ( -34.49999793727135255, -114.9929510916434339, 12.61164896875036590 ) ) ;
#9888 = CARTESIAN_POINT ( 'NONE',  ( 8.000000000000000000, -0.9861715913086367413, -17.47118961583605312 ) ) ;
#9889 = CARTESIAN_POINT ( 'NONE',  ( -37.50818044754229419, -114.9929510916434339, 13.11847460610629668 ) ) ;
#9890 = CARTESIAN_POINT ( 'NONE',  ( 8.000000000000007105, -3.975523202428068892, 13.42368113696675103 ) ) ;
#9891 = CARTESIAN_POINT ( 'NONE',  ( -39.00000000000000000, -113.9929510916434339, 12.56351784598954779 ) ) ;
#9892 = FACE_OUTER_BOUND ( 'NONE', #11508, .T. ) ;
#9893 = CARTESIAN_POINT ( 'NONE',  ( -37.75185693410092824, -114.9929510916434339, 13.05539834812634581 ) ) ;
#9894 = DIRECTION ( 'NONE',  ( -1.000000000000000000, 0.000000000000000000, 0.000000000000000000 ) ) ;
#9895 = ORIENTED_EDGE ( 'NONE', *, *, #11093, .T. ) ;
#9896 = DIRECTION ( 'NONE',  ( -1.000000000000000000, -0.000000000000000000, -0.000000000000000000 ) ) ;
#9897 = CARTESIAN_POINT ( 'NONE',  ( 0.000000000000000000, 0.000000000000000000, -55.00000000000000000 ) ) ;
#9898 = ADVANCED_FACE ( 'NONE', ( #24006 ), #35343, .T. ) ;
#9899 = ORIENTED_EDGE ( 'NONE', *, *, #18522, .F. ) ;
#9900 = CIRCLE ( 'NONE', #20230, 4.800000000000006928 ) ;
#9901 = EDGE_CURVE ( 'NONE', #22572, #1546, #10488, .T. ) ;
#9902 = CARTESIAN_POINT ( 'NONE',  ( -35.50000000000000711, -114.9929510916434339, 10.52826033068511435 ) ) ;
#9903 = EDGE_LOOP ( 'NONE', ( #19724, #2975, #23589, #123 ) ) ;
#9904 = EDGE_CURVE ( 'NONE', #16930, #7329, #19108, .T. ) ;
#9905 = CIRCLE ( 'NONE', #16206, 3.800000000000018918 ) ;
#9906 = AXIS2_PLACEMENT_3D ( 'NONE', #13611, #33399, #16651 ) ;
#9907 = CARTESIAN_POINT ( 'NONE',  ( 7.999999999999992895, 0.000000000000000000, 0.000000000000000000 ) ) ;
#9908 = CARTESIAN_POINT ( 'NONE',  ( -4.000000000000000000, -2.710505431213761085E-17, 38.90000000000000568 ) ) ;
#9909 = ORIENTED_EDGE ( 'NONE', *, *, #25316, .T. ) ;
#9910 = DIRECTION ( 'NONE',  ( 0.000000000000000000, 0.8443279255020125218, 0.5358267949790005424 ) ) ;
#9911 = EDGE_LOOP ( 'NONE', ( #1332, #23959, #4586, #13788 ) ) ;
#9912 = CARTESIAN_POINT ( 'NONE',  ( -34.50000000000000000, -113.2441867727860227, 0.9026824934337903672 ) ) ;
#9913 = CARTESIAN_POINT ( 'NONE',  ( 0.000000000000000000, -6.109652351741458709, -46.58570277113513214 ) ) ;
#9914 = CARTESIAN_POINT ( 'NONE',  ( 8.000000000000000000, 13.24207120356986422, -14.98824707027427650 ) ) ;
#9915 = ADVANCED_FACE ( 'NONE', ( #21451 ), #32806, .T. ) ;
#9916 = ORIENTED_EDGE ( 'NONE', *, *, #17409, .T. ) ;
#9917 = CARTESIAN_POINT ( 'NONE',  ( -38.18337828418795965, -110.9754527089670546, 4.034774454178449155 ) ) ;
#9918 = EDGE_CURVE ( 'NONE', #28703, #28380, #12044, .T. ) ;
#9919 = CIRCLE ( 'NONE', #11060, 20.00000000000000355 ) ;
#9920 = CARTESIAN_POINT ( 'NONE',  ( 38.00000000000000000, 14.30000000000001492, 3.000000000000002665 ) ) ;
#9921 = CARTESIAN_POINT ( 'NONE',  ( -35.50000000000000711, -112.9486715495423681, -1.623175561345890472 ) ) ;
#9922 = ORIENTED_EDGE ( 'NONE', *, *, #12376, .T. ) ;
#9923 = ORIENTED_EDGE ( 'NONE', *, *, #13107, .T. ) ;
#9924 = DIRECTION ( 'NONE',  ( -1.000000000000000000, 0.000000000000000000, 0.000000000000000000 ) ) ;
#9925 = CARTESIAN_POINT ( 'NONE',  ( -34.49999999999998579, -33.73076211353324538, 92.74999999999992895 ) ) ;
#9926 = ORIENTED_EDGE ( 'NONE', *, *, #19957, .T. ) ;
#9927 = VERTEX_POINT ( 'NONE', #24353 ) ;
#9928 = CARTESIAN_POINT ( 'NONE',  ( -34.50000000000000000, -113.6807644833805995, -1.624782352598427959 ) ) ;
#9929 = AXIS2_PLACEMENT_3D ( 'NONE', #23643, #32100, #23089 ) ;
#9930 = AXIS2_PLACEMENT_3D ( 'NONE', #18032, #20901, #14805 ) ;
#9931 = DIRECTION ( 'NONE',  ( 0.000000000000000000, 0.000000000000000000, 1.000000000000000000 ) ) ;
#9932 = ORIENTED_EDGE ( 'NONE', *, *, #5712, .F. ) ;
#9933 = EDGE_LOOP ( 'NONE', ( #27048, #4645 ) ) ;
#9934 = CARTESIAN_POINT ( 'NONE',  ( 0.000000000000000000, 0.000000000000000000, -22.00000000000000000 ) ) ;
#9935 = EDGE_CURVE ( 'NONE', #35493, #30249, #32448, .T. ) ;
#9936 = CARTESIAN_POINT ( 'NONE',  ( -38.00000000000000711, -113.9929510916434339, 12.44250253426875119 ) ) ;
#9937 = PRODUCT_RELATED_PRODUCT_CATEGORY ( 'part', '', ( #34550 ) ) ;
#9938 = CARTESIAN_POINT ( 'NONE',  ( 0.000000000000000000, 0.000000000000000000, 0.000000000000000000 ) ) ;
#9939 = EDGE_CURVE ( 'NONE', #13682, #34443, #16635, .T. ) ;
#9940 = CARTESIAN_POINT ( 'NONE',  ( -35.50025087934803736, -113.9929510916434339, 12.63488142334835196 ) ) ;
#9941 = CARTESIAN_POINT ( 'NONE',  ( -38.00000000000000711, -115.9929510916434481, 12.53051367006571937 ) ) ;
#9942 = DIRECTION ( 'NONE',  ( -1.000000000000000000, 0.000000000000000000, 0.000000000000000000 ) ) ;
#9943 = VECTOR ( 'NONE', #12875, 1000.000000000000000 ) ;
#9944 = DIRECTION ( 'NONE',  ( -1.000000000000000000, -0.000000000000000000, 0.000000000000000000 ) ) ;
#9945 = CIRCLE ( 'NONE', #31791, 4.000000000000000000 ) ;
#9946 = EDGE_CURVE ( 'NONE', #23989, #30393, #12620, .T. ) ;
#9947 = ORIENTED_EDGE ( 'NONE', *, *, #15003, .T. ) ;
#9948 = EDGE_CURVE ( 'NONE', #14032, #25616, #30106, .T. ) ;
#9949 = CARTESIAN_POINT ( 'NONE',  ( 8.000000000000007105, 9.433698091065215507, 1.111908866155128628 ) ) ;
#9950 = CARTESIAN_POINT ( 'NONE',  ( 8.000000000000000000, 2.912696353505818792, 21.80633394113451118 ) ) ;
#9951 = CARTESIAN_POINT ( 'NONE',  ( 46.00000000000000000, -25.98076211353320275, 92.99999999999991473 ) ) ;
#9952 = ORIENTED_EDGE ( 'NONE', *, *, #15490, .T. ) ;
#9953 = DIRECTION ( 'NONE',  ( 0.000000000000000000, 0.000000000000000000, 1.000000000000000000 ) ) ;
#9954 = AXIS2_PLACEMENT_3D ( 'NONE', #23464, #28504, #15156 ) ;
#9955 = VECTOR ( 'NONE', #17634, 1000.000000000000114 ) ;
#9956 = CARTESIAN_POINT ( 'NONE',  ( -35.50000000000000711, -112.1222502514821144, 1.343475657184566296 ) ) ;
#9957 = CARTESIAN_POINT ( 'NONE',  ( 46.00000000000000000, 1.347111479062090574E-15, 81.00000000000001421 ) ) ;
#9958 = FACE_OUTER_BOUND ( 'NONE', #14682, .T. ) ;
#9959 = B_SPLINE_CURVE_WITH_KNOTS ( 'NONE', 3,
 ( #33238, #28191, #27839, #8907, #25137, #6222, #14846, #1003, #14479, #6392, #17356, #19531, #11444, #19872, #30537, #17006, #28541, #11612, #3179, #3705, #14655, #28361, #22585, #5867, #25670, #33768, #14137, #17535, #11980, #464, #22947, #30887, #25490, #16832, #33405, #17182, #33946, #8727, #9097, #3530, #25312, #19696, #20228, #30711, #6042, #807, #11786, #20055, #31063, #9274, #28016, #633, #1181, #31238, #6560, #3891, #3363, #25853, #22243, #14309, #32129, #23853, #31766, #12154, #29260, #12328, #34303, #20766, #15725, #1527, #26741, #9633, #1351, #12695, #7456, #23490, #15019, #23672, #26377, #7101, #18074, #18438, #12512, #17722, #4606, #15543, #26562, #4780, #34123, #29436, #7281, #29073, #23125, #34660, #9984, #9443, #15365, #4423, #26192, #23300, #17899, #20594, #1898, #20946, #4247, #20401, #31945, #31590, #10166, #28722, #12874, #34841, #31415, #4075, #6747, #34484, #26023, #6926, #28895, #1709, #15184, #18257, #9804, #21136, #10843, #13884, #30100, #8820, #11366, #33328, #11183, #16746, #33495, #11015, #552, #5789, #14049, #14229, #2925, #24874, #26, #11539, #19272, #27409, #2758, #27590, #32977, #19103, #13720, #25046, #30462, #27756, #19462, #22155, #6136, #199, #17098, #21981 ),
 .UNSPECIFIED., .F., .F.,
 ( 4, 2, 2, 2, 2, 2, 2, 2, 2, 2, 2, 2, 2, 2, 2, 2, 2, 2, 2, 2, 2, 2, 2, 2, 2, 2, 2, 2, 2, 2, 2, 2, 2, 2, 2, 2, 2, 2, 2, 2, 2, 2, 2, 2, 2, 2, 2, 2, 2, 2, 2, 2, 2, 2, 2, 2, 2, 2, 2, 2, 2, 2, 2, 2, 2, 2, 2, 2, 2, 2, 2, 2, 2, 2, 2, 2, 2, 2, 4 ),
 ( 0.000000000000000000, 0.005381740036788157898, 0.008072610055182236413, 0.009418045064379276105, 0.01009076256897779508, 0.01076348007357631580, 0.01185104180586291078, 0.01293860353814950404, 0.01511372700272269054, 0.01946397393186906355, 0.02816446779016181304, 0.04556545550674730855, 0.08036743093991829956, 0.1151694063730892975, 0.1325703940896748034, 0.1412708879479675494, 0.1456211348771139225, 0.1477962583416871090, 0.1488838200739737161, 0.1499713818062602955, 0.1507624401091536004, 0.1515534984120469053, 0.1531356150178334874, 0.1562998482294066793, 0.1626283146525530909, 0.1752852474988458864, 0.2005991131914315051, 0.2512268445766027147, 0.3018545759617738966, 0.3271684416543594875, 0.3398253745006523108, 0.3461538409237986946, 0.3493180741353718588, 0.3509001907411584686, 0.3524823073469450785, 0.3548354025267266287, 0.3571884977065081790, 0.3618946880660712795, 0.3713070687851974805, 0.3901318302234498825, 0.4277813530999547420, 0.4654308759764596015, 0.4842556374147120035, 0.4936680181338382045, 0.4983742084934013050, 0.5007273036731828553, 0.5030803988529644055, 0.5053274392295320494, 0.5075744796060996933, 0.5120685603592350921, 0.5210567218655057786, 0.5390330448780472627, 0.5749856909031301200, 0.6109383369282129772, 0.6289146599407544613, 0.6379028214470251479, 0.6423969022001605467, 0.6446439425767281906, 0.6468909829532958344, 0.6492440781330773847, 0.6515971733128589349, 0.6563033636724220354, 0.6657157443915482364, 0.6845405058298006384, 0.7221900287063054424, 0.7598395515828102464, 0.7786643130210626484, 0.7880766937401888494, 0.7927828840997519499, 0.7951359792795336112, 0.7974890744593151615, 0.7990711910651018268, 0.8006533076708883812, 0.8038175408824614898, 0.8101460073056079292, 0.8228029401519008079, 0.8481168058444863433, 0.8987445372296576362, 1.000000000000000000 ),
 .UNSPECIFIED. ) ;
#9960 = CARTESIAN_POINT ( 'NONE',  ( -35.50000000000000711, -114.1489256397697289, 9.518467544735724317 ) ) ;
#9961 = DIRECTION ( 'NONE',  ( -0.000000000000000000, -0.000000000000000000, -1.000000000000000000 ) ) ;
#9962 = EDGE_CURVE ( 'NONE', #20326, #24108, #35073, .T. ) ;
#9963 = EDGE_LOOP ( 'NONE', ( #945, #34378, #9754, #25206 ) ) ;
#9964 = DIRECTION ( 'NONE',  ( -1.000000000000000000, 0.000000000000000000, 0.000000000000000000 ) ) ;
#9965 = CARTESIAN_POINT ( 'NONE',  ( -34.50000000000000000, -117.0140978167138854, -0.3122823525984416704 ) ) ;
#9966 = DIRECTION ( 'NONE',  ( 0.000000000000000000, 0.000000000000000000, 1.000000000000000000 ) ) ;
#9967 = ORIENTED_EDGE ( 'NONE', *, *, #14172, .T. ) ;
#9968 = ORIENTED_EDGE ( 'NONE', *, *, #34122, .F. ) ;
#9969 = CARTESIAN_POINT ( 'NONE',  ( -36.94073759706868287, -115.0000000000000000, 8.871475545821548181 ) ) ;
#9970 = SURFACE_STYLE_FILL_AREA ( #20389 ) ;
#9971 = ORIENTED_EDGE ( 'NONE', *, *, #7741, .T. ) ;
#9972 = ORIENTED_EDGE ( 'NONE', *, *, #15213, .T. ) ;
#9973 = CARTESIAN_POINT ( 'NONE',  ( -34.50000000000000000, -113.1981689815712997, 0.8971895242272823756 ) ) ;
#9974 = CIRCLE ( 'NONE', #28943, 4.000000000000003553 ) ;
#9975 = CARTESIAN_POINT ( 'NONE',  ( 3.799999999999999822, 0.000000000000000000, 36.00000000000000000 ) ) ;
#9976 = EDGE_CURVE ( 'NONE', #26571, #28899, #7595, .T. ) ;
#9977 = CARTESIAN_POINT ( 'NONE',  ( 0.000000000000000000, -9.604183132802312173, -5.908880290975638161 ) ) ;
#9978 = EDGE_CURVE ( 'NONE', #17384, #33209, #25859, .T. ) ;
#9979 = VECTOR ( 'NONE', #5244, 1000.000000000000000 ) ;
#9980 = CARTESIAN_POINT ( 'NONE',  ( -35.50000000000000000, -113.9948283797722439, 10.50648163149984171 ) ) ;
#9981 = AXIS2_PLACEMENT_3D ( 'NONE', #3753, #22996, #25542 ) ;
#9982 = EDGE_CURVE ( 'NONE', #30739, #24774, #28114, .T. ) ;
#9983 = CARTESIAN_POINT ( 'NONE',  ( 4.000000000000003553, 18.53613841426857789, -48.58406706613882875 ) ) ;
#9984 = CARTESIAN_POINT ( 'NONE',  ( -36.01562499999996447, -114.9929510916434339, 14.11852480586264846 ) ) ;
#9985 = LINE ( 'NONE', #12513, #18004 ) ;
#9986 = EDGE_CURVE ( 'NONE', #27576, #485, #33325, .T. ) ;
#9987 = FACE_OUTER_BOUND ( 'NONE', #28604, .T. ) ;
#9988 = ORIENTED_EDGE ( 'NONE', *, *, #13368, .T. ) ;
#9989 = CARTESIAN_POINT ( 'NONE',  ( -35.50000000000000000, -115.9929510916434481, 12.53051367006571581 ) ) ;
#9990 = LINE ( 'NONE', #20951, #12497 ) ;
#9991 = EDGE_CURVE ( 'NONE', #10771, #4384, #17788, .T. ) ;
#9992 = LINE ( 'NONE', #4085, #15223 ) ;
#9993 = DIRECTION ( 'NONE',  ( -1.000000000000000000, 0.000000000000000000, 0.000000000000000000 ) ) ;
#9994 = CIRCLE ( 'NONE', #34732, 4.999999999999990230 ) ;
#9995 = ORIENTED_EDGE ( 'NONE', *, *, #24145, .F. ) ;
#9996 = DIRECTION ( 'NONE',  ( -1.000000000000000000, -0.000000000000000000, -0.000000000000000000 ) ) ;
#9997 = FACE_OUTER_BOUND ( 'NONE', #8401, .T. ) ;
#9998 = DIRECTION ( 'NONE',  ( 0.000000000000000000, -0.4817536741017037771, -0.8763066800438699122 ) ) ;
#9999 = DIRECTION ( 'NONE',  ( -1.000000000000000000, -0.000000000000000000, 0.000000000000000000 ) ) ;
#10000 = ORIENTED_EDGE ( 'NONE', *, *, #11236, .T. ) ;
#10001 = CARTESIAN_POINT ( 'NONE',  ( -37.97545270896701908, -113.5265240346955977, 6.847274454178448266 ) ) ;
#10002 = DIRECTION ( 'NONE',  ( 1.000000000000000000, 0.000000000000000000, 0.000000000000000000 ) ) ;
#10003 = DIRECTION ( 'NONE',  ( 1.000000000000000000, -0.000000000000000000, 0.000000000000000000 ) ) ;
#10004 = VERTEX_POINT ( 'NONE', #11896 ) ;
#10005 = ORIENTED_EDGE ( 'NONE', *, *, #11253, .F. ) ;
#10006 = AXIS2_PLACEMENT_3D ( 'NONE', #347, #11343, #19594 ) ;
#10007 = PRESENTATION_STYLE_ASSIGNMENT (( #20614 ) ) ;
#10008 = AXIS2_PLACEMENT_3D ( 'NONE', #28285, #24389, #19319 ) ;
#10009 = CARTESIAN_POINT ( 'NONE',  ( -42.49999999999999289, -31.68172400785665488, 97.87435565298206086 ) ) ;
#10010 = VERTEX_POINT ( 'NONE', #731 ) ;
#10011 = CARTESIAN_POINT ( 'NONE',  ( -36.94073759706868287, -116.9999999999999858, 8.871475545821548181 ) ) ;
#10012 = VERTEX_POINT ( 'NONE', #6980 ) ;
#10013 = FILL_AREA_STYLE_COLOUR ( '', #32253 ) ;
#10014 = ORIENTED_EDGE ( 'NONE', *, *, #15774, .T. ) ;
#10015 = ORIENTED_EDGE ( 'NONE', *, *, #6570, .F. ) ;
#10016 = CARTESIAN_POINT ( 'NONE',  ( 8.000000000000000000, -19.60123832284022072, 3.973846525876368219 ) ) ;
#10017 = LINE ( 'NONE', #9835, #32121 ) ;
#10018 = EDGE_CURVE ( 'NONE', #34251, #14155, #30984, .T. ) ;
#10019 = DIRECTION ( 'NONE',  ( 1.000000000000000000, -5.339440136655842133E-16, -1.047965281155519420E-16 ) ) ;
#10020 = ORIENTED_EDGE ( 'NONE', *, *, #24468, .F. ) ;
#10021 = ORIENTED_EDGE ( 'NONE', *, *, #20988, .F. ) ;
#10022 = CIRCLE ( 'NONE', #14602, 3.799999999999999822 ) ;
#10023 = EDGE_CURVE ( 'NONE', #24725, #19376, #11191, .T. ) ;
#10024 = DIRECTION ( 'NONE',  ( 0.000000000000000000, 0.000000000000000000, 1.000000000000000000 ) ) ;
#10025 = DIRECTION ( 'NONE',  ( 0.9995917534020517525, -0.02857142857142376188, -1.185676054145132037E-15 ) ) ;
#10026 = ORIENTED_EDGE ( 'NONE', *, *, #14824, .T. ) ;
#10027 = CARTESIAN_POINT ( 'NONE',  ( 0.000000000000000000, 31.08872492059957793, 41.68322423723111569 ) ) ;
#10028 = DIRECTION ( 'NONE',  ( 0.000000000000000000, 0.000000000000000000, 1.000000000000000000 ) ) ;
#10029 = FACE_OUTER_BOUND ( 'NONE', #33976, .T. ) ;
#10030 = CIRCLE ( 'NONE', #7736, 20.00000000000000711 ) ;
#10031 = CARTESIAN_POINT ( 'NONE',  ( -34.50000000000000000, -115.9929510916434481, 12.60752341388803721 ) ) ;
#10032 = AXIS2_PLACEMENT_3D ( 'NONE', #23958, #26839, #35304 ) ;
#10033 = LINE ( 'NONE', #1760, #17459 ) ;
#10034 = CARTESIAN_POINT ( 'NONE',  ( -35.02454729103298092, -114.8876895276775087, 6.097274454178449155 ) ) ;
#10035 = CARTESIAN_POINT ( 'NONE',  ( -34.50000000000000000, -115.9929510916434481, 12.60752341388803721 ) ) ;
#10036 = CYLINDRICAL_SURFACE ( 'NONE', #32595, 14.70000000000000107 ) ;
#10037 = CYLINDRICAL_SURFACE ( 'NONE', #33968, 20.00000000000000355 ) ;
#10038 = DIRECTION ( 'NONE',  ( 1.000000000000000000, -0.000000000000000000, 0.000000000000000000 ) ) ;
#10039 = CARTESIAN_POINT ( 'NONE',  ( 0.000000000000000000, 0.000000000000000000, 60.90000000000001279 ) ) ;
#10040 = CARTESIAN_POINT ( 'NONE',  ( 8.000000000000000000, 17.06000345190438594, 10.43821259704026794 ) ) ;
#10041 = ORIENTED_EDGE ( 'NONE', *, *, #11042, .F. ) ;
#10042 = CARTESIAN_POINT ( 'NONE',  ( -36.11231047232249125, -115.9754527089670262, 2.777725545821550845 ) ) ;
#10043 = CARTESIAN_POINT ( 'NONE',  ( 65.00000000000001421, 54.25778039068027425, 73.39034659349927381 ) ) ;
#10044 = CARTESIAN_POINT ( 'NONE',  ( -35.50000000000000000, -113.0140978167140702, 0.8752176474015603835 ) ) ;
#10045 = ORIENTED_EDGE ( 'NONE', *, *, #16927, .T. ) ;
#10046 = VERTEX_POINT ( 'NONE', #28290 ) ;
#10047 = CARTESIAN_POINT ( 'NONE',  ( 55.00000000000000000, -25.98076211353320275, 84.99999999999994316 ) ) ;
#10048 = FACE_OUTER_BOUND ( 'NONE', #1081, .T. ) ;
#10049 = EDGE_LOOP ( 'NONE', ( #8844, #29713, #18211, #11777 ) ) ;
#10050 = ORIENTED_EDGE ( 'NONE', *, *, #6214, .F. ) ;
#10051 = ORIENTED_EDGE ( 'NONE', *, *, #2954, .T. ) ;
#10052 = AXIS2_PLACEMENT_3D ( 'NONE', #14681, #25695, #6585 ) ;
#10053 = CARTESIAN_POINT ( 'NONE',  ( 46.00000000000000000, 0.000000000000000000, 70.00000000000000000 ) ) ;
#10054 = AXIS2_PLACEMENT_3D ( 'NONE', #32937, #28244, #3584 ) ;
#10055 = DIRECTION ( 'NONE',  ( 0.000000000000000000, 0.000000000000000000, 1.000000000000000000 ) ) ;
#10056 = DIRECTION ( 'NONE',  ( 0.000000000000000000, 0.000000000000000000, -1.000000000000000000 ) ) ;
#10057 = AXIS2_PLACEMENT_3D ( 'NONE', #32193, #7520, #18499 ) ;
#10058 = DIRECTION ( 'NONE',  ( -1.000000000000000000, -0.000000000000000000, -0.000000000000000000 ) ) ;
#10059 = ORIENTED_EDGE ( 'NONE', *, *, #32301, .T. ) ;
#10060 = ORIENTED_EDGE ( 'NONE', *, *, #6659, .T. ) ;
#10061 = CARTESIAN_POINT ( 'NONE',  ( -35.50000000000000000, -117.0140978167138854, 0.8752176474015623819 ) ) ;
#10062 = AXIS2_PLACEMENT_3D ( 'NONE', #22094, #5551, #27524 ) ;
#10063 = EDGE_CURVE ( 'NONE', #9746, #29518, #22952, .T. ) ;
#10064 = CARTESIAN_POINT ( 'NONE',  ( 8.000000000000007105, 0.000000000000000000, 0.000000000000000000 ) ) ;
#10065 = DIRECTION ( 'NONE',  ( 0.000000000000000000, 0.5877852522924685852, 0.8090169943749506709 ) ) ;
#10066 = VERTEX_POINT ( 'NONE', #33868 ) ;
#10067 = CYLINDRICAL_SURFACE ( 'NONE', #7458, 6.000000000000005329 ) ;
#10068 = AXIS2_PLACEMENT_3D ( 'NONE', #21984, #16585, #32981 ) ;
#10069 = LINE ( 'NONE', #1982, #16124 ) ;
#10070 = CARTESIAN_POINT ( 'NONE',  ( -34.50000000000000000, -114.9929510916434339, 12.39849696637031506 ) ) ;
#10071 = DIRECTION ( 'NONE',  ( 0.000000000000000000, -0.5877852522924802425, 0.8090169943749421222 ) ) ;
#10072 = CARTESIAN_POINT ( 'NONE',  ( -35.52552712174884419, -114.9929510916434339, 12.77960891308624447 ) ) ;
#10073 = CARTESIAN_POINT ( 'NONE',  ( 0.000000000000000000, -36.06787431788650622, -37.45808914225528952 ) ) ;
#10074 = ADVANCED_FACE ( 'NONE', ( #22340 ), #33501, .T. ) ;
#10075 = CARTESIAN_POINT ( 'NONE',  ( -34.50000000000000000, -114.9929296450195721, 10.49869535309826674 ) ) ;
#10076 = CARTESIAN_POINT ( 'NONE',  ( 0.000000000000000000, 0.000000000000000000, 36.00000000000000000 ) ) ;
#10077 = DIRECTION ( 'NONE',  ( -1.174092375852890260E-15, 4.222049128630259891E-16, 1.000000000000000000 ) ) ;
#10078 = DIRECTION ( 'NONE',  ( 1.000000000000000000, -4.625929269271460867E-15, -1.174092375852883357E-15 ) ) ;
#10079 = ORIENTED_EDGE ( 'NONE', *, *, #10138, .T. ) ;
#10081 = CLOSED_SHELL ( 'NONE', ( #14335, #3369, #29311, #15692, #8201, #16052, #2291, #23787, #19167, #25612, #11330, #28969, #13259, #7778, #14679, #2943, #8884, #1335, #23807, #16766, #30406, #23101 ) ) ;
#10080 = PLANE ( 'NONE',  #29070 ) ;
#10082 = DIRECTION ( 'NONE',  ( 0.000000000000000000, 0.3090169943749412895, 0.9510565162951555296 ) ) ;
#10083 = AXIS2_PLACEMENT_3D ( 'NONE', #12525, #1192, #9815 ) ;
#10084 = VERTEX_POINT ( 'NONE', #16925 ) ;
#10085 = CARTESIAN_POINT ( 'NONE',  ( -36.31249999999995026, -114.9929510916434339, 13.11852480586264669 ) ) ;
#10086 = ORIENTED_EDGE ( 'NONE', *, *, #28853, .F. ) ;
#10087 = CARTESIAN_POINT ( 'NONE',  ( -37.05926240293131713, -115.9999999999999858, 4.878524454178449155 ) ) ;
#10088 = CARTESIAN_POINT ( 'NONE',  ( 0.000000000000000000, 31.08872492060014991, -41.68322423723069647 ) ) ;
#10089 = AXIS2_PLACEMENT_3D ( 'NONE', #25506, #28560, #3911 ) ;
#10090 = VERTEX_POINT ( 'NONE', #19977 ) ;
#10091 = ORIENTED_EDGE ( 'NONE', *, *, #463, .T. ) ;
#10092 = CARTESIAN_POINT ( 'NONE',  ( -34.50000000000000000, -113.0140978167138712, 0.7189676474015717078 ) ) ;
#10093 = CARTESIAN_POINT ( 'NONE',  ( 0.000000000000000000, 0.000000000000000000, 0.000000000000000000 ) ) ;
#10094 = VERTEX_POINT ( 'NONE', #22685 ) ;
#10095 = CARTESIAN_POINT ( 'NONE',  ( -39.99999999999999289, -113.9407375970686758, 3.753524454178448710 ) ) ;
#10096 = CIRCLE ( 'NONE', #14677, 8.000000000000007105 ) ;
#10097 = DIRECTION ( 'NONE',  ( 1.000000000000000000, -0.000000000000000000, -0.000000000000000000 ) ) ;
#10098 = DIRECTION ( 'NONE',  ( 0.000000000000000000, 0.8660254037844362651, 0.5000000000000042188 ) ) ;
#10099 = VERTEX_POINT ( 'NONE', #17107 ) ;
#10100 = ORIENTED_EDGE ( 'NONE', *, *, #13770, .F. ) ;
#10101 = DIRECTION ( 'NONE',  ( 0.000000000000000000, -0.5877852522924796874, 0.8090169943749426773 ) ) ;
#10102 = DIRECTION ( 'NONE',  ( 0.000000000000000000, -1.000000000000000000, 0.000000000000000000 ) ) ;
#10103 = ORIENTED_EDGE ( 'NONE', *, *, #11056, .F. ) ;
#10104 = EDGE_LOOP ( 'NONE', ( #30028, #9148, #14033, #26872 ) ) ;
#10105 = CARTESIAN_POINT ( 'NONE',  ( -34.50000000000000000, -112.7530559548648341, -2.608751991713152307 ) ) ;
#10106 = EDGE_CURVE ( 'NONE', #8056, #11602, #28728, .T. ) ;
#10107 = PRODUCT_DEFINITION_SHAPE ( 'NONE', 'NONE',  #35623 ) ;
#10108 = CIRCLE ( 'NONE', #25042, 3.999999999999996447 ) ;
#10109 = EDGE_CURVE ( 'NONE', #10620, #32703, #30459, .T. ) ;
#10110 = LINE ( 'NONE', #15139, #8154 ) ;
#10111 = ORIENTED_EDGE ( 'NONE', *, *, #16990, .T. ) ;
#10112 = ORIENTED_EDGE ( 'NONE', *, *, #20685, .F. ) ;
#10113 = DIRECTION ( 'NONE',  ( -1.000000000000000000, 0.000000000000000000, 0.000000000000000000 ) ) ;
#10114 = CIRCLE ( 'NONE', #26229, 22.00000000000000000 ) ;
#10115 = VECTOR ( 'NONE', #3764, 1000.000000000000000 ) ;
#10116 = CARTESIAN_POINT ( 'NONE',  ( -38.00000000000000711, -113.9929510916434339, 11.73841344789285657 ) ) ;
#10117 = CARTESIAN_POINT ( 'NONE',  ( 115.0000000000000000, 81.48267994499606459, 34.65054357219658243 ) ) ;
#10118 = ADVANCED_FACE ( 'NONE', ( #22162 ), #14582, .T. ) ;
#10119 = CARTESIAN_POINT ( 'NONE',  ( -34.50000000000000000, -113.9186338266397058, 10.49738657667399266 ) ) ;
#10120 =( GEOMETRIC_REPRESENTATION_CONTEXT ( 3 ) GLOBAL_UNCERTAINTY_ASSIGNED_CONTEXT ( ( #957 ) ) GLOBAL_UNIT_ASSIGNED_CONTEXT ( ( #30348, #3510, #14458 ) ) REPRESENTATION_CONTEXT ( 'NONE', 'WORKASPACE' ) );
#10121 = ADVANCED_FACE ( 'NONE', ( #14057 ), #22872, .T. ) ;
#10122 = CARTESIAN_POINT ( 'NONE',  ( -35.99386409314529800, -115.9929510916434481, 13.11852378322482515 ) ) ;
#10123 = VECTOR ( 'NONE', #22469, 1000.000000000000000 ) ;
#10124 = DIRECTION ( 'NONE',  ( -1.000000000000000000, 0.000000000000000000, 0.000000000000000000 ) ) ;
#10125 = FACE_OUTER_BOUND ( 'NONE', #4817, .T. ) ;
#10126 = ORIENTED_EDGE ( 'NONE', *, *, #24273, .T. ) ;
#10127 = LINE ( 'NONE', #21093, #14231 ) ;
#10128 = CARTESIAN_POINT ( 'NONE',  ( 8.000000000000000000, 0.000000000000000000, 0.000000000000000000 ) ) ;
#10129 = CARTESIAN_POINT ( 'NONE',  ( -3.799999999999999822, 4.653657836759942730E-16, -31.10000000000000142 ) ) ;
#10130 = ORIENTED_EDGE ( 'NONE', *, *, #3298, .T. ) ;
#10131 = DIRECTION ( 'NONE',  ( -1.000000000000000000, 0.000000000000000000, 0.000000000000000000 ) ) ;
#10132 = AXIS2_PLACEMENT_3D ( 'NONE', #29939, #27601, #16591 ) ;
#10133 = CARTESIAN_POINT ( 'NONE',  ( -35.50000000000000711, -112.5103839485166333, -1.498529437127682495 ) ) ;
#10134 = DIRECTION ( 'NONE',  ( 0.000000000000000000, 0.000000000000000000, 1.000000000000000000 ) ) ;
#10135 = DIRECTION ( 'NONE',  ( -1.000000000000000000, 0.000000000000000000, 0.000000000000000000 ) ) ;
#10136 = DIRECTION ( 'NONE',  ( -0.000000000000000000, 0.000000000000000000, -1.000000000000000000 ) ) ;
#10137 = AXIS2_PLACEMENT_3D ( 'NONE', #18579, #29754, #26884 ) ;
#10138 = EDGE_CURVE ( 'NONE', #30069, #23788, #558, .T. ) ;
#10139 = VECTOR ( 'NONE', #29317, 1000.000000000000000 ) ;
#10140 = ORIENTED_EDGE ( 'NONE', *, *, #12517, .F. ) ;
#10141 = DIRECTION ( 'NONE',  ( 0.000000000000000000, 0.000000000000000000, -1.000000000000000000 ) ) ;
#10142 = CARTESIAN_POINT ( 'NONE',  ( -35.50000000000000000, -111.0141141789186605, -0.6738694770610589302 ) ) ;
#10143 = FACE_OUTER_BOUND ( 'NONE', #19519, .T. ) ;
#10144 = VERTEX_POINT ( 'NONE', #25238 ) ;
#10145 = ORIENTED_EDGE ( 'NONE', *, *, #3496, .T. ) ;
#10146 = CARTESIAN_POINT ( 'NONE',  ( -39.02454729103295961, -114.7691647218148745, 2.159774454178448710 ) ) ;
#10147 = CIRCLE ( 'NONE', #26270, 20.00000000000000711 ) ;
#10148 =( LENGTH_UNIT ( ) NAMED_UNIT ( * ) SI_UNIT ( .MILLI., .METRE. ) );
#10149 = AXIS2_PLACEMENT_3D ( 'NONE', #8043, #291, #8217 ) ;
#10150 = LINE ( 'NONE', #1211, #25025 ) ;
#10151 = ORIENTED_EDGE ( 'NONE', *, *, #34154, .F. ) ;
#10152 = VERTEX_POINT ( 'NONE', #11546 ) ;
#10153 = CARTESIAN_POINT ( 'NONE',  ( -34.50000000000000000, -113.0140978167137860, 0.8752176474016654106 ) ) ;
#10154 = EDGE_CURVE ( 'NONE', #10339, #8680, #14910, .T. ) ;
#10155 = EDGE_CURVE ( 'NONE', #29894, #15796, #27765, .T. ) ;
#10156 = EDGE_CURVE ( 'NONE', #2175, #30986, #32734, .T. ) ;
#10157 = DIRECTION ( 'NONE',  ( 1.000000000000000000, 0.000000000000000000, 0.000000000000000000 ) ) ;
#10158 = DIRECTION ( 'NONE',  ( 0.000000000000000000, 0.000000000000000000, -1.000000000000000000 ) ) ;
#10159 = CIRCLE ( 'NONE', #18760, 19.99999999999998579 ) ;
#10160 = AXIS2_PLACEMENT_3D ( 'NONE', #14241, #14944, #4001 ) ;
#10161 = CARTESIAN_POINT ( 'NONE',  ( -35.50000000000000000, -113.9743717753924699, 10.50403980422039396 ) ) ;
#10162 = DIRECTION ( 'NONE',  ( -1.000000000000000000, 0.000000000000000000, 0.000000000000000000 ) ) ;
#10163 = EDGE_CURVE ( 'NONE', #5508, #16891, #29300, .T. ) ;
#10164 = CARTESIAN_POINT ( 'NONE',  ( -34.50000000000000000, -112.0140978167138712, -0.1247823525984259746 ) ) ;
#10165 = EDGE_CURVE ( 'NONE', #966, #27135, #22387, .T. ) ;
#10166 = CARTESIAN_POINT ( 'NONE',  ( -37.24999999999992895, -114.9929510916434339, 14.11852480586264846 ) ) ;
#10167 = CARTESIAN_POINT ( 'NONE',  ( 0.000000000000000000, 3.678165988948591814, 15.05623113391068379 ) ) ;
#10168 = AXIS2_PLACEMENT_3D ( 'NONE', #25831, #12128, #1504 ) ;
#10169 = VECTOR ( 'NONE', #16839, 1000.000000000000000 ) ;
#10170 = DIRECTION ( 'NONE',  ( -1.000000000000000000, 0.000000000000000000, 0.000000000000000000 ) ) ;
#10171 = VERTEX_POINT ( 'NONE', #15246 ) ;
#10172 = CARTESIAN_POINT ( 'NONE',  ( -35.97955704204053262, -115.9929510916434481, 13.11812344617474402 ) ) ;
#10173 = DIRECTION ( 'NONE',  ( -1.000000000000000000, 0.000000000000000000, 0.000000000000000000 ) ) ;
#10174 = CARTESIAN_POINT ( 'NONE',  ( -90.00000000000002842, 1.346812405055736621E-15, 7.020000000000052864 ) ) ;
#10175 = AXIS2_PLACEMENT_3D ( 'NONE', #6863, #17835, #12446 ) ;
#10176 = CARTESIAN_POINT ( 'NONE',  ( 1.479000000000007642, 9.623377526722998283E-16, 5.016000000000010672 ) ) ;
#10177 = DIRECTION ( 'NONE',  ( 0.000000000000000000, 0.000000000000000000, -1.000000000000000000 ) ) ;
#10178 = AXIS2_PLACEMENT_3D ( 'NONE', #20777, #7113, #7471 ) ;
#10179 = ORIENTED_EDGE ( 'NONE', *, *, #5772, .T. ) ;
#10180 = CARTESIAN_POINT ( 'NONE',  ( 65.00000000000001421, 81.48267994499606459, 22.65054357219659664 ) ) ;
#10181 = FACE_OUTER_BOUND ( 'NONE', #1266, .T. ) ;
#10182 = CARTESIAN_POINT ( 'NONE',  ( -3.799999999999999822, 4.653657836759942730E-16, -53.39999999999999858 ) ) ;
#10183 = DIRECTION ( 'NONE',  ( -1.000000000000000000, 0.000000000000000000, 0.000000000000000000 ) ) ;
#10184 = CARTESIAN_POINT ( 'NONE',  ( -37.35495115944176092, -112.9754527089670688, 7.034774454178450043 ) ) ;
#10185 = CARTESIAN_POINT ( 'NONE',  ( -34.49999999999998579, -25.98076211353322051, 84.99999999999992895 ) ) ;
#10186 = MANIFOLD_SOLID_BREP ( 'Mirror1', #19244 ) ;
#10187 = FACE_OUTER_BOUND ( 'NONE', #30304, .T. ) ;
#10188 = ADVANCED_FACE ( 'NONE', ( #21368 ), #10231, .T. ) ;
#10189 = ORIENTED_EDGE ( 'NONE', *, *, #23890, .F. ) ;
#10190 = AXIS2_PLACEMENT_3D ( 'NONE', #33288, #25004, #8604 ) ;
#10191 = ORIENTED_EDGE ( 'NONE', *, *, #19121, .T. ) ;
#10192 = CARTESIAN_POINT ( 'NONE',  ( -34.49999999999998579, -38.78532556477436088, 79.33933265213893549 ) ) ;
#10193 = AXIS2_PLACEMENT_3D ( 'NONE', #28320, #414, #8520 ) ;
#10194 = EDGE_CURVE ( 'NONE', #33932, #1954, #10580, .T. ) ;
#10195 = DIRECTION ( 'NONE',  ( -1.000000000000000000, 0.000000000000000000, 0.000000000000000000 ) ) ;
#10196 = ORIENTED_EDGE ( 'NONE', *, *, #10564, .T. ) ;
#10197 = CARTESIAN_POINT ( 'NONE',  ( -37.76916472181486739, -116.0245472910329880, 5.965225545821550845 ) ) ;
#10198 = EDGE_LOOP ( 'NONE', ( #3655, #8531 ) ) ;
#10199 = AXIS2_PLACEMENT_3D ( 'NONE', #14629, #33913, #28160 ) ;
#10200 =( LENGTH_UNIT ( ) NAMED_UNIT ( * ) SI_UNIT ( .MILLI., .METRE. ) );
#10201 = EDGE_LOOP ( 'NONE', ( #15532, #15346, #8655, #15112 ) ) ;
#10202 = ORIENTED_EDGE ( 'NONE', *, *, #29807, .T. ) ;
#10203 = VECTOR ( 'NONE', #14957, 1000.000000000000000 ) ;
#10204 = DIRECTION ( 'NONE',  ( -1.783119874454246424E-31, -1.187911941725854497E-31, 1.000000000000000000 ) ) ;
#10205 = CIRCLE ( 'NONE', #16508, 15.49899999999998279 ) ;
#10206 = EDGE_CURVE ( 'NONE', #19029, #17795, #1595, .T. ) ;
#10207 =( GEOMETRIC_REPRESENTATION_CONTEXT ( 3 ) GLOBAL_UNCERTAINTY_ASSIGNED_CONTEXT ( ( #9232 ) ) GLOBAL_UNIT_ASSIGNED_CONTEXT ( ( #1733, #4449, #12718 ) ) REPRESENTATION_CONTEXT ( 'NONE', 'WORKASPACE' ) );
#10208 = EDGE_CURVE ( 'NONE', #3289, #16353, #24161, .T. ) ;
#10209 = CARTESIAN_POINT ( 'NONE',  ( 0.000000000000000000, 0.000000000000000000, -40.89999999999999858 ) ) ;
#10210 = ORIENTED_EDGE ( 'NONE', *, *, #23855, .F. ) ;
#10211 = ORIENTED_EDGE ( 'NONE', *, *, #12600, .T. ) ;
#10212 = DIRECTION ( 'NONE',  ( -1.000000000000000000, 0.000000000000000000, 0.000000000000000000 ) ) ;
#10213 = DIRECTION ( 'NONE',  ( 1.000000000000000000, -5.339440136655842133E-16, -1.047965281155519420E-16 ) ) ;
#10214 = VERTEX_POINT ( 'NONE', #34719 ) ;
#10215 = FACE_OUTER_BOUND ( 'NONE', #2989, .T. ) ;
#10216 = AXIS2_PLACEMENT_3D ( 'NONE', #35379, #24752, #33205 ) ;
#10217 = CARTESIAN_POINT ( 'NONE',  ( 8.000000000000000000, 0.000000000000000000, 0.000000000000000000 ) ) ;
#10218 = CYLINDRICAL_SURFACE ( 'NONE', #12109, 7.199999999999994849 ) ;
#10219 = CIRCLE ( 'NONE', #29199, 4.000000000000003553 ) ;
#10220 = DIRECTION ( 'NONE',  ( 1.000000000000000000, -4.528031003192420052E-15, -1.179290629824070178E-15 ) ) ;
#10221 = CARTESIAN_POINT ( 'NONE',  ( -36.94073759706868287, -112.0000000000000142, 8.628524454178448266 ) ) ;
#10222 = CARTESIAN_POINT ( 'NONE',  ( -34.50000000000000000, -114.7000328234681206, 8.631511418192262752 ) ) ;
#10223 = CYLINDRICAL_SURFACE ( 'NONE', #19943, 3.799999999999999822 ) ;
#10224 = AXIS2_PLACEMENT_3D ( 'NONE', #20990, #26424, #1755 ) ;
#10225 = CIRCLE ( 'NONE', #11379, 0.6000000000000028644 ) ;
#10226 = CYLINDRICAL_SURFACE ( 'NONE', #22431, 3.799999999999999822 ) ;
#10227 = VECTOR ( 'NONE', #13655, 1000.000000000000000 ) ;
#10228 = CARTESIAN_POINT ( 'NONE',  ( 7.999999999999992895, 0.000000000000000000, 0.000000000000000000 ) ) ;
#10229 = CARTESIAN_POINT ( 'NONE',  ( 8.000000000000000000, 0.5097555531873367851, 19.99350267651958291 ) ) ;
#10230 = DIRECTION ( 'NONE',  ( -1.226634733346697831E-16, 0.9659258262890646485, 0.2588190451025342842 ) ) ;
#10231 = CYLINDRICAL_SURFACE ( 'NONE', #31009, 8.000000000000003553 ) ;
#10232 = EDGE_LOOP ( 'NONE', ( #266, #5649, #2640, #1072 ) ) ;
#10233 = CARTESIAN_POINT ( 'NONE',  ( -38.37230871539094323, -115.4561184093552413, 3.058975545821551290 ) ) ;
#10234 = CIRCLE ( 'NONE', #1033, 19.99999999999999645 ) ;
#10235 = DIRECTION ( 'NONE',  ( -1.000000000000000000, 0.000000000000000000, 0.000000000000000000 ) ) ;
#10236 = DIRECTION ( 'NONE',  ( 0.000000000000000000, 0.5877852522924682521, 0.8090169943749511150 ) ) ;
#10237 = EDGE_CURVE ( 'NONE', #4138, #28129, #9161, .T. ) ;
#10238 = EDGE_LOOP ( 'NONE', ( #22498, #13339, #2422, #17755 ) ) ;
#10239 = VERTEX_POINT ( 'NONE', #18496 ) ;
#10240 = EDGE_CURVE ( 'NONE', #20113, #7164, #4834, .T. ) ;
#10241 = CARTESIAN_POINT ( 'NONE',  ( -55.00000000000000000, -25.98076211353320275, 78.99999999999992895 ) ) ;
#10242 = FACE_OUTER_BOUND ( 'NONE', #4560, .T. ) ;
#10243 = ORIENTED_EDGE ( 'NONE', *, *, #31569, .T. ) ;
#10244 = EDGE_LOOP ( 'NONE', ( #25621, #23956, #33085, #14672 ) ) ;
#10245 = ORIENTED_EDGE ( 'NONE', *, *, #33511, .F. ) ;
#10246 = AXIS2_PLACEMENT_3D ( 'NONE', #4037, #34455, #34087 ) ;
#10247 = DIRECTION ( 'NONE',  ( 0.000000000000000000, 0.000000000000000000, -1.000000000000000000 ) ) ;
#10248 = DIRECTION ( 'NONE',  ( 0.000000000000000000, -0.5000000000000067724, 0.8660254037844348218 ) ) ;
#10249 = CIRCLE ( 'NONE', #17709, 19.99999999999998579 ) ;
#10250 = VECTOR ( 'NONE', #14654, 1000.000000000000000 ) ;
#10251 = CIRCLE ( 'NONE', #30375, 7.199999999999990408 ) ;
#10252 = CARTESIAN_POINT ( 'NONE',  ( -45.00000000000000000, 0.000000000000000000, 70.00000000000000000 ) ) ;
#10253 = DIRECTION ( 'NONE',  ( 0.000000000000000000, 0.000000000000000000, 1.000000000000000000 ) ) ;
#10254 = VERTEX_POINT ( 'NONE', #15776 ) ;
#10255 = VERTEX_POINT ( 'NONE', #26794 ) ;
#10256 = CARTESIAN_POINT ( 'NONE',  ( -35.50000000000000711, -112.0140978167138712, -0.4685323525984295134 ) ) ;
#10257 = AXIS2_PLACEMENT_3D ( 'NONE', #19303, #19489, #8514 ) ;
#10258 = CYLINDRICAL_SURFACE ( 'NONE', #148, 7.199999999999993960 ) ;
#10259 = LINE ( 'NONE', #19050, #20090 ) ;
#10260 = EDGE_LOOP ( 'NONE', ( #32478, #15, #29778, #2444 ) ) ;
#10261 = AXIS2_PLACEMENT_3D ( 'NONE', #19245, #16552, #2898 ) ;
#10262 = DIRECTION ( 'NONE',  ( -1.000000000000000000, 0.000000000000000000, 0.000000000000000000 ) ) ;
#10263 = CARTESIAN_POINT ( 'NONE',  ( -34.50000000000000000, -112.0577668799241309, 1.173706424699810569 ) ) ;
#10264 = CARTESIAN_POINT ( 'NONE',  ( -34.50000000000000000, -114.9929510916434339, 10.53376102667243508 ) ) ;
#10265 = DIRECTION ( 'NONE',  ( -1.000000000000000000, 0.000000000000000000, 0.000000000000000000 ) ) ;
#10266 = CARTESIAN_POINT ( 'NONE',  ( -37.89983305244309975, -114.9929510916434339, 12.92579853460519246 ) ) ;
#10267 = DIRECTION ( 'NONE',  ( 0.000000000000000000, 0.000000000000000000, 1.000000000000000000 ) ) ;
#10268 = CARTESIAN_POINT ( 'NONE',  ( -34.50000000000000000, -114.0185793162512908, 9.502217742515812304 ) ) ;
#10269 = DIRECTION ( 'NONE',  ( -1.000000000000000000, 0.000000000000000000, 0.000000000000000000 ) ) ;
#10270 = CARTESIAN_POINT ( 'NONE',  ( -37.99359134332094357, -114.9929510916434339, 12.69998175888958158 ) ) ;
#10271 = FILL_AREA_STYLE ('',( #18707 ) ) ;
#10272 = ORIENTED_EDGE ( 'NONE', *, *, #29104, .F. ) ;
#10273 = FACE_OUTER_BOUND ( 'NONE', #4906, .T. ) ;
#10274 = CARTESIAN_POINT ( 'NONE',  ( 0.000000000000000000, -47.49120266317495975, -0.8606222198180163430 ) ) ;
#10275 = ORIENTED_EDGE ( 'NONE', *, *, #16140, .T. ) ;
#10276 = CARTESIAN_POINT ( 'NONE',  ( -37.58145695302688694, -114.9929510916434339, 13.11211614918362756 ) ) ;
#10277 = EDGE_LOOP ( 'NONE', ( #33558, #26667 ) ) ;
#10278 = CIRCLE ( 'NONE', #35014, 15.49899999999999700 ) ;
#10279 = CARTESIAN_POINT ( 'NONE',  ( -38.97545270896704039, -113.1123104723225197, 8.347274454178448266 ) ) ;
#10280 = AXIS2_PLACEMENT_3D ( 'NONE', #17181, #9631, #3529 ) ;
#10281 = CARTESIAN_POINT ( 'NONE',  ( 0.000000000000000000, -2.710505431213761085E-17, 54.99999999999999289 ) ) ;
#10282 = ORIENTED_EDGE ( 'NONE', *, *, #25069, .F. ) ;
#10283 = VECTOR ( 'NONE', #14649, 1000.000000000000000 ) ;
#10284 = ORIENTED_EDGE ( 'NONE', *, *, #5523, .F. ) ;
#10285 = ADVANCED_FACE ( 'NONE', ( #2146 ), #13122, .T. ) ;
#10286 = CARTESIAN_POINT ( 'NONE',  ( 0.000000000000000000, -1.111908866155156161, 9.433698091065117808 ) ) ;
#10287 = ORIENTED_EDGE ( 'NONE', *, *, #24718, .T. ) ;
#10288 = AXIS2_PLACEMENT_3D ( 'NONE', #19958, #6298, #17266 ) ;
#10289 = CARTESIAN_POINT ( 'NONE',  ( -34.83677480945819838, -111.9205845034225462, 2.816024454178448710 ) ) ;
#10290 = DIRECTION ( 'NONE',  ( -1.000000000000000000, 0.000000000000000000, 0.000000000000000000 ) ) ;
#10291 = CARTESIAN_POINT ( 'NONE',  ( 0.000000000000000000, 0.000000000000000000, 65.00000000000000000 ) ) ;
#10292 = ORIENTED_EDGE ( 'NONE', *, *, #16558, .F. ) ;
#10293 = ORIENTED_EDGE ( 'NONE', *, *, #32391, .T. ) ;
#10294 = CARTESIAN_POINT ( 'NONE',  ( 0.000000000000000000, 0.000000000000000000, 0.000000000000000000 ) ) ;
#10295 = ADVANCED_FACE ( 'NONE', ( #12574 ), #5009, .T. ) ;
#10296 =( NAMED_UNIT ( * ) PLANE_ANGLE_UNIT ( ) SI_UNIT ( $, .RADIAN. ) );
#10297 = PLANE ( 'NONE',  #24780 ) ;
#10298 = ORIENTED_EDGE ( 'NONE', *, *, #2909, .T. ) ;
#10299 = VERTEX_POINT ( 'NONE', #13292 ) ;
#10300 = CARTESIAN_POINT ( 'NONE',  ( -34.50000000000000000, -113.6807644833805995, -2.624782352598442614 ) ) ;
#10301 = CARTESIAN_POINT ( 'NONE',  ( -46.00000000000000000, -25.98076211353320275, 84.99999999999992895 ) ) ;
#10302 = ORIENTED_EDGE ( 'NONE', *, *, #24516, .T. ) ;
#10303 = CARTESIAN_POINT ( 'NONE',  ( -35.50000000000000711, -114.5636144531578680, 9.676196722963288366 ) ) ;
#10304 = CIRCLE ( 'NONE', #13170, 14.00000000000000000 ) ;
#10305 = CARTESIAN_POINT ( 'NONE',  ( -34.50000000000000000, -113.9557924591415627, 10.50182206170499555 ) ) ;
#10306 =( BOUNDED_SURFACE ( )  B_SPLINE_SURFACE ( 3, 3, ( 
 ( #30180, #30534, #10921, #8904, #16652, #108, #11096, #22238, #5693, #2835, #8372, #22406, #27836, #460, #3174, #13794, #33235, #6218, #19355, #19691, #33401, #8724, #17000, #8554, #3004, #14305, #3360, #13964, #19525, #30708, #6039, #5864, #17178, #28010, #3527, #25306, #629, #11608, #22581, #21890, #32881, #8205, #19185, #5517, #34117, #29071, #14842, #4419, #22941, #14652, #3701, #33940, #31588, #6743, #26019, #4070, #20397, #31409, #25485, #17896, #9092, #6922, #17719, #6388, #28891, #25849, #803, #4243, #1348, #17353, #20763, #15182, #15014, #20050, #9440, #1174, #11977, #3885, #12150, #23122, #11783, #9271, #28717, #25665, #20224, #26189, #1525, #998, #12324, #22760, #31233, #23297, #9800, #18071, #28356, #12508, #6556, #17531, #33762, #34297, #9627, #28536, #31763, #31058, #20592, #23487, #7095, #34481, #10516, #24040, #29612, #10695, #23849, #13398, #18613, #26921, #27090, #15720, #26736, #12870, #13231, #2430, #24382, #34836, #29965, #4776, #26374, #20942, #15539, #21661, #1706, #5133, #7987, #31942, #16071, #2076, #7623, #12691, #23670, #13053, #7804, #29258, #2264, #32302, #18432, #35197, #35027, #21477, #35370, #10344, #4948, #21303, #15900, #24204, #32125, #21132, #32471, #18791 ),
 ( #34657, #32665, #7453, #4603, #26560, #29795, #10161, #7278, #1896, #18968, #15362, #9980, #18253, #29431, #2962, #25266, #13756, #25084, #5475, #8158, #588, #16428, #19492, #11574, #27626, #19826, #2607, #3313, #27449, #21843, #30495, #11223, #13923, #22190, #33535, #22021, #5824, #22544, #33191, #8863, #14266, #32836, #8518, #30320, #33016, #5307, #16785, #27795, #65, #24912, #3132, #16245, #14088, #10880, #235, #19139, #412, #27264, #11403, #22367, #27962, #11052, #13572, #30136, #16614, #24563, #8330, #35557, #5657, #2796, #33362, #8687, #19654, #24738, #19309, #30665, #5997, #16957, #23453, #6702, #17683, #1484, #34076, #14803, #9226, #6346, #950, #6882, #31015, #9588, #31372, #22903, #28145, #4027, #17312, #28850, #11743, #20556, #34255, #3487, #22721, #25448, #20182, #30837, #20009, #14437, #25809, #766, #28318, #11932, #31190, #28495, #17494, #4204, #3664, #33712, #9401, #1134, #3843, #12107, #34448, #33897, #28682, #26149, #23078, #12467, #15145, #9050, #20358, #6521, #14971, #9765, #25977, #1303, #25625, #12287, #23257, #6176, #31557, #14613, #17853, #17139, #4742, #13360, #7418, #26697, #7761, #15503, #18031, #9936, #32088, #29028, #26522, #27051, #10116, #26338, #2223, #13192 ),
 ( #32266, #1673, #16032, #24165, #10305, #15323, #15679, #21083, #7234, #34792, #18395, #29397, #7054, #4569, #2031, #20899, #1854, #10479, #35159, #31898, #13007, #24343, #12827, #23993, #5089, #35333, #12655, #21441, #18215, #23631, #4378, #34985, #21267, #34617, #2392, #29221, #7586, #23810, #20725, #29575, #15854, #18574, #4909, #31721, #26876, #18744, #32438, #29748, #22328, #11008, #21973, #8115, #8478, #33321, #8647, #30096, #25225, #22, #21614, #16203, #10839, #5953, #32615, #365, #3266, #27226, #11362, #32973, #2921, #7944, #18923, #8288, #3091, #24521, #33148, #27584, #13715, #30456, #11179, #5434, #30276, #22150, #29924, #16576, #2568, #19267, #13534, #5614, #14225, #13880, #24866, #19614, #16385, #5266, #35510, #194, #21797, #27403, #16910, #19455, #32794, #27750, #14044, #25041, #10656, #19096, #27916, #5785, #16742, #2754, #30617, #24694, #6834, #3794, #20142, #14566, #11700, #6302, #12244, #717, #14924, #1088, #28276, #33489, #9358, #22669, #34211, #17094, #25936, #3981, #8816, #28101, #30789, #25580, #547, #25403, #19778, #31148, #6130, #33660, #17271, #897, #33851, #22856, #20505, #11879, #17450, #9178, #6478, #23035, #3618, #28450, #20319, #14751, #30969, #19962, #28635, #3445 ),
 ( #8996, #25761, #12059, #14397, #34033, #31325, #6653, #17631, #1259, #23218, #9538, #31513, #17805, #28807, #4156, #15097, #11533, #22501, #4699, #32396, #12781, #5045, #23401, #24126, #12604, #7008, #15631, #32043, #34748, #7379, #18699, #7187, #26652, #21399, #18351, #7716, #35117, #17983, #29351, #15455, #18166, #10441, #1983, #34572, #10264, #26289, #28983, #29697, #1625, #12959, #26108, #23760, #1438, #34400, #12417, #23579, #4331, #23944, #34940, #10070, #21225, #9718, #29175, #32221, #20677, #7547, #31675, #15275, #9887, #18527, #26472, #4526, #20851, #29530, #4864, #31854, #21035, #15807, #1807, #26826, #2181, #13151, #18883, #16655, #8599, #2703, #21933, #3047, #10793, #13321, #5225, #27355, #24301, #21752, #22287, #5394, #21568, #33106, #8428, #19413, #19571, #2351, #11317, #11142, #32928, #30576, #27541, #2877, #33282, #19225, #10967, #30055, #27183, #32746, #27710, #16165, #30412, #16531, #8073, #35291, #24827, #2525, #14007, #32564, #5740, #16698, #10611, #7899, #29879, #16341, #15991, #13491, #24474, #8249, #35461, #19056, #13671, #24651, #30230, #5567, #325, #13839, #151, #22110, #25000, #27005, #22627, #11657, #14706, #6264, #675, #25361, #33995, #510, #852, #16873, #14888, #33620 ),
 ( #11487, #6087, #1225, #27877, #31284, #34172, #22458, #6611, #17228, #30932, #11834, #33450, #12204, #14185, #28234, #8772, #23177, #25719, #1052, #14521, #20102, #9495, #14354, #3942, #9140, #17405, #17583, #3574, #25539, #3407, #3751, #28590, #25898, #8953, #20455, #22814, #3223, #19739, #17053, #5909, #25188, #30752, #28066, #19917, #33815, #31109, #6436, #28408, #12023, #22993, #9321, #20277, #18308, #12740, #34529, #15586, #31813, #26608, #34708, #7334, #12917, #18123, #15233, #10699, #34896, #1580, #17943, #10031, #23716, #12375, #29974, #4292, #5311, #20995, #31633, #12562, #7992, #15415, #31467, #23903, #6969, #28944, #4476, #35562, #20810, #10885, #26242, #20634, #9679, #23535, #1943, #31998, #29306, #4656, #26428, #1758, #6794, #21667, #15060, #32671, #18974, #23352, #16251, #7148, #17765, #27269, #2611, #34351, #13576, #24568, #28767, #26070, #4119, #29127, #9845, #1399, #33197, #242, #8164, #5661, #11227, #22027, #16619, #11580, #593, #33021, #19496, #25452, #27631, #3139, #6184, #14443, #2801, #22548, #11058, #13760, #19144, #30142, #19832, #8335, #24744, #419, #27802, #30499, #14094, #770, #2970, #22371, #17144, #25088, #28149, #30843, #71, #11408, #22195, #13928, #3491, #33367 ),
 ( #8693, #27453, #8523, #19313, #5831, #21849, #16790, #19658, #8869, #24918, #5479, #30325, #30671, #16432, #6004, #32845, #16963, #27968, #3319, #14272, #25270, #33539, #33718, #7059, #6886, #28686, #4381, #23262, #34258, #18036, #14976, #31375, #25814, #22909, #17500, #23456, #11939, #26154, #12290, #3847, #9057, #20560, #33903, #9768, #28322, #1487, #15148, #20015, #3668, #6351, #1140, #11749, #955, #31019, #6705, #17317, #9231, #28499, #12114, #9405, #34080, #31728, #23084, #4032, #20364, #17687, #9591, #14809, #25984, #31560, #1306, #6524, #31194, #4209, #14619, #17859, #22726, #20730, #28856, #20189, #12471, #34451, #29033, #25629, #15326, #26342, #29579, #26882, #18578, #29226, #34990, #21618, #10122, #21445, #1860, #4572, #32620, #12832, #15860, #7949, #23999, #16209, #13196, #18750, #10311, #21087, #16037, #5097, #7422, #23814, #2229, #4916, #18218, #35337, #32093, #10662, #24169, #34799, #18399, #13365, #21271, #1676, #29752, #29401, #4746, #32270, #5270, #26702, #12658, #15683, #26526, #15506, #2038, #7767, #35163, #10484, #32442, #7591, #27055, #23635, #2397, #20904, #24347, #18930, #13014, #29929, #34622, #9941, #31904, #7237, #8122, #22506, #30625, #16748, #21804, #11184, #16582, #13722 ),
 ( #27592, #27410, #11016, #16917, #5958, #2759, #24875, #30798, #32978, #8483, #11540, #19783, #19104, #27925, #16392, #30101, #24526, #2927, #33154, #5439, #33496, #35514, #13885, #24702, #8822, #371, #22334, #200, #5791, #6138, #27, #25231, #30463, #3097, #3273, #22157, #19464, #21982, #25048, #14230, #553, #8293, #27230, #27757, #2572, #32801, #19274, #13539, #10845, #30282, #5621, #14050, #11367, #33329, #8652, #19619, #25410, #28456, #9547, #30976, #3987, #6310, #20324, #14402, #15105, #3626, #22862, #28813, #17276, #31518, #17638, #9186, #725, #25942, #28281, #26114, #33668, #6841, #20514, #11705, #9004, #22675, #6484, #17099, #14572, #19968, #12067, #25585, #906, #33859, #17457, #14758, #3801, #1444, #25766, #34038, #1095, #23040, #14932, #20147, #31153, #1264, #9365, #11885, #31332, #17813, #6660, #28641, #28108, #12426, #12250, #23223, #34216, #4163, #23410, #34407, #9724, #20686, #31681, #3451, #23954, #34579, #4706, #27012, #15464, #26834, #7193, #9893, #2358, #18173, #7015, #4532, #31861, #10270, #4337, #5053, #29184, #23587, #21233, #12966, #15637, #34949, #35300, #23767, #7555, #13328, #32229, #24308, #15998, #20859, #18534, #32050, #34755, #10618, #29538, #4871, #1813, #26660 ) ),
 .UNSPECIFIED., .T., .F., .T. ) 
 B_SPLINE_SURFACE_WITH_KNOTS ( ( 4, 3, 4 ),
 ( 4, 2, 2, 2, 2, 2, 2, 2, 2, 2, 2, 2, 2, 2, 2, 2, 2, 2, 2, 2, 2, 2, 2, 2, 2, 2, 2, 2, 2, 2, 2, 2, 2, 2, 2, 2, 2, 2, 2, 2, 2, 2, 2, 2, 2, 2, 2, 2, 2, 2, 2, 2, 2, 2, 2, 2, 2, 2, 2, 2, 2, 2, 2, 2, 2, 2, 2, 2, 2, 2, 2, 2, 2, 2, 2, 2, 2, 2, 4 ),
 ( 0.000000000000000000, 0.5000000000000000000, 1.000000000000000000 ),
 ( 0.000000000000000000, 0.005381740036788157898, 0.008072610055182236413, 0.009418045064379276105, 0.01009076256897779508, 0.01076348007357631580, 0.01185104180586291078, 0.01293860353814950404, 0.01511372700272269054, 0.01946397393186906355, 0.02816446779016181304, 0.04556545550674730855, 0.08036743093991829956, 0.1151694063730892975, 0.1325703940896748034, 0.1412708879479675494, 0.1456211348771139225, 0.1477962583416871090, 0.1488838200739737161, 0.1499713818062602955, 0.1507624401091536004, 0.1515534984120469053, 0.1531356150178334874, 0.1562998482294066793, 0.1626283146525530909, 0.1752852474988458864, 0.2005991131914315051, 0.2512268445766027147, 0.3018545759617738966, 0.3271684416543594875, 0.3398253745006523108, 0.3461538409237986946, 0.3493180741353718588, 0.3509001907411584686, 0.3524823073469450785, 0.3548354025267266287, 0.3571884977065081790, 0.3618946880660712795, 0.3713070687851974805, 0.3901318302234498825, 0.4277813530999547420, 0.4654308759764596015, 0.4842556374147120035, 0.4936680181338382045, 0.4983742084934013050, 0.5007273036731828553, 0.5030803988529644055, 0.5053274392295320494, 0.5075744796060996933, 0.5120685603592350921, 0.5210567218655057786, 0.5390330448780472627, 0.5749856909031301200, 0.6109383369282129772, 0.6289146599407544613, 0.6379028214470251479, 0.6423969022001605467, 0.6446439425767281906, 0.6468909829532958344, 0.6492440781330773847, 0.6515971733128589349, 0.6563033636724220354, 0.6657157443915482364, 0.6845405058298006384, 0.7221900287063054424, 0.7598395515828102464, 0.7786643130210626484, 0.7880766937401888494, 0.7927828840997519499, 0.7951359792795336112, 0.7974890744593151615, 0.7990711910651018268, 0.8006533076708883812, 0.8038175408824614898, 0.8101460073056079292, 0.8228029401519008079, 0.8481168058444863433, 0.8987445372296576362, 1.000000000000000000 ),
 .UNSPECIFIED. ) 
 GEOMETRIC_REPRESENTATION_ITEM ( )  RATIONAL_B_SPLINE_SURFACE ( (
 ( 1.000000000000000000, 1.000000000000000000, 1.000000000000000000, 1.000000000000000000, 1.000000000000000000, 1.000000000000000000, 1.000000000000000000, 1.000000000000000000, 1.000000000000000000, 1.000000000000000000, 1.000000000000000000, 1.000000000000000000, 1.000000000000000000, 1.000000000000000000, 1.000000000000000000, 1.000000000000000000, 1.000000000000000000, 1.000000000000000000, 1.000000000000000000, 1.000000000000000000, 1.000000000000000000, 1.000000000000000000, 1.000000000000000000, 1.000000000000000000, 1.000000000000000000, 1.000000000000000000, 1.000000000000000000, 1.000000000000000000, 1.000000000000000000, 1.000000000000000000, 1.000000000000000000, 1.000000000000000000, 1.000000000000000000, 1.000000000000000000, 1.000000000000000000, 1.000000000000000000, 1.000000000000000000, 1.000000000000000000, 1.000000000000000000, 1.000000000000000000, 1.000000000000000000, 1.000000000000000000, 1.000000000000000000, 1.000000000000000000, 1.000000000000000000, 1.000000000000000000, 1.000000000000000000, 1.000000000000000000, 1.000000000000000000, 1.000000000000000000, 1.000000000000000000, 1.000000000000000000, 1.000000000000000000, 1.000000000000000000, 1.000000000000000000, 1.000000000000000000, 1.000000000000000000, 1.000000000000000000, 1.000000000000000000, 1.000000000000000000, 1.000000000000000000, 1.000000000000000000, 1.000000000000000000, 1.000000000000000000, 1.000000000000000000, 1.000000000000000000, 1.000000000000000000, 1.000000000000000000, 1.000000000000000000, 1.000000000000000000, 1.000000000000000000, 1.000000000000000000, 1.000000000000000000, 1.000000000000000000, 1.000000000000000000, 1.000000000000000000, 1.000000000000000000, 1.000000000000000000, 1.000000000000000000, 1.000000000000000000, 1.000000000000000000, 1.000000000000000000, 1.000000000000000000, 1.000000000000000000, 1.000000000000000000, 1.000000000000000000, 1.000000000000000000, 1.000000000000000000, 1.000000000000000000, 1.000000000000000000, 1.000000000000000000, 1.000000000000000000, 1.000000000000000000, 1.000000000000000000, 1.000000000000000000, 1.000000000000000000, 1.000000000000000000, 1.000000000000000000, 1.000000000000000000, 1.000000000000000000, 1.000000000000000000, 1.000000000000000000, 1.000000000000000000, 1.000000000000000000, 1.000000000000000000, 1.000000000000000000, 1.000000000000000000, 1.000000000000000000, 1.000000000000000000, 1.000000000000000000, 1.000000000000000000, 1.000000000000000000, 1.000000000000000000, 1.000000000000000000, 1.000000000000000000, 1.000000000000000000, 1.000000000000000000, 1.000000000000000000, 1.000000000000000000, 1.000000000000000000, 1.000000000000000000, 1.000000000000000000, 1.000000000000000000, 1.000000000000000000, 1.000000000000000000, 1.000000000000000000, 1.000000000000000000, 1.000000000000000000, 1.000000000000000000, 1.000000000000000000, 1.000000000000000000, 1.000000000000000000, 1.000000000000000000, 1.000000000000000000, 1.000000000000000000, 1.000000000000000000, 1.000000000000000000, 1.000000000000000000, 1.000000000000000000, 1.000000000000000000, 1.000000000000000000, 1.000000000000000000, 1.000000000000000000, 1.000000000000000000, 1.000000000000000000, 1.000000000000000000, 1.000000000000000000, 1.000000000000000000, 1.000000000000000000, 1.000000000000000000, 1.000000000000000000, 1.000000000000000000, 1.000000000000000000, 1.000000000000000000, 1.000000000000000000, 1.000000000000000000, 1.000000000000000000, 1.000000000000000000),
 ( 0.3333333333333333703, 0.3333333333333333703, 0.3333333333333333703, 0.3333333333333333703, 0.3333333333333333703, 0.3333333333333333703, 0.3333333333333333703, 0.3333333333333333703, 0.3333333333333333703, 0.3333333333333333703, 0.3333333333333333703, 0.3333333333333333703, 0.3333333333333333703, 0.3333333333333333703, 0.3333333333333333703, 0.3333333333333333703, 0.3333333333333333703, 0.3333333333333333703, 0.3333333333333333703, 0.3333333333333333703, 0.3333333333333333703, 0.3333333333333333703, 0.3333333333333333703, 0.3333333333333333703, 0.3333333333333333703, 0.3333333333333333703, 0.3333333333333333703, 0.3333333333333333703, 0.3333333333333333703, 0.3333333333333333703, 0.3333333333333333703, 0.3333333333333333703, 0.3333333333333333703, 0.3333333333333333703, 0.3333333333333333703, 0.3333333333333333703, 0.3333333333333333703, 0.3333333333333333703, 0.3333333333333333703, 0.3333333333333333703, 0.3333333333333333703, 0.3333333333333333703, 0.3333333333333333703, 0.3333333333333333703, 0.3333333333333333703, 0.3333333333333333703, 0.3333333333333333703, 0.3333333333333333703, 0.3333333333333333703, 0.3333333333333333703, 0.3333333333333333703, 0.3333333333333333703, 0.3333333333333333703, 0.3333333333333333703, 0.3333333333333333703, 0.3333333333333333703, 0.3333333333333333703, 0.3333333333333333703, 0.3333333333333333703, 0.3333333333333333703, 0.3333333333333333703, 0.3333333333333333703, 0.3333333333333333703, 0.3333333333333333703, 0.3333333333333333703, 0.3333333333333333703, 0.3333333333333333703, 0.3333333333333333703, 0.3333333333333333703, 0.3333333333333333703, 0.3333333333333333703, 0.3333333333333333703, 0.3333333333333333703, 0.3333333333333333703, 0.3333333333333333703, 0.3333333333333333703, 0.3333333333333333703, 0.3333333333333333703, 0.3333333333333333703, 0.3333333333333333703, 0.3333333333333333703, 0.3333333333333333703, 0.3333333333333333703, 0.3333333333333333703, 0.3333333333333333703, 0.3333333333333333703, 0.3333333333333333703, 0.3333333333333333703, 0.3333333333333333703, 0.3333333333333333703, 0.3333333333333333703, 0.3333333333333333703, 0.3333333333333333703, 0.3333333333333333703, 0.3333333333333333703, 0.3333333333333333703, 0.3333333333333333703, 0.3333333333333333703, 0.3333333333333333703, 0.3333333333333333703, 0.3333333333333333703, 0.3333333333333333703, 0.3333333333333333703, 0.3333333333333333703, 0.3333333333333333703, 0.3333333333333333703, 0.3333333333333333703, 0.3333333333333333703, 0.3333333333333333703, 0.3333333333333333703, 0.3333333333333333703, 0.3333333333333333703, 0.3333333333333333703, 0.3333333333333333703, 0.3333333333333333703, 0.3333333333333333703, 0.3333333333333333703, 0.3333333333333333703, 0.3333333333333333703, 0.3333333333333333703, 0.3333333333333333703, 0.3333333333333333703, 0.3333333333333333703, 0.3333333333333333703, 0.3333333333333333703, 0.3333333333333333703, 0.3333333333333333703, 0.3333333333333333703, 0.3333333333333333703, 0.3333333333333333703, 0.3333333333333333703, 0.3333333333333333703, 0.3333333333333333703, 0.3333333333333333703, 0.3333333333333333703, 0.3333333333333333703, 0.3333333333333333703, 0.3333333333333333703, 0.3333333333333333703, 0.3333333333333333703, 0.3333333333333333703, 0.3333333333333333703, 0.3333333333333333703, 0.3333333333333333703, 0.3333333333333333703, 0.3333333333333333703, 0.3333333333333333703, 0.3333333333333333703, 0.3333333333333333703, 0.3333333333333333703, 0.3333333333333333703, 0.3333333333333333703, 0.3333333333333333703, 0.3333333333333333703, 0.3333333333333333703, 0.3333333333333333703, 0.3333333333333333703, 0.3333333333333333703),
 ( 0.3333333333333333703, 0.3333333333333333703, 0.3333333333333333703, 0.3333333333333333703, 0.3333333333333333703, 0.3333333333333333703, 0.3333333333333333703, 0.3333333333333333703, 0.3333333333333333703, 0.3333333333333333703, 0.3333333333333333703, 0.3333333333333333703, 0.3333333333333333703, 0.3333333333333333703, 0.3333333333333333703, 0.3333333333333333703, 0.3333333333333333703, 0.3333333333333333703, 0.3333333333333333703, 0.3333333333333333703, 0.3333333333333333703, 0.3333333333333333703, 0.3333333333333333703, 0.3333333333333333703, 0.3333333333333333703, 0.3333333333333333703, 0.3333333333333333703, 0.3333333333333333703, 0.3333333333333333703, 0.3333333333333333703, 0.3333333333333333703, 0.3333333333333333703, 0.3333333333333333703, 0.3333333333333333703, 0.3333333333333333703, 0.3333333333333333703, 0.3333333333333333703, 0.3333333333333333703, 0.3333333333333333703, 0.3333333333333333703, 0.3333333333333333703, 0.3333333333333333703, 0.3333333333333333703, 0.3333333333333333703, 0.3333333333333333703, 0.3333333333333333703, 0.3333333333333333703, 0.3333333333333333703, 0.3333333333333333703, 0.3333333333333333703, 0.3333333333333333703, 0.3333333333333333703, 0.3333333333333333703, 0.3333333333333333703, 0.3333333333333333703, 0.3333333333333333703, 0.3333333333333333703, 0.3333333333333333703, 0.3333333333333333703, 0.3333333333333333703, 0.3333333333333333703, 0.3333333333333333703, 0.3333333333333333703, 0.3333333333333333703, 0.3333333333333333703, 0.3333333333333333703, 0.3333333333333333703, 0.3333333333333333703, 0.3333333333333333703, 0.3333333333333333703, 0.3333333333333333703, 0.3333333333333333703, 0.3333333333333333703, 0.3333333333333333703, 0.3333333333333333703, 0.3333333333333333703, 0.3333333333333333703, 0.3333333333333333703, 0.3333333333333333703, 0.3333333333333333703, 0.3333333333333333703, 0.3333333333333333703, 0.3333333333333333703, 0.3333333333333333703, 0.3333333333333333703, 0.3333333333333333703, 0.3333333333333333703, 0.3333333333333333703, 0.3333333333333333703, 0.3333333333333333703, 0.3333333333333333703, 0.3333333333333333703, 0.3333333333333333703, 0.3333333333333333703, 0.3333333333333333703, 0.3333333333333333703, 0.3333333333333333703, 0.3333333333333333703, 0.3333333333333333703, 0.3333333333333333703, 0.3333333333333333703, 0.3333333333333333703, 0.3333333333333333703, 0.3333333333333333703, 0.3333333333333333703, 0.3333333333333333703, 0.3333333333333333703, 0.3333333333333333703, 0.3333333333333333703, 0.3333333333333333703, 0.3333333333333333703, 0.3333333333333333703, 0.3333333333333333703, 0.3333333333333333703, 0.3333333333333333703, 0.3333333333333333703, 0.3333333333333333703, 0.3333333333333333703, 0.3333333333333333703, 0.3333333333333333703, 0.3333333333333333703, 0.3333333333333333703, 0.3333333333333333703, 0.3333333333333333703, 0.3333333333333333703, 0.3333333333333333703, 0.3333333333333333703, 0.3333333333333333703, 0.3333333333333333703, 0.3333333333333333703, 0.3333333333333333703, 0.3333333333333333703, 0.3333333333333333703, 0.3333333333333333703, 0.3333333333333333703, 0.3333333333333333703, 0.3333333333333333703, 0.3333333333333333703, 0.3333333333333333703, 0.3333333333333333703, 0.3333333333333333703, 0.3333333333333333703, 0.3333333333333333703, 0.3333333333333333703, 0.3333333333333333703, 0.3333333333333333703, 0.3333333333333333703, 0.3333333333333333703, 0.3333333333333333703, 0.3333333333333333703, 0.3333333333333333703, 0.3333333333333333703, 0.3333333333333333703, 0.3333333333333333703, 0.3333333333333333703, 0.3333333333333333703, 0.3333333333333333703, 0.3333333333333333703),
 ( 1.000000000000000000, 1.000000000000000000, 1.000000000000000000, 1.000000000000000000, 1.000000000000000000, 1.000000000000000000, 1.000000000000000000, 1.000000000000000000, 1.000000000000000000, 1.000000000000000000, 1.000000000000000000, 1.000000000000000000, 1.000000000000000000, 1.000000000000000000, 1.000000000000000000, 1.000000000000000000, 1.000000000000000000, 1.000000000000000000, 1.000000000000000000, 1.000000000000000000, 1.000000000000000000, 1.000000000000000000, 1.000000000000000000, 1.000000000000000000, 1.000000000000000000, 1.000000000000000000, 1.000000000000000000, 1.000000000000000000, 1.000000000000000000, 1.000000000000000000, 1.000000000000000000, 1.000000000000000000, 1.000000000000000000, 1.000000000000000000, 1.000000000000000000, 1.000000000000000000, 1.000000000000000000, 1.000000000000000000, 1.000000000000000000, 1.000000000000000000, 1.000000000000000000, 1.000000000000000000, 1.000000000000000000, 1.000000000000000000, 1.000000000000000000, 1.000000000000000000, 1.000000000000000000, 1.000000000000000000, 1.000000000000000000, 1.000000000000000000, 1.000000000000000000, 1.000000000000000000, 1.000000000000000000, 1.000000000000000000, 1.000000000000000000, 1.000000000000000000, 1.000000000000000000, 1.000000000000000000, 1.000000000000000000, 1.000000000000000000, 1.000000000000000000, 1.000000000000000000, 1.000000000000000000, 1.000000000000000000, 1.000000000000000000, 1.000000000000000000, 1.000000000000000000, 1.000000000000000000, 1.000000000000000000, 1.000000000000000000, 1.000000000000000000, 1.000000000000000000, 1.000000000000000000, 1.000000000000000000, 1.000000000000000000, 1.000000000000000000, 1.000000000000000000, 1.000000000000000000, 1.000000000000000000, 1.000000000000000000, 1.000000000000000000, 1.000000000000000000, 1.000000000000000000, 1.000000000000000000, 1.000000000000000000, 1.000000000000000000, 1.000000000000000000, 1.000000000000000000, 1.000000000000000000, 1.000000000000000000, 1.000000000000000000, 1.000000000000000000, 1.000000000000000000, 1.000000000000000000, 1.000000000000000000, 1.000000000000000000, 1.000000000000000000, 1.000000000000000000, 1.000000000000000000, 1.000000000000000000, 1.000000000000000000, 1.000000000000000000, 1.000000000000000000, 1.000000000000000000, 1.000000000000000000, 1.000000000000000000, 1.000000000000000000, 1.000000000000000000, 1.000000000000000000, 1.000000000000000000, 1.000000000000000000, 1.000000000000000000, 1.000000000000000000, 1.000000000000000000, 1.000000000000000000, 1.000000000000000000, 1.000000000000000000, 1.000000000000000000, 1.000000000000000000, 1.000000000000000000, 1.000000000000000000, 1.000000000000000000, 1.000000000000000000, 1.000000000000000000, 1.000000000000000000, 1.000000000000000000, 1.000000000000000000, 1.000000000000000000, 1.000000000000000000, 1.000000000000000000, 1.000000000000000000, 1.000000000000000000, 1.000000000000000000, 1.000000000000000000, 1.000000000000000000, 1.000000000000000000, 1.000000000000000000, 1.000000000000000000, 1.000000000000000000, 1.000000000000000000, 1.000000000000000000, 1.000000000000000000, 1.000000000000000000, 1.000000000000000000, 1.000000000000000000, 1.000000000000000000, 1.000000000000000000, 1.000000000000000000, 1.000000000000000000, 1.000000000000000000, 1.000000000000000000, 1.000000000000000000, 1.000000000000000000, 1.000000000000000000, 1.000000000000000000, 1.000000000000000000, 1.000000000000000000, 1.000000000000000000),
 ( 0.3333333333333333703, 0.3333333333333333703, 0.3333333333333333703, 0.3333333333333333703, 0.3333333333333333703, 0.3333333333333333703, 0.3333333333333333703, 0.3333333333333333703, 0.3333333333333333703, 0.3333333333333333703, 0.3333333333333333703, 0.3333333333333333703, 0.3333333333333333703, 0.3333333333333333703, 0.3333333333333333703, 0.3333333333333333703, 0.3333333333333333703, 0.3333333333333333703, 0.3333333333333333703, 0.3333333333333333703, 0.3333333333333333703, 0.3333333333333333703, 0.3333333333333333703, 0.3333333333333333703, 0.3333333333333333703, 0.3333333333333333703, 0.3333333333333333703, 0.3333333333333333703, 0.3333333333333333703, 0.3333333333333333703, 0.3333333333333333703, 0.3333333333333333703, 0.3333333333333333703, 0.3333333333333333703, 0.3333333333333333703, 0.3333333333333333703, 0.3333333333333333703, 0.3333333333333333703, 0.3333333333333333703, 0.3333333333333333703, 0.3333333333333333703, 0.3333333333333333703, 0.3333333333333333703, 0.3333333333333333703, 0.3333333333333333703, 0.3333333333333333703, 0.3333333333333333703, 0.3333333333333333703, 0.3333333333333333703, 0.3333333333333333703, 0.3333333333333333703, 0.3333333333333333703, 0.3333333333333333703, 0.3333333333333333703, 0.3333333333333333703, 0.3333333333333333703, 0.3333333333333333703, 0.3333333333333333703, 0.3333333333333333703, 0.3333333333333333703, 0.3333333333333333703, 0.3333333333333333703, 0.3333333333333333703, 0.3333333333333333703, 0.3333333333333333703, 0.3333333333333333703, 0.3333333333333333703, 0.3333333333333333703, 0.3333333333333333703, 0.3333333333333333703, 0.3333333333333333703, 0.3333333333333333703, 0.3333333333333333703, 0.3333333333333333703, 0.3333333333333333703, 0.3333333333333333703, 0.3333333333333333703, 0.3333333333333333703, 0.3333333333333333703, 0.3333333333333333703, 0.3333333333333333703, 0.3333333333333333703, 0.3333333333333333703, 0.3333333333333333703, 0.3333333333333333703, 0.3333333333333333703, 0.3333333333333333703, 0.3333333333333333703, 0.3333333333333333703, 0.3333333333333333703, 0.3333333333333333703, 0.3333333333333333703, 0.3333333333333333703, 0.3333333333333333703, 0.3333333333333333703, 0.3333333333333333703, 0.3333333333333333703, 0.3333333333333333703, 0.3333333333333333703, 0.3333333333333333703, 0.3333333333333333703, 0.3333333333333333703, 0.3333333333333333703, 0.3333333333333333703, 0.3333333333333333703, 0.3333333333333333703, 0.3333333333333333703, 0.3333333333333333703, 0.3333333333333333703, 0.3333333333333333703, 0.3333333333333333703, 0.3333333333333333703, 0.3333333333333333703, 0.3333333333333333703, 0.3333333333333333703, 0.3333333333333333703, 0.3333333333333333703, 0.3333333333333333703, 0.3333333333333333703, 0.3333333333333333703, 0.3333333333333333703, 0.3333333333333333703, 0.3333333333333333703, 0.3333333333333333703, 0.3333333333333333703, 0.3333333333333333703, 0.3333333333333333703, 0.3333333333333333703, 0.3333333333333333703, 0.3333333333333333703, 0.3333333333333333703, 0.3333333333333333703, 0.3333333333333333703, 0.3333333333333333703, 0.3333333333333333703, 0.3333333333333333703, 0.3333333333333333703, 0.3333333333333333703, 0.3333333333333333703, 0.3333333333333333703, 0.3333333333333333703, 0.3333333333333333703, 0.3333333333333333703, 0.3333333333333333703, 0.3333333333333333703, 0.3333333333333333703, 0.3333333333333333703, 0.3333333333333333703, 0.3333333333333333703, 0.3333333333333333703, 0.3333333333333333703, 0.3333333333333333703, 0.3333333333333333703, 0.3333333333333333703, 0.3333333333333333703, 0.3333333333333333703, 0.3333333333333333703, 0.3333333333333333703),
 ( 0.3333333333333333703, 0.3333333333333333703, 0.3333333333333333703, 0.3333333333333333703, 0.3333333333333333703, 0.3333333333333333703, 0.3333333333333333703, 0.3333333333333333703, 0.3333333333333333703, 0.3333333333333333703, 0.3333333333333333703, 0.3333333333333333703, 0.3333333333333333703, 0.3333333333333333703, 0.3333333333333333703, 0.3333333333333333703, 0.3333333333333333703, 0.3333333333333333703, 0.3333333333333333703, 0.3333333333333333703, 0.3333333333333333703, 0.3333333333333333703, 0.3333333333333333703, 0.3333333333333333703, 0.3333333333333333703, 0.3333333333333333703, 0.3333333333333333703, 0.3333333333333333703, 0.3333333333333333703, 0.3333333333333333703, 0.3333333333333333703, 0.3333333333333333703, 0.3333333333333333703, 0.3333333333333333703, 0.3333333333333333703, 0.3333333333333333703, 0.3333333333333333703, 0.3333333333333333703, 0.3333333333333333703, 0.3333333333333333703, 0.3333333333333333703, 0.3333333333333333703, 0.3333333333333333703, 0.3333333333333333703, 0.3333333333333333703, 0.3333333333333333703, 0.3333333333333333703, 0.3333333333333333703, 0.3333333333333333703, 0.3333333333333333703, 0.3333333333333333703, 0.3333333333333333703, 0.3333333333333333703, 0.3333333333333333703, 0.3333333333333333703, 0.3333333333333333703, 0.3333333333333333703, 0.3333333333333333703, 0.3333333333333333703, 0.3333333333333333703, 0.3333333333333333703, 0.3333333333333333703, 0.3333333333333333703, 0.3333333333333333703, 0.3333333333333333703, 0.3333333333333333703, 0.3333333333333333703, 0.3333333333333333703, 0.3333333333333333703, 0.3333333333333333703, 0.3333333333333333703, 0.3333333333333333703, 0.3333333333333333703, 0.3333333333333333703, 0.3333333333333333703, 0.3333333333333333703, 0.3333333333333333703, 0.3333333333333333703, 0.3333333333333333703, 0.3333333333333333703, 0.3333333333333333703, 0.3333333333333333703, 0.3333333333333333703, 0.3333333333333333703, 0.3333333333333333703, 0.3333333333333333703, 0.3333333333333333703, 0.3333333333333333703, 0.3333333333333333703, 0.3333333333333333703, 0.3333333333333333703, 0.3333333333333333703, 0.3333333333333333703, 0.3333333333333333703, 0.3333333333333333703, 0.3333333333333333703, 0.3333333333333333703, 0.3333333333333333703, 0.3333333333333333703, 0.3333333333333333703, 0.3333333333333333703, 0.3333333333333333703, 0.3333333333333333703, 0.3333333333333333703, 0.3333333333333333703, 0.3333333333333333703, 0.3333333333333333703, 0.3333333333333333703, 0.3333333333333333703, 0.3333333333333333703, 0.3333333333333333703, 0.3333333333333333703, 0.3333333333333333703, 0.3333333333333333703, 0.3333333333333333703, 0.3333333333333333703, 0.3333333333333333703, 0.3333333333333333703, 0.3333333333333333703, 0.3333333333333333703, 0.3333333333333333703, 0.3333333333333333703, 0.3333333333333333703, 0.3333333333333333703, 0.3333333333333333703, 0.3333333333333333703, 0.3333333333333333703, 0.3333333333333333703, 0.3333333333333333703, 0.3333333333333333703, 0.3333333333333333703, 0.3333333333333333703, 0.3333333333333333703, 0.3333333333333333703, 0.3333333333333333703, 0.3333333333333333703, 0.3333333333333333703, 0.3333333333333333703, 0.3333333333333333703, 0.3333333333333333703, 0.3333333333333333703, 0.3333333333333333703, 0.3333333333333333703, 0.3333333333333333703, 0.3333333333333333703, 0.3333333333333333703, 0.3333333333333333703, 0.3333333333333333703, 0.3333333333333333703, 0.3333333333333333703, 0.3333333333333333703, 0.3333333333333333703, 0.3333333333333333703, 0.3333333333333333703, 0.3333333333333333703, 0.3333333333333333703, 0.3333333333333333703, 0.3333333333333333703),
 ( 1.000000000000000000, 1.000000000000000000, 1.000000000000000000, 1.000000000000000000, 1.000000000000000000, 1.000000000000000000, 1.000000000000000000, 1.000000000000000000, 1.000000000000000000, 1.000000000000000000, 1.000000000000000000, 1.000000000000000000, 1.000000000000000000, 1.000000000000000000, 1.000000000000000000, 1.000000000000000000, 1.000000000000000000, 1.000000000000000000, 1.000000000000000000, 1.000000000000000000, 1.000000000000000000, 1.000000000000000000, 1.000000000000000000, 1.000000000000000000, 1.000000000000000000, 1.000000000000000000, 1.000000000000000000, 1.000000000000000000, 1.000000000000000000, 1.000000000000000000, 1.000000000000000000, 1.000000000000000000, 1.000000000000000000, 1.000000000000000000, 1.000000000000000000, 1.000000000000000000, 1.000000000000000000, 1.000000000000000000, 1.000000000000000000, 1.000000000000000000, 1.000000000000000000, 1.000000000000000000, 1.000000000000000000, 1.000000000000000000, 1.000000000000000000, 1.000000000000000000, 1.000000000000000000, 1.000000000000000000, 1.000000000000000000, 1.000000000000000000, 1.000000000000000000, 1.000000000000000000, 1.000000000000000000, 1.000000000000000000, 1.000000000000000000, 1.000000000000000000, 1.000000000000000000, 1.000000000000000000, 1.000000000000000000, 1.000000000000000000, 1.000000000000000000, 1.000000000000000000, 1.000000000000000000, 1.000000000000000000, 1.000000000000000000, 1.000000000000000000, 1.000000000000000000, 1.000000000000000000, 1.000000000000000000, 1.000000000000000000, 1.000000000000000000, 1.000000000000000000, 1.000000000000000000, 1.000000000000000000, 1.000000000000000000, 1.000000000000000000, 1.000000000000000000, 1.000000000000000000, 1.000000000000000000, 1.000000000000000000, 1.000000000000000000, 1.000000000000000000, 1.000000000000000000, 1.000000000000000000, 1.000000000000000000, 1.000000000000000000, 1.000000000000000000, 1.000000000000000000, 1.000000000000000000, 1.000000000000000000, 1.000000000000000000, 1.000000000000000000, 1.000000000000000000, 1.000000000000000000, 1.000000000000000000, 1.000000000000000000, 1.000000000000000000, 1.000000000000000000, 1.000000000000000000, 1.000000000000000000, 1.000000000000000000, 1.000000000000000000, 1.000000000000000000, 1.000000000000000000, 1.000000000000000000, 1.000000000000000000, 1.000000000000000000, 1.000000000000000000, 1.000000000000000000, 1.000000000000000000, 1.000000000000000000, 1.000000000000000000, 1.000000000000000000, 1.000000000000000000, 1.000000000000000000, 1.000000000000000000, 1.000000000000000000, 1.000000000000000000, 1.000000000000000000, 1.000000000000000000, 1.000000000000000000, 1.000000000000000000, 1.000000000000000000, 1.000000000000000000, 1.000000000000000000, 1.000000000000000000, 1.000000000000000000, 1.000000000000000000, 1.000000000000000000, 1.000000000000000000, 1.000000000000000000, 1.000000000000000000, 1.000000000000000000, 1.000000000000000000, 1.000000000000000000, 1.000000000000000000, 1.000000000000000000, 1.000000000000000000, 1.000000000000000000, 1.000000000000000000, 1.000000000000000000, 1.000000000000000000, 1.000000000000000000, 1.000000000000000000, 1.000000000000000000, 1.000000000000000000, 1.000000000000000000, 1.000000000000000000, 1.000000000000000000, 1.000000000000000000, 1.000000000000000000, 1.000000000000000000, 1.000000000000000000, 1.000000000000000000, 1.000000000000000000, 1.000000000000000000, 1.000000000000000000, 1.000000000000000000) ) ) 
 REPRESENTATION_ITEM ( '' )  SURFACE ( )  );
#10307 = DIRECTION ( 'NONE',  ( -1.000000000000000000, 0.000000000000000000, 0.000000000000000000 ) ) ;
#10308 = DIRECTION ( 'NONE',  ( 0.000000000000000000, 0.000000000000000000, 1.000000000000000000 ) ) ;
#10309 = CARTESIAN_POINT ( 'NONE',  ( -37.56526046546249376, -113.9929510916434339, 13.11451721564129258 ) ) ;
#10310 = MANIFOLD_SOLID_BREP ( 'Keyway', #33639 ) ;
#10311 = CARTESIAN_POINT ( 'NONE',  ( -36.62499999999902656, -115.9929510916434481, 13.11852480586264846 ) ) ;
#10312 = DIRECTION ( 'NONE',  ( -1.000000000000000000, 0.000000000000000000, 0.000000000000000000 ) ) ;
#10313 = DIRECTION ( 'NONE',  ( -0.000000000000000000, 0.000000000000000000, -1.000000000000000000 ) ) ;
#10314 = ORIENTED_EDGE ( 'NONE', *, *, #24298, .F. ) ;
#10315 = CARTESIAN_POINT ( 'NONE',  ( 0.000000000000000000, 0.000000000000000000, 0.000000000000000000 ) ) ;
#10316 = DIRECTION ( 'NONE',  ( -1.000000000000000000, -1.836970198721029934E-16, -0.000000000000000000 ) ) ;
#10317 = CARTESIAN_POINT ( 'NONE',  ( -3.799999999999999822, 0.000000000000000000, -39.50000000000000711 ) ) ;
#10318 = ORIENTED_EDGE ( 'NONE', *, *, #13006, .F. ) ;
#10319 = CARTESIAN_POINT ( 'NONE',  ( 0.000000000000000000, -39.78933988720132220, 24.98727647984988565 ) ) ;
#10320 = EDGE_CURVE ( 'NONE', #18391, #4328, #21531, .T. ) ;
#10321 = CARTESIAN_POINT ( 'NONE',  ( -35.50000000000000711, -112.7549084230351752, -1.592823285203595285 ) ) ;
#10322 = CARTESIAN_POINT ( 'NONE',  ( 0.000000000000000000, -2.710505431213761085E-17, 45.10000000000000142 ) ) ;
#10323 = EDGE_CURVE ( 'NONE', #30561, #2044, #30486, .T. ) ;
#10324 = CIRCLE ( 'NONE', #32729, 20.00000000000000711 ) ;
#10325 = DIRECTION ( 'NONE',  ( -1.000000000000000000, 0.000000000000000000, 0.000000000000000000 ) ) ;
#10326 = CARTESIAN_POINT ( 'NONE',  ( 0.000000000000000000, 0.000000000000000000, -44.50000000000000000 ) ) ;
#10327 = ORIENTED_EDGE ( 'NONE', *, *, #19377, .T. ) ;
#10328 = AXIS2_PLACEMENT_3D ( 'NONE', #6881, #10113, #12464 ) ;
#10329 = DIRECTION ( 'NONE',  ( 0.000000000000000000, 0.000000000000000000, -1.000000000000000000 ) ) ;
#10330 = CARTESIAN_POINT ( 'NONE',  ( -35.50000000000000000, -113.6807644833805995, -2.624782352598442614 ) ) ;
#10331 = ORIENTED_EDGE ( 'NONE', *, *, #2711, .F. ) ;
#10332 = EDGE_LOOP ( 'NONE', ( #20354, #3125, #15214, #22173 ) ) ;
#10333 = CARTESIAN_POINT ( 'NONE',  ( -37.47347596530441649, -114.9754527089670262, 7.972274454178450043 ) ) ;
#10334 = ADVANCED_FACE ( 'NONE', ( #2848 ), #5365, .T. ) ;
#10335 = AXIS2_PLACEMENT_3D ( 'NONE', #8658, #19625, #6316 ) ;
#10336 = SHAPE_REPRESENTATION_RELATIONSHIP ( 'NONE' , 'NONE' ,  #8186, #16793 ) ;
#10337 = CARTESIAN_POINT ( 'NONE',  ( 0.000000000000000000, 0.000000000000000000, 0.000000000000000000 ) ) ;
#10338 = ORIENTED_EDGE ( 'NONE', *, *, #18882, .T. ) ;
#10339 = VERTEX_POINT ( 'NONE', #33252 ) ;
#10340 = CARTESIAN_POINT ( 'NONE',  ( -34.50000000000000000, -113.8474311500459777, -0.6247823525984269599 ) ) ;
#10341 = DIRECTION ( 'NONE',  ( 1.000000000000000000, 0.000000000000000000, 0.000000000000000000 ) ) ;
#10342 = DIRECTION ( 'NONE',  ( -1.047965281155519790E-16, -6.938893903907192632E-17, -1.000000000000000000 ) ) ;
#10343 = APPLICATION_CONTEXT ( 'automotive_design' ) ;
#10344 = CARTESIAN_POINT ( 'NONE',  ( -38.00000000000000711, -114.9929510916434339, 12.44250253426874941 ) ) ;
#10345 = CARTESIAN_POINT ( 'NONE',  ( 0.000000000000000000, 0.000000000000000000, 0.000000000000000000 ) ) ;
#10346 = VECTOR ( 'NONE', #25133, 1000.000000000000000 ) ;
#10347 = DIRECTION ( 'NONE',  ( 0.000000000000000000, 0.000000000000000000, 1.000000000000000000 ) ) ;
#10348 = CARTESIAN_POINT ( 'NONE',  ( -34.50000000000000000, -112.0414288467712112, 1.115164475686276191 ) ) ;
#10349 = ADVANCED_FACE ( 'NONE', ( #32898 ), #13460, .T. ) ;
#10350 = CYLINDRICAL_SURFACE ( 'NONE', #31838, 8.000000000000001776 ) ;
#10351 = AXIS2_PLACEMENT_3D ( 'NONE', #3219, #14181, #19568 ) ;
#10352 = CARTESIAN_POINT ( 'NONE',  ( 8.000000000000000000, 0.3212489022565391261, 16.91141623315867193 ) ) ;
#10353 = ORIENTED_EDGE ( 'NONE', *, *, #21387, .F. ) ;
#10354 = COLOUR_RGB ( '', 0.66274510, 0.83137255, 0.94901961) ;
#10355 = PRODUCT_DEFINITION_FORMATION_WITH_SPECIFIED_SOURCE ( 'ANY', '', #9806, .NOT_KNOWN. ) ;
#10356 = CARTESIAN_POINT ( 'NONE',  ( -36.06250000000000711, -115.9929510916434481, 13.11852480586264846 ) ) ;
#10357 = DIRECTION ( 'NONE',  ( 0.000000000000000000, 0.9848077530122095746, -0.1736481776669212829 ) ) ;
#10358 = CARTESIAN_POINT ( 'NONE',  ( 0.000000000000000000, -32.32520163883607722, 34.09746168776025854 ) ) ;
#10359 = DIRECTION ( 'NONE',  ( -1.000000000000000000, 0.000000000000000000, 0.000000000000000000 ) ) ;
#10360 = CARTESIAN_POINT ( 'NONE',  ( -42.49999999999999289, -26.68172400785650922, 80.78589838486213637 ) ) ;
#10361 = ORIENTED_EDGE ( 'NONE', *, *, #25562, .F. ) ;
#10362 = DIRECTION ( 'NONE',  ( -1.000000000000000000, 0.000000000000000000, 0.000000000000000000 ) ) ;
#10363 = CARTESIAN_POINT ( 'NONE',  ( 0.000000000000000000, 0.000000000000000000, 0.000000000000000000 ) ) ;
#10364 = EDGE_CURVE ( 'NONE', #31652, #34767, #17214, .T. ) ;
#10365 = CARTESIAN_POINT ( 'NONE',  ( 8.000000000000000000, 0.000000000000000000, 0.000000000000000000 ) ) ;
#10366 = DIRECTION ( 'NONE',  ( 1.110223024625156540E-16, 1.000000000000000000, 0.000000000000000000 ) ) ;
#10367 = ADVANCED_FACE ( 'NONE', ( #13632 ), #30382, .T. ) ;
#10368 = ADVANCED_FACE ( 'NONE', ( #27509 ), #3020, .T. ) ;
#10369 = CARTESIAN_POINT ( 'NONE',  ( 0.000000000000000000, 19.77827456857338007, 2.969824084036534639 ) ) ;
#10370 = MANIFOLD_SOLID_BREP ( 'Keyway', #4341 ) ;
#10371 = CARTESIAN_POINT ( 'NONE',  ( 8.000000000000000000, 0.000000000000000000, 0.000000000000000000 ) ) ;
#10372 = ORIENTED_EDGE ( 'NONE', *, *, #28849, .T. ) ;
#10373 = ORIENTED_EDGE ( 'NONE', *, *, #18675, .F. ) ;
#10374 = DIRECTION ( 'NONE',  ( 0.000000000000000000, 0.000000000000000000, 1.000000000000000000 ) ) ;
#10375 = DIRECTION ( 'NONE',  ( -1.000000000000000000, 0.000000000000000000, 0.000000000000000000 ) ) ;
#10376 = FACE_OUTER_BOUND ( 'NONE', #12226, .T. ) ;
#10377 = VERTEX_POINT ( 'NONE', #9111 ) ;
#10378 = VECTOR ( 'NONE', #24564, 1000.000000000000000 ) ;
#10379 = CARTESIAN_POINT ( 'NONE',  ( -36.11231047232249125, -115.9754527089670262, 4.277725545821551734 ) ) ;
#10380 = ADVANCED_FACE ( 'NONE', ( #17372 ), #13979, .F. ) ;
#10381 = ORIENTED_EDGE ( 'NONE', *, *, #2910, .T. ) ;
#10382 = ADVANCED_FACE ( 'NONE', ( #33960, #34137 ), #17018, .T. ) ;
#10383 = ORIENTED_EDGE ( 'NONE', *, *, #10194, .F. ) ;
#10384 = VERTEX_POINT ( 'NONE', #15031 ) ;
#10385 = ADVANCED_BREP_SHAPE_REPRESENTATION ( '', ( #33750, #21307 ), #23057 ) ;
#10386 = CARTESIAN_POINT ( 'NONE',  ( -34.49999999999998579, -21.76666049839542794, 84.29903810567665801 ) ) ;
#10387 = AXIS2_PLACEMENT_3D ( 'NONE', #24585, #21685, #13592 ) ;
#10388 = AXIS2_PLACEMENT_3D ( 'NONE', #15836, #29730, #26855 ) ;
#10389 = DIRECTION ( 'NONE',  ( 0.000000000000000000, 0.000000000000000000, 1.000000000000000000 ) ) ;
#10390 = ORIENTED_EDGE ( 'NONE', *, *, #7880, .F. ) ;
#10391 = ORIENTED_EDGE ( 'NONE', *, *, #30160, .T. ) ;
#10392 = DIRECTION ( 'NONE',  ( 0.000000000000000000, -0.1253332335643113082, 0.9921147013144768767 ) ) ;
#10393 = CARTESIAN_POINT ( 'NONE',  ( -35.00000000000000000, -113.9407375970687895, 2.496475545821554398 ) ) ;
#10394 = CARTESIAN_POINT ( 'NONE',  ( -1.599999999999990319, 0.000000000000000000, 0.000000000000000000 ) ) ;
#10395 = ADVANCED_FACE ( 'NONE', ( #20068 ), #25685, .T. ) ;
#10396 = CARTESIAN_POINT ( 'NONE',  ( -9.999999999999994671, 0.000000000000000000, 0.000000000000000000 ) ) ;
#10397 = CYLINDRICAL_SURFACE ( 'NONE', #26621, 8.000000000000001776 ) ;
#10398 = ADVANCED_FACE ( 'NONE', ( #3718 ), #22961, .T. ) ;
#10399 = AXIS2_PLACEMENT_3D ( 'NONE', #674, #28065, #31282 ) ;
#10400 = CARTESIAN_POINT ( 'NONE',  ( 0.000000000000000000, 0.000000000000000000, 0.000000000000000000 ) ) ;
#10401 = CARTESIAN_POINT ( 'NONE',  ( -35.54388159064475872, -112.6276912846090568, 4.316024454178448266 ) ) ;
#10402 = ADVANCED_FACE ( 'NONE', ( #28557 ), #14321, .T. ) ;
#10403 = CARTESIAN_POINT ( 'NONE',  ( -34.51202277066418844, -115.9929510916434481, 12.81430620224972294 ) ) ;
#10404 = CARTESIAN_POINT ( 'NONE',  ( 0.000000000000000000, 0.000000000000000000, 4.000000000000000000 ) ) ;
#10405 = DIRECTION ( 'NONE',  ( -1.000000000000000000, 0.000000000000000000, 0.000000000000000000 ) ) ;
#10406 = CARTESIAN_POINT ( 'NONE',  ( 7.999999999999992895, -46.19362259308839214, 8.585149169758333088 ) ) ;
#10407 = CARTESIAN_POINT ( 'NONE',  ( 1.599999999999989875, -5.408326913195883989, -0.7999999999999958256 ) ) ;
#10408 = DIRECTION ( 'NONE',  ( -1.000000000000000000, 0.000000000000000000, 0.000000000000000000 ) ) ;
#10409 = DIRECTION ( 'NONE',  ( -1.000000000000000000, -0.000000000000000000, -0.000000000000000000 ) ) ;
#10410 = ORIENTED_EDGE ( 'NONE', *, *, #20014, .F. ) ;
#10411 = EDGE_CURVE ( 'NONE', #4187, #21532, #11996, .T. ) ;
#10412 = ADVANCED_FACE ( 'NONE', ( #6403 ), #25883, .T. ) ;
#10413 = AXIS2_PLACEMENT_3D ( 'NONE', #12847, #31741, #7074 ) ;
#10414 = CARTESIAN_POINT ( 'NONE',  ( -38.97545270896704039, -114.8876895276775087, 6.152725545821551734 ) ) ;
#10415 = AXIS2_PLACEMENT_3D ( 'NONE', #2560, #7751, #4900 ) ;
#10416 = DIRECTION ( 'NONE',  ( 0.000000000000000000, -1.000000000000000000, 0.000000000000000000 ) ) ;
#10417 = DIRECTION ( 'NONE',  ( -1.000000000000000000, 0.000000000000000000, 0.000000000000000000 ) ) ;
#10418 = AXIS2_PLACEMENT_3D ( 'NONE', #15979, #1793, #24289 ) ;
#10419 = ORIENTED_EDGE ( 'NONE', *, *, #886, .F. ) ;
#10420 = ORIENTED_EDGE ( 'NONE', *, *, #24504, .T. ) ;
#10421 = CARTESIAN_POINT ( 'NONE',  ( -30.00000000000000000, 2.571758278209441661E-15, 0.000000000000000000 ) ) ;
#10422 = CARTESIAN_POINT ( 'NONE',  ( -46.00000000000000000, -25.98076211353320275, 95.99999999999991473 ) ) ;
#10423 = ORIENTED_EDGE ( 'NONE', *, *, #2477, .F. ) ;
#10424 = VERTEX_POINT ( 'NONE', #31432 ) ;
#10425 = EDGE_CURVE ( 'NONE', #26694, #5490, #11622, .T. ) ;
#10426 = DIRECTION ( 'NONE',  ( -1.174092375852890260E-15, 4.222049128630259891E-16, 1.000000000000000000 ) ) ;
#10427 = DIRECTION ( 'NONE',  ( -1.000000000000000000, 0.000000000000000000, 0.000000000000000000 ) ) ;
#10428 = DIRECTION ( 'NONE',  ( 0.000000000000000000, 0.000000000000000000, 1.000000000000000000 ) ) ;
#10429 = CARTESIAN_POINT ( 'NONE',  ( -26.99999999999999645, 20.00000000000000000, 2.449293598294706119E-15 ) ) ;
#10430 = EDGE_LOOP ( 'NONE', ( #2738, #25566 ) ) ;
#10431 = EDGE_LOOP ( 'NONE', ( #28570, #31808, #12123, #28379 ) ) ;
#10432 = CARTESIAN_POINT ( 'NONE',  ( -35.50000000000000711, -112.6605569508015350, 1.812590711673265575 ) ) ;
#10433 = DIRECTION ( 'NONE',  ( 0.000000000000000000, 0.000000000000000000, 1.000000000000000000 ) ) ;
#10434 = CIRCLE ( 'NONE', #31700, 7.199999999999994849 ) ;
#10435 = STYLED_ITEM ( 'NONE', ( #9793 ), #10385 ) ;
#10436 = ORIENTED_EDGE ( 'NONE', *, *, #33892, .F. ) ;
#10437 = CARTESIAN_POINT ( 'NONE',  ( -46.00000000000000000, 1.347111479062090180E-15, 59.00000000000000000 ) ) ;
#10438 = ADVANCED_FACE ( 'NONE', ( #31253 ), #6576, .T. ) ;
#10439 = CARTESIAN_POINT ( 'NONE',  ( -34.50000000000000000, -112.0141053790792114, 0.9054673897245171243 ) ) ;
#10440 = EDGE_CURVE ( 'NONE', #24590, #24598, #4612, .T. ) ;
#10441 = CARTESIAN_POINT ( 'NONE',  ( -34.50000000000000000, -114.9929510916434339, 10.51725893871048889 ) ) ;
#10442 = DIRECTION ( 'NONE',  ( 1.000000000000000000, -0.000000000000000000, -0.000000000000000000 ) ) ;
#10443 = CARTESIAN_POINT ( 'NONE',  ( -37.99974912065192711, -114.9929510916434339, 12.63488142334838571 ) ) ;
#10444 = DIRECTION ( 'NONE',  ( 0.000000000000000000, 0.000000000000000000, -1.000000000000000000 ) ) ;
#10445 = CARTESIAN_POINT ( 'NONE',  ( -34.50000000000000000, -114.9922651054798308, 10.46846006712531008 ) ) ;
#10446 = LINE ( 'NONE', #21406, #27969 ) ;
#10447 = CARTESIAN_POINT ( 'NONE',  ( 8.000000000000000000, 6.336799421339808447, 16.31134495048485533 ) ) ;
#10448 = DIRECTION ( 'NONE',  ( -1.000000000000000000, 0.000000000000000000, 0.000000000000000000 ) ) ;
#10449 = EDGE_LOOP ( 'NONE', ( #27959, #3430, #12857, #13771, #15049, #30958, #23148, #4080, #25336, #3079, #28708, #9870, #1252, #21396, #18668, #3417, #14645, #5600, #27257, #21470, #3971, #7000, #14575, #19709, #33429, #4938, #9513, #4234, #26086, #13877, #32730, #12938, #23941, #12001, #12546, #17746, #15116, #2788, #34508, #27253, #14218, #24494, #10559, #6511, #30430, #12408, #18053, #27441 ) ) ;
#10450 = DIRECTION ( 'NONE',  ( 0.000000000000000000, 0.000000000000000000, 1.000000000000000000 ) ) ;
#10451 = LINE ( 'NONE', #27195, #8864 ) ;
#10452 = ORIENTED_EDGE ( 'NONE', *, *, #14711, .F. ) ;
#10453 = CARTESIAN_POINT ( 'NONE',  ( -38.00000000000000711, -114.9929510916434339, 12.59652202191340820 ) ) ;
#10454 = ORIENTED_EDGE ( 'NONE', *, *, #30788, .F. ) ;
#10455 = EDGE_CURVE ( 'NONE', #32273, #18735, #8033, .T. ) ;
#10456 = CARTESIAN_POINT ( 'NONE',  ( -35.54388159064475872, -112.6276912846090568, 8.816024454178448266 ) ) ;
#10457 = EDGE_CURVE ( 'NONE', #5216, #25950, #1194, .T. ) ;
#10458 = CARTESIAN_POINT ( 'NONE',  ( 8.000000000000007105, -8.725776631572701447, 3.753907720749016796 ) ) ;
#10459 = EDGE_LOOP ( 'NONE', ( #9393, #4810, #28846, #19473 ) ) ;
#10460 = ORIENTED_EDGE ( 'NONE', *, *, #7323, .F. ) ;
#10461 = CARTESIAN_POINT ( 'NONE',  ( -4.000000000000000000, 0.000000000000000000, 65.00000000000000000 ) ) ;
#10462 = CIRCLE ( 'NONE', #97, 4.980000000000017302 ) ;
#10463 = COLOUR_RGB ( '', 0.66274510, 0.83137255, 0.94901961) ;
#10464 = ORIENTED_EDGE ( 'NONE', *, *, #6771, .T. ) ;
#10465 = CARTESIAN_POINT ( 'NONE',  ( -39.07941549657748936, -111.8367748094582055, 2.441024454178448710 ) ) ;
#10466 = DIRECTION ( 'NONE',  ( 0.000000000000000000, 0.6845471059286900584, -0.7289686274214103312 ) ) ;
#10467 = DIRECTION ( 'NONE',  ( -0.000000000000000000, 0.000000000000000000, -1.000000000000000000 ) ) ;
#10468 = ORIENTED_EDGE ( 'NONE', *, *, #17976, .F. ) ;
#10469 = ORIENTED_EDGE ( 'NONE', *, *, #18244, .T. ) ;
#10470 = FACE_OUTER_BOUND ( 'NONE', #8407, .T. ) ;
#10471 = DIRECTION ( 'NONE',  ( 0.000000000000000000, 0.000000000000000000, -1.000000000000000000 ) ) ;
#10472 = ORIENTED_EDGE ( 'NONE', *, *, #32076, .F. ) ;
#10473 = VERTEX_POINT ( 'NONE', #20418 ) ;
#10474 = CARTESIAN_POINT ( 'NONE',  ( -34.50000000000000000, -111.0360125565790383, 1.176611260687384419 ) ) ;
#10475 = DIRECTION ( 'NONE',  ( -1.000000000000000000, 0.000000000000000000, -0.000000000000000000 ) ) ;
#10476 = ORIENTED_EDGE ( 'NONE', *, *, #15650, .F. ) ;
#10477 = CARTESIAN_POINT ( 'NONE',  ( -35.50000000000000711, -114.1152303497977414, 9.513755561829650986 ) ) ;
#10478 = EDGE_CURVE ( 'NONE', #18497, #11997, #6900, .T. ) ;
#10479 = CARTESIAN_POINT ( 'NONE',  ( -34.50000000000000000, -113.9929510916434339, 10.50625754673588474 ) ) ;
#10480 = CARTESIAN_POINT ( 'NONE',  ( 8.000000000000000000, 14.48509162075973755, -8.733917826871222090 ) ) ;
#10481 = DIRECTION ( 'NONE',  ( -0.000000000000000000, 0.000000000000000000, -1.000000000000000000 ) ) ;
#10482 = VECTOR ( 'NONE', #10212, 1000.000000000000000 ) ;
#10483 = CARTESIAN_POINT ( 'NONE',  ( -37.51635661748575501, -113.9929510916434339, 13.11827392651459512 ) ) ;
#10484 = CARTESIAN_POINT ( 'NONE',  ( -37.99839555572501837, -115.9929510916434481, 12.65937477241749143 ) ) ;
#10485 = LINE ( 'NONE', #18400, #31413 ) ;
#10486 = CARTESIAN_POINT ( 'NONE',  ( 54.99999999999999289, -64.99999999999997158, 120.0000000000000000 ) ) ;
#10487 = ORIENTED_EDGE ( 'NONE', *, *, #15461, .T. ) ;
#10488 = LINE ( 'NONE', #8299, #33803 ) ;
#10489 = CARTESIAN_POINT ( 'NONE',  ( 0.000000000000000000, 11.19999565274250308, 10.71350075272077973 ) ) ;
#10490 = CARTESIAN_POINT ( 'NONE',  ( 0.000000000000000000, -5.871425383721172508, -51.66745943012291065 ) ) ;
#10491 = ORIENTED_EDGE ( 'NONE', *, *, #25778, .F. ) ;
#10492 = VECTOR ( 'NONE', #8529, 1000.000000000000000 ) ;
#10493 = DIRECTION ( 'NONE',  ( 1.000000000000000000, 0.000000000000000000, 0.000000000000000000 ) ) ;
#10494 = CARTESIAN_POINT ( 'NONE',  ( -35.50000000000000711, -115.5178116849130276, -1.498529437126731034 ) ) ;
#10495 = CARTESIAN_POINT ( 'NONE',  ( -39.49999999999999289, 9.432411113711806294, 117.4309090467819772 ) ) ;
#10496 = CARTESIAN_POINT ( 'NONE',  ( -35.50000000000000711, -114.9929510916434339, 11.73841344789270202 ) ) ;
#10497 = CARTESIAN_POINT ( 'NONE',  ( -3.983177536951265640, -13.66651769228263724, -1.200000000000006617 ) ) ;
#10498 = ORIENTED_EDGE ( 'NONE', *, *, #7460, .T. ) ;
#10499 = CARTESIAN_POINT ( 'NONE',  ( -23.00000000000000355, 3.857637417314161900E-15, 0.000000000000000000 ) ) ;
#10500 = CARTESIAN_POINT ( 'NONE',  ( -35.50000000000000000, -111.0140978167138570, 0.3752176474015639918 ) ) ;
#10501 = VECTOR ( 'NONE', #23259, 1000.000000000000000 ) ;
#10502 = ORIENTED_EDGE ( 'NONE', *, *, #30655, .F. ) ;
#10503 = ORIENTED_EDGE ( 'NONE', *, *, #16074, .F. ) ;
#10504 = CARTESIAN_POINT ( 'NONE',  ( -37.66520193420439000, -113.2509883718312977, 8.441024454178448266 ) ) ;
#10505 = VECTOR ( 'NONE', #16102, 1000.000000000000000 ) ;
#10506 = AXIS2_PLACEMENT_3D ( 'NONE', #6472, #25400, #25576 ) ;
#10507 = DIRECTION ( 'NONE',  ( -1.000000000000000000, 0.000000000000000000, 0.000000000000000000 ) ) ;
#10508 = ORIENTED_EDGE ( 'NONE', *, *, #1138, .T. ) ;
#10509 = ORIENTED_EDGE ( 'NONE', *, *, #27735, .F. ) ;
#10510 = CARTESIAN_POINT ( 'NONE',  ( -34.50000000000000000, -114.9307644833806137, -0.6247823525984269599 ) ) ;
#10511 = LINE ( 'NONE', #18966, #20034 ) ;
#10512 = CARTESIAN_POINT ( 'NONE',  ( 0.000000000000000000, 46.21320724403649649, 10.97699764141971102 ) ) ;
#10513 = CIRCLE ( 'NONE', #32926, 22.00000000000000000 ) ;
#10514 = AXIS2_PLACEMENT_3D ( 'NONE', #26024, #17900, #18439 ) ;
#10515 = EDGE_CURVE ( 'NONE', #15970, #3935, #11502, .T. ) ;
#10516 = CARTESIAN_POINT ( 'NONE',  ( -37.24999999999992895, -114.9929510916434339, 13.11852480586264669 ) ) ;
#10517 = DIRECTION ( 'NONE',  ( 0.000000000000000000, -6.938893903907203726E-17, -1.000000000000000000 ) ) ;
#10518 = DIRECTION ( 'NONE',  ( -1.000000000000000000, 0.000000000000000000, 0.000000000000000000 ) ) ;
#10519 = CARTESIAN_POINT ( 'NONE',  ( -34.50000000000000000, -112.0140978167138712, 0.0002176474015661141945 ) ) ;
#10520 = CARTESIAN_POINT ( 'NONE',  ( 8.000000000000000000, 0.000000000000000000, 0.000000000000000000 ) ) ;
#10521 = CIRCLE ( 'NONE', #11666, 7.499999999999992895 ) ;
#10522 = VECTOR ( 'NONE', #549, 1000.000000000000000 ) ;
#10523 = LINE ( 'NONE', #15911, #31263 ) ;
#10524 = EDGE_LOOP ( 'NONE', ( #18600, #28082, #28258, #30946 ) ) ;
#10525 = EDGE_CURVE ( 'NONE', #5751, #2191, #14491, .T. ) ;
#10526 = CIRCLE ( 'NONE', #15102, 20.00000000000000711 ) ;
#10527 = CARTESIAN_POINT ( 'NONE',  ( -35.50000000000000711, -114.0371586325023117, 9.504435485030890973 ) ) ;
#10528 = DIRECTION ( 'NONE',  ( -1.000000000000000000, -0.000000000000000000, 0.000000000000000000 ) ) ;
#10529 = LINE ( 'NONE', #21318, #17949 ) ;
#10530 = CARTESIAN_POINT ( 'NONE',  ( 3.799999999999999822, 0.000000000000000000, -52.50000000000000000 ) ) ;
#10531 = DIRECTION ( 'NONE',  ( -1.000000000000000000, 0.000000000000000000, 0.000000000000000000 ) ) ;
#10532 = EDGE_LOOP ( 'NONE', ( #29913, #6332, #7051, #29253 ) ) ;
#10533 = DIRECTION ( 'NONE',  ( 0.02040816326530624572, 0.9997917317482359900, -1.513872302914096262E-31 ) ) ;
#10534 = CARTESIAN_POINT ( 'NONE',  ( 0.000000000000000000, -2.710505431213761085E-17, 55.00000000000000000 ) ) ;
#10535 = CARTESIAN_POINT ( 'NONE',  ( 8.000000000000000000, -11.19999565274241782, -10.71350075272084545 ) ) ;
#10536 = CARTESIAN_POINT ( 'NONE',  ( 70.00000000000001421, 58.94749845961094792, 75.40996905927893579 ) ) ;
#10537 = CARTESIAN_POINT ( 'NONE',  ( 4.000000000000003553, 35.11945359308111847, 38.34871548466026070 ) ) ;
#10538 = DIRECTION ( 'NONE',  ( 0.000000000000000000, 0.000000000000000000, -1.000000000000000000 ) ) ;
#10539 = VERTEX_POINT ( 'NONE', #11802 ) ;
#10540 = AXIS2_PLACEMENT_3D ( 'NONE', #676, #8774, #19741 ) ;
#10541 = EDGE_LOOP ( 'NONE', ( #28505, #11020, #21032, #10854 ) ) ;
#10542 = AXIS2_PLACEMENT_3D ( 'NONE', #21668, #26742, #22028 ) ;
#10543 = CARTESIAN_POINT ( 'NONE',  ( 4.000000000000003553, -19.83898331853678343, -9.508666619816859011 ) ) ;
#10544 = AXIS2_PLACEMENT_3D ( 'NONE', #11503, #28021, #12160 ) ;
#10545 = CARTESIAN_POINT ( 'NONE',  ( 7.999999999999992895, 0.000000000000000000, 0.000000000000000000 ) ) ;
#10546 = CARTESIAN_POINT ( 'NONE',  ( 8.000000000000000000, 0.000000000000000000, -1.000000000000000222 ) ) ;
#10547 = ORIENTED_EDGE ( 'NONE', *, *, #33723, .F. ) ;
#10548 = CARTESIAN_POINT ( 'NONE',  ( -38.45611840935523418, -112.6276912846090568, 7.933975545821552622 ) ) ;
#10549 = EDGE_LOOP ( 'NONE', ( #1973, #13835, #20372, #16403 ) ) ;
#10550 = EDGE_CURVE ( 'NONE', #29785, #28091, #29920, .T. ) ;
#10551 = VERTEX_POINT ( 'NONE', #24060 ) ;
#10552 = VERTEX_POINT ( 'NONE', #12528 ) ;
#10553 = CARTESIAN_POINT ( 'NONE',  ( 0.000000000000000000, 0.000000000000000000, 55.00000000000000711 ) ) ;
#10554 = APPLICATION_CONTEXT ( 'automotive_design' ) ;
#10555 = VECTOR ( 'NONE', #30108, 1000.000000000000000 ) ;
#10556 = AXIS2_PLACEMENT_3D ( 'NONE', #34532, #3944, #25722 ) ;
#10557 = CARTESIAN_POINT ( 'NONE',  ( -21.15833593587365513, -24.48076211353326315, 88.99999999999994316 ) ) ;
#10558 = EDGE_LOOP ( 'NONE', ( #19768, #31078 ) ) ;
#10559 = ORIENTED_EDGE ( 'NONE', *, *, #6380, .T. ) ;
#10560 = ADVANCED_FACE ( 'NONE', ( #4623 ), #15380, .T. ) ;
#10561 = FACE_OUTER_BOUND ( 'NONE', #29186, .T. ) ;
#10562 = CARTESIAN_POINT ( 'NONE',  ( -44.00000000000000000, -3.999999999999998224, 0.000000000000000000 ) ) ;
#10563 = EDGE_CURVE ( 'NONE', #19637, #32720, #32763, .T. ) ;
#10564 = EDGE_CURVE ( 'NONE', #8141, #7811, #34677, .T. ) ;
#10565 = LINE ( 'NONE', #34890, #7894 ) ;
#10566 = AXIS2_PLACEMENT_3D ( 'NONE', #20103, #31110, #6438 ) ;
#10567 = DIRECTION ( 'NONE',  ( -0.000000000000000000, 0.000000000000000000, -1.000000000000000000 ) ) ;
#10568 = DIRECTION ( 'NONE',  ( 0.000000000000000000, 0.000000000000000000, 1.000000000000000000 ) ) ;
#10569 = CARTESIAN_POINT ( 'NONE',  ( -38.37230871539094323, -112.5438815906447729, 3.941024454178448710 ) ) ;
#10570 = EDGE_CURVE ( 'NONE', #9078, #26450, #34859, .T. ) ;
#10571 = CARTESIAN_POINT ( 'NONE',  ( -35.51674767832922441, -115.9929510916434481, 14.04194344061634325 ) ) ;
#10572 = CARTESIAN_POINT ( 'NONE',  ( 0.000000000000000000, 18.48663108841359559, 4.615718728112120139 ) ) ;
#10573 = EDGE_CURVE ( 'NONE', #21964, #19855, #23006, .T. ) ;
#10574 = FACE_OUTER_BOUND ( 'NONE', #23047, .T. ) ;
#10575 = DIRECTION ( 'NONE',  ( 0.000000000000000000, 0.000000000000000000, -1.000000000000000000 ) ) ;
#10576 = FACE_OUTER_BOUND ( 'NONE', #12540, .T. ) ;
#10577 = VECTOR ( 'NONE', #15829, 1000.000000000000000 ) ;
#10578 = AXIS2_PLACEMENT_3D ( 'NONE', #10352, #18620, #18076 ) ;
#10579 = CARTESIAN_POINT ( 'NONE',  ( 7.999999999999992895, -45.78515115856034612, -12.64416602183715455 ) ) ;
#10580 = LINE ( 'NONE', #12928, #18928 ) ;
#10581 = ORIENTED_EDGE ( 'NONE', *, *, #34263, .F. ) ;
#10582 = CARTESIAN_POINT ( 'NONE',  ( -37.05926240293131713, -111.0000000000000284, 8.121475545821549957 ) ) ;
#10583 = FACE_OUTER_BOUND ( 'NONE', #3738, .T. ) ;
#10584 = DIRECTION ( 'NONE',  ( 0.000000000000000000, 0.000000000000000000, -1.000000000000000000 ) ) ;
#10585 = CARTESIAN_POINT ( 'NONE',  ( 7.999999999999992895, -17.50309955389579386, -43.60271849949381817 ) ) ;
#10586 = ORIENTED_EDGE ( 'NONE', *, *, #12569, .T. ) ;
#10587 = ORIENTED_EDGE ( 'NONE', *, *, #22212, .F. ) ;
#10588 = CIRCLE ( 'NONE', #21484, 20.00000000000000711 ) ;
#10589 = FILL_AREA_STYLE_COLOUR ( '', #2799 ) ;
#10590 = CARTESIAN_POINT ( 'NONE',  ( 8.000000000000007105, 1.111908866155100650, 9.433698091065117808 ) ) ;
#10591 = ORIENTED_EDGE ( 'NONE', *, *, #21601, .F. ) ;
#10592 = ORIENTED_EDGE ( 'NONE', *, *, #22499, .F. ) ;
#10593 = EDGE_CURVE ( 'NONE', #29687, #15571, #12889, .T. ) ;
#10594 = DIRECTION ( 'NONE',  ( -1.000000000000000000, 0.000000000000000000, -0.000000000000000000 ) ) ;
#10595 = EDGE_CURVE ( 'NONE', #26801, #32964, #13253, .T. ) ;
#10596 = LINE ( 'NONE', #4510, #32095 ) ;
#10597 = DIRECTION ( 'NONE',  ( -1.000000000000000000, -7.849623728795052102E-17, 8.326672684688674053E-17 ) ) ;
#10598 = CARTESIAN_POINT ( 'NONE',  ( -44.00000000000000000, 0.000000000000000000, 0.000000000000000000 ) ) ;
#10599 = EDGE_LOOP ( 'NONE', ( #27398, #17362, #3068, #14836 ) ) ;
#10600 = ORIENTED_EDGE ( 'NONE', *, *, #15820, .F. ) ;
#10601 = CARTESIAN_POINT ( 'NONE',  ( -35.50000000000000000, -117.0140978167138854, 0.3752176474015736507 ) ) ;
#10602 = VECTOR ( 'NONE', #29328, 1000.000000000000000 ) ;
#10603 = EDGE_CURVE ( 'NONE', #18506, #26302, #24226, .T. ) ;
#10604 = CARTESIAN_POINT ( 'NONE',  ( 0.000000000000000000, 0.000000000000000000, 0.000000000000000000 ) ) ;
#10605 = ADVANCED_FACE ( 'NONE', ( #9646 ), #26394, .T. ) ;
#10606 = EDGE_CURVE ( 'NONE', #342, #8507, #11528, .T. ) ;
#10607 = DIRECTION ( 'NONE',  ( -1.000000000000000000, -0.000000000000000000, -0.000000000000000000 ) ) ;
#10608 = ORIENTED_EDGE ( 'NONE', *, *, #15367, .T. ) ;
#10609 = DIRECTION ( 'NONE',  ( -1.000000000000000000, -0.000000000000000000, -0.000000000000000000 ) ) ;
#10610 = CARTESIAN_POINT ( 'NONE',  ( -34.50000000000000000, -112.0221129971568104, -0.7553032835231431319 ) ) ;
#10611 = CARTESIAN_POINT ( 'NONE',  ( -37.98325232167028531, -114.9929510916434339, 14.04194344061727406 ) ) ;
#10612 = CYLINDRICAL_SURFACE ( 'NONE', #19458, 4.980000000000017302 ) ;
#10613 = CARTESIAN_POINT ( 'NONE',  ( -35.50000000000000000, -113.9929510916434339, 10.50625754673588474 ) ) ;
#10614 = LINE ( 'NONE', #2530, #32940 ) ;
#10615 = CARTESIAN_POINT ( 'NONE',  ( -34.50000000000000000, -114.9929510916434339, 10.59426868253284226 ) ) ;
#10616 = CYLINDRICAL_SURFACE ( 'NONE', #32004, 20.00000000000000355 ) ;
#10617 = EDGE_CURVE ( 'NONE', #34778, #892, #30504, .T. ) ;
#10618 = CARTESIAN_POINT ( 'NONE',  ( -38.00000000000000711, -114.9929510916434339, 11.91443571948719615 ) ) ;
#10619 = DIRECTION ( 'NONE',  ( 0.000000000000000000, 0.000000000000000000, -1.000000000000000000 ) ) ;
#10620 = VERTEX_POINT ( 'NONE', #29450 ) ;
#10621 = DIRECTION ( 'NONE',  ( 9.314451653655516225E-17, -6.938893903907203726E-17, -1.000000000000000000 ) ) ;
#10622 = FACE_OUTER_BOUND ( 'NONE', #35238, .T. ) ;
#10623 = ORIENTED_EDGE ( 'NONE', *, *, #17892, .F. ) ;
#10624 = CARTESIAN_POINT ( 'NONE',  ( -36.15625000000007816, -114.9929510916434339, 13.11852480586264669 ) ) ;
#10625 = EDGE_LOOP ( 'NONE', ( #8101, #26620, #15965, #25478, #32511, #9112, #26990, #33425, #7388, #30388, #31670, #4816 ) ) ;
#10626 = CARTESIAN_POINT ( 'NONE',  ( -39.02454729103295961, -114.7691647218148745, 8.159774454178448266 ) ) ;
#10627 = EDGE_CURVE ( 'NONE', #19767, #20378, #4795, .T. ) ;
#10628 = DIRECTION ( 'NONE',  ( 1.000000000000000000, -5.339440136655842133E-16, -1.047965281155519420E-16 ) ) ;
#10629 = EDGE_LOOP ( 'NONE', ( #30452, #32949, #34307, #569 ) ) ;
#10630 = ORIENTED_EDGE ( 'NONE', *, *, #6603, .T. ) ;
#10631 = AXIS2_PLACEMENT_3D ( 'NONE', #6773, #9299, #17745 ) ;
#10632 = CYLINDRICAL_SURFACE ( 'NONE', #13099, 4.800000000000000711 ) ;
#10633 = CIRCLE ( 'NONE', #29608, 8.000000000000014211 ) ;
#10634 = CARTESIAN_POINT ( 'NONE',  ( 8.000000000000000000, 9.471478019455140895, 14.71414642875960332 ) ) ;
#10635 = EDGE_LOOP ( 'NONE', ( #27706, #33507 ) ) ;
#10636 = CARTESIAN_POINT ( 'NONE',  ( -38.18337828418795965, -110.9754527089670546, 5.534774454178449155 ) ) ;
#10637 = EDGE_CURVE ( 'NONE', #3424, #30700, #1747, .T. ) ;
#10638 = VECTOR ( 'NONE', #12622, 1000.000000000000000 ) ;
#10639 = FACE_OUTER_BOUND ( 'NONE', #14013, .T. ) ;
#10640 = FACE_OUTER_BOUND ( 'NONE', #30525, .T. ) ;
#10641 = VERTEX_POINT ( 'NONE', #29092 ) ;
#10643 = VERTEX_POINT ( 'NONE', #28911 ) ;
#10642 = ADVANCED_FACE ( 'NONE', ( #20961 ), #1726, .T. ) ;
#10644 = FACE_OUTER_BOUND ( 'NONE', #32113, .T. ) ;
#10645 = DIRECTION ( 'NONE',  ( 1.000000000000000000, -0.000000000000000000, 0.000000000000000000 ) ) ;
#10647 = EDGE_LOOP ( 'NONE', ( #7972, #12904, #1069, #22324 ) ) ;
#10646 = VECTOR ( 'NONE', #26885, 1000.000000000000000 ) ;
#10648 = ORIENTED_EDGE ( 'NONE', *, *, #31759, .F. ) ;
#10649 = CARTESIAN_POINT ( 'NONE',  ( -34.50000000000000000, -111.0140978167138570, -0.3122823525984338988 ) ) ;
#10650 = EDGE_CURVE ( 'NONE', #24282, #35000, #18272, .T. ) ;
#10651 = CARTESIAN_POINT ( 'NONE',  ( 7.999999999999992895, 0.000000000000000000, 0.000000000000000000 ) ) ;
#10652 = ORIENTED_EDGE ( 'NONE', *, *, #24181, .T. ) ;
#10653 = EDGE_CURVE ( 'NONE', #19119, #19752, #21286, .T. ) ;
#10654 = CARTESIAN_POINT ( 'NONE',  ( -35.50000000000000711, -114.9929510916434339, 10.51175824272318415 ) ) ;
#10655 = AXIS2_PLACEMENT_3D ( 'NONE', #8257, #8083, #158 ) ;
#10656 = CARTESIAN_POINT ( 'NONE',  ( -36.62499999999902656, -113.9929510916434339, 14.11852480586265024 ) ) ;
#10657 = CIRCLE ( 'NONE', #15224, 0.5000000000000004441 ) ;
#10658 = DIRECTION ( 'NONE',  ( 0.000000000000000000, 0.3681245526846786964, -0.9297764858882511252 ) ) ;
#10659 = FACE_OUTER_BOUND ( 'NONE', #10201, .T. ) ;
#10660 = CARTESIAN_POINT ( 'NONE',  ( -38.00000000000000711, -113.9929510916434339, 11.21034663311206181 ) ) ;
#10661 = VECTOR ( 'NONE', #11625, 1000.000000000000000 ) ;
#10662 = CARTESIAN_POINT ( 'NONE',  ( -37.48437500000004263, -115.9929510916434481, 13.11852480586264846 ) ) ;
#10663 = CARTESIAN_POINT ( 'NONE',  ( 8.000000000000000000, -11.11653975335780942, -12.74840161668743299 ) ) ;
#10664 = AXIS2_PLACEMENT_3D ( 'NONE', #33092, #19042, #8585 ) ;
#10665 = PLANE ( 'NONE',  #11782 ) ;
#10666 = VERTEX_POINT ( 'NONE', #32319 ) ;
#10667 = DIRECTION ( 'NONE',  ( 1.000000000000000000, -4.524158825347490025E-15, -1.174092375852883357E-15 ) ) ;
#10668 = CARTESIAN_POINT ( 'NONE',  ( 0.000000000000000000, 0.000000000000000000, 0.000000000000000000 ) ) ;
#10669 = CARTESIAN_POINT ( 'NONE',  ( 3.799999999999999822, 0.000000000000000000, 35.10000000000000142 ) ) ;
#10670 = AXIS2_PLACEMENT_3D ( 'NONE', #12070, #23413, #33863 ) ;
#10671 = VERTEX_POINT ( 'NONE', #18089 ) ;
#10672 = DIRECTION ( 'NONE',  ( -1.000000000000000000, -0.000000000000000000, 0.000000000000000000 ) ) ;
#10673 = ORIENTED_EDGE ( 'NONE', *, *, #16872, .F. ) ;
#10674 = CARTESIAN_POINT ( 'NONE',  ( -35.50000000000000000, -113.1061333991432321, 0.8862035858144284850 ) ) ;
#10675 = DIRECTION ( 'NONE',  ( -1.000000000000000000, 0.000000000000000000, 0.000000000000000000 ) ) ;
#10676 = CARTESIAN_POINT ( 'NONE',  ( -35.50000000000000711, -114.9929510916434339, 10.56126450660895699 ) ) ;
#10677 = DIRECTION ( 'NONE',  ( -1.000000000000000000, -0.000000000000000000, 0.000000000000000000 ) ) ;
#10678 = EDGE_CURVE ( 'NONE', #28884, #34626, #28217, .T. ) ;
#10679 = ORIENTED_EDGE ( 'NONE', *, *, #24951, .T. ) ;
#10680 = ADVANCED_FACE ( 'NONE', ( #27816 ), #16092, .T. ) ;
#10681 = CARTESIAN_POINT ( 'NONE',  ( -39.49999999999999289, -1.387778780781445676E-14, 110.0000000000000000 ) ) ;
#10682 = CIRCLE ( 'NONE', #32513, 17.49900000000001299 ) ;
#10683 = CARTESIAN_POINT ( 'NONE',  ( -35.50000000000000000, -111.0140821919592327, -0.5779076015960634694 ) ) ;
#10684 = VERTEX_POINT ( 'NONE', #8535 ) ;
#10685 = ORIENTED_EDGE ( 'NONE', *, *, #24960, .F. ) ;
#10686 = CARTESIAN_POINT ( 'NONE',  ( -35.02454729103298803, -114.8876895276775087, 3.097274454178448710 ) ) ;
#10687 =( LENGTH_UNIT ( ) NAMED_UNIT ( * ) SI_UNIT ( .MILLI., .METRE. ) );
#10688 = CARTESIAN_POINT ( 'NONE',  ( 0.000000000000000000, 14.48509162075973755, -8.733917826871222090 ) ) ;
#10689 = EDGE_LOOP ( 'NONE', ( #12752, #6064 ) ) ;
#10690 = VERTEX_POINT ( 'NONE', #19160 ) ;
#10691 = CARTESIAN_POINT ( 'NONE',  ( -34.50000000000000000, -113.0140978167139991, 0.8595926474015699315 ) ) ;
#10692 = CARTESIAN_POINT ( 'NONE',  ( 0.000000000000000000, -3.753907720748892007, -8.725776631572756514 ) ) ;
#10693 = DIRECTION ( 'NONE',  ( 0.000000000000000000, 0.000000000000000000, 1.000000000000000000 ) ) ;
#10694 = FACE_OUTER_BOUND ( 'NONE', #27124, .T. ) ;
#10695 = CARTESIAN_POINT ( 'NONE',  ( -37.42187499999997158, -114.9929510916434339, 13.11852480586264669 ) ) ;
#10696 = CYLINDRICAL_SURFACE ( 'NONE', #19542, 13.99999999999999822 ) ;
#10697 = DIRECTION ( 'NONE',  ( 1.000000000000000000, -0.000000000000000000, 0.000000000000000000 ) ) ;
#10698 = CARTESIAN_POINT ( 'NONE',  ( -34.50000000000000000, -112.1222502514821144, 1.343475657184566296 ) ) ;
#10699 = CARTESIAN_POINT ( 'NONE',  ( -34.50000000000000000, -115.9929510916434481, 12.56351784598954424 ) ) ;
#10700 = CARTESIAN_POINT ( 'NONE',  ( 8.000000000000000000, -10.62435788049451624, 13.16139124467916588 ) ) ;
#10701 = AXIS2_PLACEMENT_3D ( 'NONE', #4389, #7777, #9778 ) ;
#10702 = CARTESIAN_POINT ( 'NONE',  ( 7.999999999999992895, 0.000000000000000000, 0.000000000000000000 ) ) ;
#10703 = VERTEX_POINT ( 'NONE', #30158 ) ;
#10704 = CARTESIAN_POINT ( 'NONE',  ( -35.50000000000000711, -114.1264797827112574, 9.515205387299289441 ) ) ;
#10705 = LINE ( 'NONE', #21675, #33189 ) ;
#10706 = DIRECTION ( 'NONE',  ( -1.000000000000000000, 0.000000000000000000, 0.000000000000000000 ) ) ;
#10707 = CARTESIAN_POINT ( 'NONE',  ( 1.479000000000007420, 1.339905674773393496E-15, 6.984000000000015085 ) ) ;
#10708 = CIRCLE ( 'NONE', #19325, 3.799999999999999822 ) ;
#10709 = CIRCLE ( 'NONE', #6101, 15.49900000000001121 ) ;
#10710 = DIRECTION ( 'NONE',  ( -1.000000000000000000, 0.000000000000000000, 0.000000000000000000 ) ) ;
#10711 = VERTEX_POINT ( 'NONE', #16453 ) ;
#10712 = CIRCLE ( 'NONE', #24520, 44.99999999999999289 ) ;
#10713 = CARTESIAN_POINT ( 'NONE',  ( 0.000000000000000000, 0.000000000000000000, 0.000000000000000000 ) ) ;
#10714 = DIRECTION ( 'NONE',  ( 0.02040816326530617286, -0.9997917317482359900, 9.329158281316450075E-32 ) ) ;
#10715 = CARTESIAN_POINT ( 'NONE',  ( 0.000000000000000000, -46.87740477351715640, -3.172455868805712509 ) ) ;
#10716 = CARTESIAN_POINT ( 'NONE',  ( -10.00000000000000000, 0.000000000000000000, 0.000000000000000000 ) ) ;
#10717 = LINE ( 'NONE', #13779, #9521 ) ;
#10718 = LINE ( 'NONE', #35580, #8994 ) ;
#10719 = VERTEX_POINT ( 'NONE', #30513 ) ;
#10720 = VECTOR ( 'NONE', #9108, 1000.000000000000000 ) ;
#10721 = VERTEX_POINT ( 'NONE', #24402 ) ;
#10722 = EDGE_CURVE ( 'NONE', #24884, #16008, #5844, .T. ) ;
#10723 = DIRECTION ( 'NONE',  ( 1.000000000000000000, 0.000000000000000000, 0.000000000000000000 ) ) ;
#10724 = CARTESIAN_POINT ( 'NONE',  ( 8.000000000000007105, 3.753907720749127819, 8.725776631572756514 ) ) ;
#10725 = DIRECTION ( 'NONE',  ( -1.000000000000000000, 0.000000000000000000, 0.000000000000000000 ) ) ;
#10726 = ORIENTED_EDGE ( 'NONE', *, *, #34096, .F. ) ;
#10727 = CARTESIAN_POINT ( 'NONE',  ( -36.23083527818512550, -111.9754527089670404, 6.715225545821551734 ) ) ;
#10728 = VERTEX_POINT ( 'NONE', #2984 ) ;
#10729 = PRESENTATION_STYLE_ASSIGNMENT (( #7657 ) ) ;
#10730 = EDGE_LOOP ( 'NONE', ( #9256, #4729, #21645, #18333 ) ) ;
#10731 = ORIENTED_EDGE ( 'NONE', *, *, #28365, .F. ) ;
#10732 = FACE_BOUND ( 'NONE', #1389, .T. ) ;
#10733 = AXIS2_PLACEMENT_3D ( 'NONE', #12260, #25783, #8833 ) ;
#10734 = EDGE_CURVE ( 'NONE', #891, #16728, #27110, .T. ) ;
#10735 = AXIS2_PLACEMENT_3D ( 'NONE', #29539, #15638, #32051 ) ;
#10736 = CIRCLE ( 'NONE', #23953, 4.980000000000017302 ) ;
#10737 = DIRECTION ( 'NONE',  ( -1.000000000000000000, 0.000000000000000000, 0.000000000000000000 ) ) ;
#10738 = ORIENTED_EDGE ( 'NONE', *, *, #34015, .F. ) ;
#10739 = ORIENTED_EDGE ( 'NONE', *, *, #33511, .T. ) ;
#10740 = CIRCLE ( 'NONE', #12458, 0.6000000000000029754 ) ;
#10741 = CARTESIAN_POINT ( 'NONE',  ( -36.49999999999999289, -11.24969279549607748, 111.5585998451919778 ) ) ;
#10742 = DIRECTION ( 'NONE',  ( 1.000000000000000000, -0.000000000000000000, 0.000000000000000000 ) ) ;
#10743 = VECTOR ( 'NONE', #9283, 1000.000000000000000 ) ;
#10744 = CARTESIAN_POINT ( 'NONE',  ( 38.00000000000000000, 1.391938065904714129E-14, 3.000000000000002665 ) ) ;
#10745 = CIRCLE ( 'NONE', #7851, 4.800000000000006040 ) ;
#10746 = CIRCLE ( 'NONE', #14759, 47.49900000000001654 ) ;
#10747 = CARTESIAN_POINT ( 'NONE',  ( -3.799999999999999822, -2.710505431213761085E-17, 45.89999999999999858 ) ) ;
#10748 = CARTESIAN_POINT ( 'NONE',  ( 4.000000000000003553, -13.42368113696662490, -3.975523202428152381 ) ) ;
#10749 = DIRECTION ( 'NONE',  ( 0.000000000000000000, 0.6845471059286846183, 0.7289686274214153272 ) ) ;
#10750 = CARTESIAN_POINT ( 'NONE',  ( -37.88878409051687157, -115.9929510916434481, 14.07058620477052280 ) ) ;
#10751 = LINE ( 'NONE', #13285, #30894 ) ;
#10752 = FACE_OUTER_BOUND ( 'NONE', #9709, .T. ) ;
#10753 = CIRCLE ( 'NONE', #17049, 9.999999999999994671 ) ;
#10754 = CARTESIAN_POINT ( 'NONE',  ( 8.000000000000007105, -1.111908866155156161, 9.433698091065117808 ) ) ;
#10755 = DIRECTION ( 'NONE',  ( 0.000000000000000000, 0.000000000000000000, -1.000000000000000000 ) ) ;
#10756 = AXIS2_PLACEMENT_3D ( 'NONE', #20011, #11935, #5659 ) ;
#10757 = DIRECTION ( 'NONE',  ( -1.000000000000000000, 0.000000000000000000, 0.000000000000000000 ) ) ;
#10758 = DIRECTION ( 'NONE',  ( 0.000000000000000000, 0.000000000000000000, 1.000000000000000000 ) ) ;
#10759 = ORIENTED_EDGE ( 'NONE', *, *, #13704, .T. ) ;
#10760 = CARTESIAN_POINT ( 'NONE',  ( -38.97545270896704039, -114.8876895276775087, 4.652725545821551734 ) ) ;
#10761 = FACE_OUTER_BOUND ( 'NONE', #13733, .T. ) ;
#10762 = DIRECTION ( 'NONE',  ( 0.000000000000000000, 0.000000000000000000, -1.000000000000000000 ) ) ;
#10763 = DIRECTION ( 'NONE',  ( 0.000000000000000000, 0.000000000000000000, 1.000000000000000000 ) ) ;
#10764 = VERTEX_POINT ( 'NONE', #2449 ) ;
#10765 = VERTEX_POINT ( 'NONE', #19333 ) ;
#10766 = AXIS2_PLACEMENT_3D ( 'NONE', #28124, #30645, #8843 ) ;
#10767 = UNCERTAINTY_MEASURE_WITH_UNIT (LENGTH_MEASURE( 1.000000000000000082E-05 ), #34242, 'distance_accuracy_value', 'NONE');
#10768 = EDGE_CURVE ( 'NONE', #30211, #24075, #14391, .T. ) ;
#10769 = SURFACE_STYLE_FILL_AREA ( #30038 ) ;
#10770 = DIRECTION ( 'NONE',  ( 0.000000000000000000, 0.9980267284282712259, 0.06279051952931682945 ) ) ;
#10771 = VERTEX_POINT ( 'NONE', #5325 ) ;
#10772 = EDGE_CURVE ( 'NONE', #12651, #30694, #25909, .T. ) ;
#10773 = AXIS2_PLACEMENT_3D ( 'NONE', #24220, #24756, #32483 ) ;
#10774 = VECTOR ( 'NONE', #14680, 1000.000000000000000 ) ;
#10775 = ORIENTED_EDGE ( 'NONE', *, *, #34299, .F. ) ;
#10776 = CARTESIAN_POINT ( 'NONE',  ( 50.00000000000000711, -2.775557561562891351E-14, 110.0000000000000000 ) ) ;
#10777 = FACE_OUTER_BOUND ( 'NONE', #13164, .T. ) ;
#10778 = EDGE_CURVE ( 'NONE', #16643, #32151, #24761, .T. ) ;
#10779 = DIRECTION ( 'NONE',  ( -0.9999999999999998890, -1.836970198680994997E-16, -1.109924098441123339E-27 ) ) ;
#10780 = CARTESIAN_POINT ( 'NONE',  ( -55.00000000000000000, 0.000000000000000000, 70.00000000000000000 ) ) ;
#10781 = AXIS2_PLACEMENT_3D ( 'NONE', #7678, #7856, #2662 ) ;
#10782 = ORIENTED_EDGE ( 'NONE', *, *, #2731, .T. ) ;
#10783 = VERTEX_POINT ( 'NONE', #11075 ) ;
#10784 = ADVANCED_FACE ( 'NONE', ( #22043 ), #35389, .T. ) ;
#10785 = VECTOR ( 'NONE', #30623, 1000.000000000000000 ) ;
#10786 = FACE_BOUND ( 'NONE', #25248, .T. ) ;
#10787 = DIRECTION ( 'NONE',  ( 1.000000000000000000, -5.339440136655842133E-16, -1.047965281155519420E-16 ) ) ;
#10788 = EDGE_LOOP ( 'NONE', ( #16608, #24749, #32910, #20250 ) ) ;
#10789 = LINE ( 'NONE', #29348, #12058 ) ;
#10790 = VECTOR ( 'NONE', #24502, 1000.000000000000000 ) ;
#10791 = CARTESIAN_POINT ( 'NONE',  ( -34.50000000000000000, -115.0468226098135744, -1.624774171496087716 ) ) ;
#10792 = CIRCLE ( 'NONE', #12506, 47.49900000000000944 ) ;
#10793 = CARTESIAN_POINT ( 'NONE',  ( -35.90191880024783444, -114.9929510916434339, 14.11551573851448893 ) ) ;
#10794 = LINE ( 'NONE', #2528, #17133 ) ;
#10795 = CARTESIAN_POINT ( 'NONE',  ( -35.50000000000000000, -113.8814751941377352, 10.49295109164313722 ) ) ;
#10796 = CARTESIAN_POINT ( 'NONE',  ( 0.000000000000000000, 1.111908866155322695, -9.433698091065103597 ) ) ;
#10797 = CARTESIAN_POINT ( 'NONE',  ( -34.50015059926905536, -114.9929510916434339, 12.64306614848962695 ) ) ;
#10798 = CARTESIAN_POINT ( 'NONE',  ( 8.000000000000000000, -7.317194182740013098, -18.61340026142654480 ) ) ;
#10799 = CIRCLE ( 'NONE', #15364, 8.000000000000015987 ) ;
#10800 = ADVANCED_FACE ( 'NONE', ( #13420 ), #13944, .T. ) ;
#10801 = DIRECTION ( 'NONE',  ( -1.000000000000000000, -0.000000000000000000, -0.000000000000000000 ) ) ;
#10802 = CARTESIAN_POINT ( 'NONE',  ( 0.000000000000000000, 0.000000000000000000, -32.00000000000000000 ) ) ;
#10803 = ORIENTED_EDGE ( 'NONE', *, *, #5691, .F. ) ;
#10804 = CARTESIAN_POINT ( 'NONE',  ( 4.000000000000003553, 30.03615769709793426, -42.44795908868959344 ) ) ;
#10805 = LINE ( 'NONE', #15816, #14614 ) ;
#10806 = ORIENTED_EDGE ( 'NONE', *, *, #30517, .T. ) ;
#10807 = CARTESIAN_POINT ( 'NONE',  ( -36.07812499999994316, -114.9929510916434339, 13.11852480586264669 ) ) ;
#10808 = EDGE_LOOP ( 'NONE', ( #32725, #19504, #19347, #18865, #7430 ) ) ;
#10809 = CARTESIAN_POINT ( 'NONE',  ( -38.99999999999999289, -113.9407375970686900, 6.753524454178448266 ) ) ;
#10810 = DIRECTION ( 'NONE',  ( 9.314451653655516225E-17, -6.938893903907203726E-17, -1.000000000000000000 ) ) ;
#10811 = CIRCLE ( 'NONE', #23451, 20.00000000000000711 ) ;
#10812 = ORIENTED_EDGE ( 'NONE', *, *, #3429, .T. ) ;
#10813 = ORIENTED_EDGE ( 'NONE', *, *, #1405, .F. ) ;
#10814 = CIRCLE ( 'NONE', #26337, 20.00000000000000711 ) ;
#10815 = EDGE_CURVE ( 'NONE', #15158, #27081, #16683, .T. ) ;
#10816 = DIRECTION ( 'NONE',  ( 0.000000000000000000, 0.000000000000000000, -1.000000000000000000 ) ) ;
#10817 = FACE_OUTER_BOUND ( 'NONE', #20873, .T. ) ;
#10818 = EDGE_CURVE ( 'NONE', #24162, #12885, #5781, .T. ) ;
#10819 = VECTOR ( 'NONE', #20854, 1000.000000000000000 ) ;
#10820 = EDGE_CURVE ( 'NONE', #2288, #6915, #19009, .T. ) ;
#10821 = VERTEX_POINT ( 'NONE', #27284 ) ;
#10822 = CARTESIAN_POINT ( 'NONE',  ( -37.05926240293133134, -116.9999999999999858, 6.378524454178448266 ) ) ;
#10823 = AXIS2_PLACEMENT_3D ( 'NONE', #2865, #5895, #33433 ) ;
#10824 = DIRECTION ( 'NONE',  ( -1.000000000000000000, 0.000000000000000000, -0.000000000000000000 ) ) ;
#10825 = CARTESIAN_POINT ( 'NONE',  ( 3.799999999999999822, -2.710505431213761085E-17, 45.10000000000000142 ) ) ;
#10826 = VERTEX_POINT ( 'NONE', #16805 ) ;
#10827 = ORIENTED_EDGE ( 'NONE', *, *, #35179, .F. ) ;
#10828 = CARTESIAN_POINT ( 'NONE',  ( 8.000000000000007105, 1.111908866155322695, -9.433698091065103597 ) ) ;
#10829 = EDGE_CURVE ( 'NONE', #16551, #5076, #2628, .T. ) ;
#10830 = MECHANICAL_DESIGN_GEOMETRIC_PRESENTATION_REPRESENTATION (  '', ( #4521 ), #13125 ) ;
#10831 = EDGE_CURVE ( 'NONE', #12890, #35474, #24750, .T. ) ;
#10832 = CARTESIAN_POINT ( 'NONE',  ( -1.799999999999996492, 8.057851996059937582E-16, 4.200000000000014388 ) ) ;
#10833 = EDGE_LOOP ( 'NONE', ( #33185, #23415, #1996, #18028 ) ) ;
#10834 = VERTEX_POINT ( 'NONE', #7825 ) ;
#10835 = CARTESIAN_POINT ( 'NONE',  ( -34.50000000000000000, -114.3474311500471572, -2.624782352598442614 ) ) ;
#10836 = DIRECTION ( 'NONE',  ( -1.000000000000000000, 0.000000000000000000, 0.000000000000000000 ) ) ;
#10837 = ORIENTED_EDGE ( 'NONE', *, *, #22288, .F. ) ;
#10838 = CARTESIAN_POINT ( 'NONE',  ( -35.50000000000000711, -114.0371586325023117, 9.504435485030890973 ) ) ;
#10839 = CARTESIAN_POINT ( 'NONE',  ( -34.50000000000000000, -113.9929510916434339, 12.44250253426871033 ) ) ;
#10840 = LINE ( 'NONE', #21798, #24640 ) ;
#10841 = DIRECTION ( 'NONE',  ( -1.000000000000000000, 0.000000000000000000, 0.000000000000000000 ) ) ;
#10842 = CARTESIAN_POINT ( 'NONE',  ( -34.50000000000000000, -113.9929510916434339, 12.59102132592610346 ) ) ;
#10843 = CARTESIAN_POINT ( 'NONE',  ( -37.74437085908087397, -114.9929510916434339, 14.09929883582536903 ) ) ;
#10844 = EDGE_CURVE ( 'NONE', #25690, #11512, #18813, .T. ) ;
#10845 = CARTESIAN_POINT ( 'NONE',  ( -35.50000000000000711, -114.9929510916434339, 10.61627146648203812 ) ) ;
#10846 = DIRECTION ( 'NONE',  ( -1.000000000000000000, 0.000000000000000000, 0.000000000000000000 ) ) ;
#10847 = CARTESIAN_POINT ( 'NONE',  ( 7.999999999999992895, 51.19683565102445044, 9.104066087303644750 ) ) ;
#10848 = EDGE_CURVE ( 'NONE', #864, #32025, #8881, .T. ) ;
#10849 = VERTEX_POINT ( 'NONE', #9248 ) ;
#10850 = EDGE_CURVE ( 'NONE', #21098, #3168, #22560, .T. ) ;
#10851 = DIRECTION ( 'NONE',  ( 9.314451653655516225E-17, -6.938893903907203726E-17, -1.000000000000000000 ) ) ;
#10852 = DIRECTION ( 'NONE',  ( 1.000000000000000000, 1.836970198721029934E-16, 0.000000000000000000 ) ) ;
#10853 = CARTESIAN_POINT ( 'NONE',  ( -46.00000000000000000, 0.000000000000000000, 11.00000000000000000 ) ) ;
#10854 = ORIENTED_EDGE ( 'NONE', *, *, #6401, .T. ) ;
#10855 = CARTESIAN_POINT ( 'NONE',  ( 7.999999999999992895, 31.08872492059958148, 41.68322423723111569 ) ) ;
#10856 = ORIENTED_EDGE ( 'NONE', *, *, #24635, .T. ) ;
#10857 = CARTESIAN_POINT ( 'NONE',  ( -35.50000000000000000, -113.7503824761461004, 0.9631051547057219997 ) ) ;
#10858 = DIRECTION ( 'NONE',  ( 1.000000000000000000, -0.000000000000000000, -0.000000000000000000 ) ) ;
#10859 = CARTESIAN_POINT ( 'NONE',  ( -37.99999999999998579, -113.9407375970686758, 6.753524454178450043 ) ) ;
#10860 = EDGE_CURVE ( 'NONE', #4114, #32945, #3497, .T. ) ;
#10861 = EDGE_CURVE ( 'NONE', #4012, #9519, #25103, .T. ) ;
#10862 = CARTESIAN_POINT ( 'NONE',  ( -35.50000000000000711, -114.9929510916434339, 12.59102132592610523 ) ) ;
#10863 = CARTESIAN_POINT ( 'NONE',  ( 0.000000000000000000, 6.336799421340039373, -16.31134495048478428 ) ) ;
#10864 = ORIENTED_EDGE ( 'NONE', *, *, #11093, .F. ) ;
#10865 = DIRECTION ( 'NONE',  ( 1.000000000000000000, 0.000000000000000000, 0.000000000000000000 ) ) ;
#10866 = CARTESIAN_POINT ( 'NONE',  ( -35.50000000000000000, -111.0140978167138570, 0.7189676474015717078 ) ) ;
#10867 = ORIENTED_EDGE ( 'NONE', *, *, #24743, .F. ) ;
#10868 = ORIENTED_EDGE ( 'NONE', *, *, #19386, .F. ) ;
#10869 = CARTESIAN_POINT ( 'NONE',  ( -37.05926240293131713, -115.9999999999999858, 1.878524454178448710 ) ) ;
#10870 = CIRCLE ( 'NONE', #11990, 19.99999999999998579 ) ;
#10871 = EDGE_CURVE ( 'NONE', #9085, #20492, #30858, .T. ) ;
#10872 = LINE ( 'NONE', #21296, #21559 ) ;
#10873 = ORIENTED_EDGE ( 'NONE', *, *, #14483, .F. ) ;
#10874 = ORIENTED_EDGE ( 'NONE', *, *, #20988, .T. ) ;
#10875 = CIRCLE ( 'NONE', #22336, 7.800000000000051337 ) ;
#10876 = CARTESIAN_POINT ( 'NONE',  ( -34.50000000000000000, -115.0140978167138712, -0.6247823525984408377 ) ) ;
#10877 = CARTESIAN_POINT ( 'NONE',  ( -34.49999999999998579, -12.79398423610758684, 91.86693750936007064 ) ) ;
#10878 = LINE ( 'NONE', #32834, #16629 ) ;
#10879 = PLANE ( 'NONE',  #22562 ) ;
#10880 = CARTESIAN_POINT ( 'NONE',  ( -35.50000000000000000, -113.9929510916434339, 11.21034663311132107 ) ) ;
#10881 = CARTESIAN_POINT ( 'NONE',  ( 7.999999999999992895, 44.75336757549778355, 14.30704879393622520 ) ) ;
#10882 = CARTESIAN_POINT ( 'NONE',  ( -34.50000000000001421, -39.95319397786859383, 75.20096189432314304 ) ) ;
#10883 = CARTESIAN_POINT ( 'NONE',  ( -34.50000000000000000, -114.9307644833806137, -1.624782352598427959 ) ) ;
#10884 = ADVANCED_FACE ( 'NONE', ( #16977 ), #17329, .F. ) ;
#10885 = CARTESIAN_POINT ( 'NONE',  ( -35.75562914091914024, -115.9929510916434481, 14.09929883582542409 ) ) ;
#10886 = DIRECTION ( 'NONE',  ( 0.000000000000000000, 0.2486898871648552389, -0.9685831611286309650 ) ) ;
#10887 = EDGE_CURVE ( 'NONE', #31530, #7529, #14454, .T. ) ;
#10888 = DIRECTION ( 'NONE',  ( 1.000000000000000000, 1.836970198721029934E-16, 0.000000000000000000 ) ) ;
#10889 = ORIENTED_EDGE ( 'NONE', *, *, #21777, .F. ) ;
#10890 = AXIS2_PLACEMENT_3D ( 'NONE', #25892, #20628, #17759 ) ;
#10891 = CARTESIAN_POINT ( 'NONE',  ( -37.99599240977853754, -115.9929510916434481, 12.68378527132499656 ) ) ;
#10892 = DIRECTION ( 'NONE',  ( 0.000000000000000000, 0.000000000000000000, 1.000000000000000000 ) ) ;
#10893 = SURFACE_STYLE_USAGE ( .BOTH. , #13583 ) ;
#10894 = CARTESIAN_POINT ( 'NONE',  ( -90.00000000000002842, 1.346812405055736621E-15, 7.020000000000052864 ) ) ;
#10895 = FACE_OUTER_BOUND ( 'NONE', #9100, .T. ) ;
#10896 = ORIENTED_EDGE ( 'NONE', *, *, #7502, .F. ) ;
#10897 = AXIS2_PLACEMENT_3D ( 'NONE', #3662, #27793, #233 ) ;
#10898 = CARTESIAN_POINT ( 'NONE',  ( 7.999999999999992895, 26.17370628620655637, 39.63700417846175128 ) ) ;
#10899 = CARTESIAN_POINT ( 'NONE',  ( 8.000000000000000000, 0.000000000000000000, 0.000000000000000000 ) ) ;
#10900 = DIRECTION ( 'NONE',  ( -1.000000000000000000, 0.000000000000000000, 0.000000000000000000 ) ) ;
#10901 = DIRECTION ( 'NONE',  ( -1.000000000000000000, 0.000000000000000000, 0.000000000000000000 ) ) ;
#10902 = ADVANCED_FACE ( 'NONE', ( #19673 ), #30687, .F. ) ;
#10903 = AXIS2_PLACEMENT_3D ( 'NONE', #377, #11376, #26254 ) ;
#10904 = CARTESIAN_POINT ( 'NONE',  ( -44.00000000000000711, 19.99999999999999645, 2.449293598294706119E-15 ) ) ;
#10905 = DIRECTION ( 'NONE',  ( 1.000000000000000000, -4.336808689941996437E-15, -1.174092375852883357E-15 ) ) ;
#10906 = ORIENTED_EDGE ( 'NONE', *, *, #23573, .F. ) ;
#10907 = EDGE_LOOP ( 'NONE', ( #17159, #14592, #6989, #27979 ) ) ;
#10908 = CARTESIAN_POINT ( 'NONE',  ( -10.00000000000000000, 0.000000000000000000, 0.000000000000000000 ) ) ;
#10909 = DIRECTION ( 'NONE',  ( 0.000000000000000000, 0.9048270524660205760, -0.4257792915650703836 ) ) ;
#10910 = CARTESIAN_POINT ( 'NONE',  ( 8.000000000000000000, 19.83898331853685448, 9.508666619816709797 ) ) ;
#10911 = ORIENTED_EDGE ( 'NONE', *, *, #16025, .T. ) ;
#10912 = CARTESIAN_POINT ( 'NONE',  ( -39.02454729103295961, -113.2308352781851539, 9.340225545821549957 ) ) ;
#10913 = EDGE_LOOP ( 'NONE', ( #33706, #23319, #6990, #8227, #4017, #8572, #5390, #15432 ) ) ;
#10914 =( NAMED_UNIT ( * ) SI_UNIT ( $, .STERADIAN. ) SOLID_ANGLE_UNIT ( ) );
#10915 = VERTEX_POINT ( 'NONE', #23095 ) ;
#10916 = ORIENTED_EDGE ( 'NONE', *, *, #34140, .T. ) ;
#10917 = CARTESIAN_POINT ( 'NONE',  ( 8.000000000000000000, -5.482169781018729537, -16.00140663693126086 ) ) ;
#10918 = CYLINDRICAL_SURFACE ( 'NONE', #15616, 8.000000000000001776 ) ;
#10919 = ORIENTED_EDGE ( 'NONE', *, *, #34176, .T. ) ;
#10920 = AXIS2_PLACEMENT_3D ( 'NONE', #3042, #19734, #11314 ) ;
#10921 = CARTESIAN_POINT ( 'NONE',  ( -35.50000000000000711, -114.0371586325023117, 9.504435485030890973 ) ) ;
#10922 = FACE_BOUND ( 'NONE', #17086, .T. ) ;
#10923 = AXIS2_PLACEMENT_3D ( 'NONE', #26575, #29631, #2283 ) ;
#10924 = LINE ( 'NONE', #10976, #2625 ) ;
#10925 = FACE_BOUND ( 'NONE', #9017, .T. ) ;
#10926 = VECTOR ( 'NONE', #22280, 1000.000000000000000 ) ;
#10927 = CARTESIAN_POINT ( 'NONE',  ( 0.000000000000000000, 0.000000000000000000, 0.000000000000000000 ) ) ;
#10928 = DIRECTION ( 'NONE',  ( 1.000000000000000000, -0.000000000000000000, 0.000000000000000000 ) ) ;
#10929 = EDGE_CURVE ( 'NONE', #24948, #6464, #27068, .T. ) ;
#10930 = DIRECTION ( 'NONE',  ( 0.000000000000000000, -0.9848077530122062440, -0.1736481776669401844 ) ) ;
#10931 = CARTESIAN_POINT ( 'NONE',  ( -36.31249999999994316, -115.9929510916434481, 14.11852480586265024 ) ) ;
#10932 = CARTESIAN_POINT ( 'NONE',  ( -34.49999999999998579, -39.90017302060827831, 83.49999999999991473 ) ) ;
#10933 = CARTESIAN_POINT ( 'NONE',  ( 65.00000000000001421, -25.99649394950422021, 81.00003093645240426 ) ) ;
#10934 = FACE_OUTER_BOUND ( 'NONE', #13823, .T. ) ;
#10935 = DIRECTION ( 'NONE',  ( -1.000000000000000000, -0.000000000000000000, -0.000000000000000000 ) ) ;
#10936 = FACE_OUTER_BOUND ( 'NONE', #10549, .T. ) ;
#10937 = SURFACE_SIDE_STYLE ('',( #8393 ) ) ;
#10938 = ORIENTED_EDGE ( 'NONE', *, *, #21207, .F. ) ;
#10939 = CIRCLE ( 'NONE', #31052, 6.000000000000005329 ) ;
#10940 = CARTESIAN_POINT ( 'NONE',  ( -37.88768952767750875, -112.0245472910329880, 6.527725545821550845 ) ) ;
#10941 = DIRECTION ( 'NONE',  ( 0.000000000000000000, 0.000000000000000000, -1.000000000000000000 ) ) ;
#10942 = LINE ( 'NONE', #6852, #17622 ) ;
#10943 = DIRECTION ( 'NONE',  ( -1.000000000000000000, 0.000000000000000000, 0.000000000000000000 ) ) ;
#10944 = ORIENTED_EDGE ( 'NONE', *, *, #30449, .T. ) ;
#10945 = VECTOR ( 'NONE', #26297, 1000.000000000000000 ) ;
#10946 = ORIENTED_EDGE ( 'NONE', *, *, #17089, .T. ) ;
#10947 = LINE ( 'NONE', #19207, #24429 ) ;
#10948 = EDGE_LOOP ( 'NONE', ( #35273, #16777, #2360, #26444 ) ) ;
#10949 = VERTEX_POINT ( 'NONE', #14283 ) ;
#10950 = AXIS2_PLACEMENT_3D ( 'NONE', #4440, #24933, #10901 ) ;
#10951 = AXIS2_PLACEMENT_3D ( 'NONE', #8800, #3248, #33473 ) ;
#10952 = CIRCLE ( 'NONE', #602, 3.799999999999999822 ) ;
#10953 = DIRECTION ( 'NONE',  ( -1.000000000000000000, 0.000000000000000000, 0.000000000000000000 ) ) ;
#10954 = DIRECTION ( 'NONE',  ( -1.000000000000000000, 0.000000000000000000, 0.000000000000000000 ) ) ;
#10955 = DIRECTION ( 'NONE',  ( -1.000000000000000000, -5.551115123125782702E-17, 3.538022753612654186E-17 ) ) ;
#10956 = CARTESIAN_POINT ( 'NONE',  ( 4.000000000000003553, 15.92965478239619515, 15.17386234660388844 ) ) ;
#10957 = ORIENTED_EDGE ( 'NONE', *, *, #27618, .F. ) ;
#10958 = VERTEX_POINT ( 'NONE', #20201 ) ;
#10959 = CARTESIAN_POINT ( 'NONE',  ( 50.00000000000000711, -25.98076211353320275, 84.99999999999994316 ) ) ;
#10960 = CIRCLE ( 'NONE', #31079, 4.000000000000000000 ) ;
#10961 = CARTESIAN_POINT ( 'NONE',  ( 0.000000000000000000, 0.000000000000000000, 0.000000000000000000 ) ) ;
#10962 = ORIENTED_EDGE ( 'NONE', *, *, #31285, .F. ) ;
#10963 = DIRECTION ( 'NONE',  ( -1.000000000000000000, -1.734723475976807094E-16, 0.000000000000000000 ) ) ;
#10964 = VECTOR ( 'NONE', #15771, 1000.000000000000000 ) ;
#10965 = CARTESIAN_POINT ( 'NONE',  ( -34.50000000000000000, -112.0140900043366088, -0.5935324770972457697 ) ) ;
#10966 = EDGE_CURVE ( 'NONE', #31461, #19641, #8058, .T. ) ;
#10967 = CARTESIAN_POINT ( 'NONE',  ( -37.37500000000009237, -114.9929510916434339, 14.11852480586264846 ) ) ;
#10968 = EDGE_CURVE ( 'NONE', #29341, #32249, #6718, .T. ) ;
#10969 = CARTESIAN_POINT ( 'NONE',  ( -38.00000000000000711, -114.9929510916434339, 12.17846912687782179 ) ) ;
#10970 = DIRECTION ( 'NONE',  ( 1.000000000000000000, -0.000000000000000000, -0.000000000000000000 ) ) ;
#10971 = AXIS2_PLACEMENT_3D ( 'NONE', #18411, #4756, #15699 ) ;
#10972 = CARTESIAN_POINT ( 'NONE',  ( -34.50000000000000000, -114.9929510916434339, 11.91443571948719971 ) ) ;
#10974 = CYLINDRICAL_SURFACE ( 'NONE', #10190, 8.000000000000000000 ) ;
#10973 = VECTOR ( 'NONE', #26689, 1000.000000000000000 ) ;
#10975 = CARTESIAN_POINT ( 'NONE',  ( 3.799999999999999822, 0.000000000000000000, -31.10000000000000142 ) ) ;
#10976 = CARTESIAN_POINT ( 'NONE',  ( 7.999999999999992895, -34.03046037009280411, 33.13733193845794034 ) ) ;
#10977 = DIRECTION ( 'NONE',  ( -1.000000000000000000, -0.000000000000000000, -0.000000000000000000 ) ) ;
#10978 = CYLINDRICAL_SURFACE ( 'NONE', #12340, 13.99999999999999822 ) ;
#10979 = ORIENTED_EDGE ( 'NONE', *, *, #15449, .F. ) ;
#10980 = DIRECTION ( 'NONE',  ( -1.000000000000000000, 0.000000000000000000, 0.000000000000000000 ) ) ;
#10981 = ORIENTED_EDGE ( 'NONE', *, *, #5587, .T. ) ;
#10982 = EDGE_CURVE ( 'NONE', #12448, #16934, #33942, .T. ) ;
#10983 = CARTESIAN_POINT ( 'NONE',  ( -39.07941549657748936, -111.8367748094582055, 5.441024454178449155 ) ) ;
#10984 = CARTESIAN_POINT ( 'NONE',  ( -42.49999999999999289, -24.48076211353326315, 88.99999999999994316 ) ) ;
#10985 = ORIENTED_EDGE ( 'NONE', *, *, #22566, .T. ) ;
#10986 = ORIENTED_EDGE ( 'NONE', *, *, #1285, .T. ) ;
#10987 = DIRECTION ( 'NONE',  ( -1.000000000000000000, 0.000000000000000000, 0.000000000000000000 ) ) ;
#10988 = DIRECTION ( 'NONE',  ( 0.000000000000000000, -0.4999999999999891753, -0.8660254037844450359 ) ) ;
#10989 = VERTEX_POINT ( 'NONE', #22385 ) ;
#10990 = CARTESIAN_POINT ( 'NONE',  ( -34.00000000000000000, -113.9407375970686758, 3.996475545821551734 ) ) ;
#10991 = DIRECTION ( 'NONE',  ( 0.000000000000000000, 0.000000000000000000, -1.000000000000000000 ) ) ;
#10992 = DIRECTION ( 'NONE',  ( 0.000000000000000000, 0.000000000000000000, 1.000000000000000000 ) ) ;
#10993 = EDGE_LOOP ( 'NONE', ( #23531, #4686, #19987, #30426 ) ) ;
#10994 = ORIENTED_EDGE ( 'NONE', *, *, #9496, .T. ) ;
#10995 = CYLINDRICAL_SURFACE ( 'NONE', #3353, 20.00000000000000355 ) ;
#10996 = AXIS2_PLACEMENT_3D ( 'NONE', #19736, #22990, #17226 ) ;
#10997 = VECTOR ( 'NONE', #3784, 1000.000000000000000 ) ;
#10998 = EDGE_CURVE ( 'NONE', #6287, #21466, #24185, .T. ) ;
#10999 = CARTESIAN_POINT ( 'NONE',  ( 46.00000000000000000, 0.000000000000000000, 0.000000000000000000 ) ) ;
#11000 = ORIENTED_EDGE ( 'NONE', *, *, #20898, .T. ) ;
#11001 = ORIENTED_EDGE ( 'NONE', *, *, #35459, .T. ) ;
#11002 = CARTESIAN_POINT ( 'NONE',  ( -35.50000000000000000, -111.0140978167138570, 0.2502176474015764263 ) ) ;
#11003 = PRODUCT_DEFINITION_SHAPE ( 'NONE', 'NONE',  #35652 ) ;
#11004 = CARTESIAN_POINT ( 'NONE',  ( 7.999999999999992895, -36.05989434073592292, -30.12041790338657066 ) ) ;
#11005 = EDGE_LOOP ( 'NONE', ( #17824, #22868, #33564, #20176 ) ) ;
#11006 = CARTESIAN_POINT ( 'NONE',  ( 7.999999999999992895, 29.60891106212840285, -37.14118181634734839 ) ) ;
#11007 = EDGE_CURVE ( 'NONE', #30, #2768, #33380, .T. ) ;
#11008 = CARTESIAN_POINT ( 'NONE',  ( -34.50000000000000000, -113.9929510916434339, 10.68227981832981044 ) ) ;
#11009 = EDGE_CURVE ( 'NONE', #5065, #8132, #28161, .T. ) ;
#11010 = LINE ( 'NONE', #13881, #29249 ) ;
#11011 = AXIS2_PLACEMENT_3D ( 'NONE', #5185, #24257, #35244 ) ;
#11012 = DIRECTION ( 'NONE',  ( -1.000000000000000000, -0.000000000000000000, -0.000000000000000000 ) ) ;
#11013 = EDGE_CURVE ( 'NONE', #6235, #32406, #20026, .T. ) ;
#11014 = CARTESIAN_POINT ( 'NONE',  ( -34.68937937320795584, -113.9929510916434339, 13.37409560816408671 ) ) ;
#11015 = CARTESIAN_POINT ( 'NONE',  ( -38.98077402996267438, -114.9929510916434339, 12.86289566494346204 ) ) ;
#11016 = CARTESIAN_POINT ( 'NONE',  ( -35.50000000000000711, -114.0371586325023117, 9.504435485030890973 ) ) ;
#11017 =( NAMED_UNIT ( * ) SI_UNIT ( $, .STERADIAN. ) SOLID_ANGLE_UNIT ( ) );
#11018 = CYLINDRICAL_SURFACE ( 'NONE', #8903, 4.800000000000000711 ) ;
#11019 = ORIENTED_EDGE ( 'NONE', *, *, #20246, .T. ) ;
#11020 = ORIENTED_EDGE ( 'NONE', *, *, #17533, .F. ) ;
#11021 = EDGE_CURVE ( 'NONE', #17030, #26694, #17512, .T. ) ;
#11022 = AXIS2_PLACEMENT_3D ( 'NONE', #14885, #31465, #9492 ) ;
#11023 = MECHANICAL_DESIGN_GEOMETRIC_PRESENTATION_REPRESENTATION (  '', ( #14466 ), #7568 ) ;
#11024 = CARTESIAN_POINT ( 'NONE',  ( -10.00000000000000000, 0.000000000000000000, 0.000000000000000000 ) ) ;
#11025 = AXIS2_PLACEMENT_3D ( 'NONE', #13996, #8416, #33271 ) ;
#11026 = FACE_OUTER_BOUND ( 'NONE', #24713, .T. ) ;
#11027 = EDGE_CURVE ( 'NONE', #16212, #32593, #14823, .T. ) ;
#11028 = ORIENTED_EDGE ( 'NONE', *, *, #5891, .T. ) ;
#11029 = LINE ( 'NONE', #24535, #27944 ) ;
#11030 = ORIENTED_EDGE ( 'NONE', *, *, #524, .F. ) ;
#11031 =( REPRESENTATION_RELATIONSHIP ('NONE','NONE', #26607, #27563 ) REPRESENTATION_RELATIONSHIP_WITH_TRANSFORMATION ( #31454 )SHAPE_REPRESENTATION_RELATIONSHIP( ) );
#11032 = CARTESIAN_POINT ( 'NONE',  ( -35.50000000000000000, -112.9990795116828650, 0.8734249692896993711 ) ) ;
#11033 = CARTESIAN_POINT ( 'NONE',  ( 4.000000000000003553, 47.32430374665962347, -21.55018039121478424 ) ) ;
#11034 = CARTESIAN_POINT ( 'NONE',  ( -37.47347596530441649, -114.9754527089670262, 4.972274454178449155 ) ) ;
#11035 = FACE_OUTER_BOUND ( 'NONE', #14920, .T. ) ;
#11036 = EDGE_LOOP ( 'NONE', ( #29463, #9968, #227, #15399 ) ) ;
#11037 = CARTESIAN_POINT ( 'NONE',  ( -34.49999999999998579, -24.48076211353329157, 98.91941090707499029 ) ) ;
#11038 = CARTESIAN_POINT ( 'NONE',  ( -35.50000000000000000, -117.0140978167138854, 0.0002176474015578471800 ) ) ;
#11039 = VERTEX_POINT ( 'NONE', #1150 ) ;
#11040 = EDGE_LOOP ( 'NONE', ( #2644, #31547, #19899, #10314 ) ) ;
#11041 = CARTESIAN_POINT ( 'NONE',  ( -36.11231047232249125, -112.0245472910329880, 7.222274454178451819 ) ) ;
#11042 = EDGE_CURVE ( 'NONE', #12726, #4002, #12302, .T. ) ;
#11043 = DIRECTION ( 'NONE',  ( 0.000000000000000000, -0.3090169943749350723, -0.9510565162951576390 ) ) ;
#11044 = ORIENTED_EDGE ( 'NONE', *, *, #2523, .T. ) ;
#11045 = EDGE_LOOP ( 'NONE', ( #16751, #11341, #49, #15005 ) ) ;
#11046 = CARTESIAN_POINT ( 'NONE',  ( -34.50000000000000000, -115.0140978167143402, -0.6247823525984417259 ) ) ;
#11047 = LINE ( 'NONE', #20980, #31528 ) ;
#11048 = EDGE_CURVE ( 'NONE', #10551, #876, #30528, .T. ) ;
#11049 = VECTOR ( 'NONE', #277, 1000.000000000000000 ) ;
#11050 = CARTESIAN_POINT ( 'NONE',  ( 8.000000000000000000, 18.62763138773855687, 10.49404041845541968 ) ) ;
#11051 = DIRECTION ( 'NONE',  ( 0.000000000000000000, -0.5000000000000032196, 0.8660254037844368202 ) ) ;
#11052 = CARTESIAN_POINT ( 'NONE',  ( -35.50000000000000000, -113.9929510916434339, 12.50851088611648265 ) ) ;
#11053 = DIRECTION ( 'NONE',  ( 0.000000000000000000, 0.3681245526846787519, -0.9297764858882511252 ) ) ;
#11054 = EDGE_CURVE ( 'NONE', #22703, #32586, #26354, .T. ) ;
#11055 = DIRECTION ( 'NONE',  ( 0.000000000000000000, -6.987080667128811173E-15, 1.000000000000000000 ) ) ;
#11056 = EDGE_CURVE ( 'NONE', #28075, #1935, #16133, .T. ) ;
#11057 = CARTESIAN_POINT ( 'NONE',  ( -34.50000000000000000, -115.5178116849130276, -1.498529437126731034 ) ) ;
#11058 = CARTESIAN_POINT ( 'NONE',  ( -38.98797722933581866, -115.9929510916434481, 12.81430620224974959 ) ) ;
#11059 = DIRECTION ( 'NONE',  ( -1.000000000000000000, 0.000000000000000000, 0.000000000000000000 ) ) ;
#11060 = AXIS2_PLACEMENT_3D ( 'NONE', #16442, #22553, #3854 ) ;
#11061 = CARTESIAN_POINT ( 'NONE',  ( 8.000000000000000000, -18.62763138773852134, 2.494040418455287345 ) ) ;
#11062 = DIRECTION ( 'NONE',  ( 0.000000000000000000, 1.000000000000000000, 0.000000000000000000 ) ) ;
#11063 = EDGE_LOOP ( 'NONE', ( #669, #34277, #32430, #6604 ) ) ;
#11064 = CARTESIAN_POINT ( 'NONE',  ( -35.50000000000000711, -114.2598117360253696, 9.542047897280109936 ) ) ;
#11065 = DIRECTION ( 'NONE',  ( 0.000000000000000000, 0.000000000000000000, -1.000000000000000000 ) ) ;
#11066 = PRESENTATION_STYLE_ASSIGNMENT (( #79 ) ) ;
#11067 = DIRECTION ( 'NONE',  ( 0.000000000000000000, 0.000000000000000000, 1.000000000000000000 ) ) ;
#11068 = LINE ( 'NONE', #21679, #15341 ) ;
#11069 = EDGE_CURVE ( 'NONE', #17029, #17838, #45, .T. ) ;
#11070 = ORIENTED_EDGE ( 'NONE', *, *, #33422, .T. ) ;
#11071 = LINE ( 'NONE', #22040, #33740 ) ;
#11072 = DIRECTION ( 'NONE',  ( -0.000000000000000000, 0.000000000000000000, 1.000000000000000000 ) ) ;
#11073 = AXIS2_PLACEMENT_3D ( 'NONE', #14973, #1855, #1304 ) ;
#11074 = CARTESIAN_POINT ( 'NONE',  ( -37.49999999999999289, -11.52052244843579309, 115.1848168619253698 ) ) ;
#11075 = CARTESIAN_POINT ( 'NONE',  ( 8.000000000000000000, 14.18878633068160866, 6.236773481718133283 ) ) ;
#11076 = CONTEXT_DEPENDENT_SHAPE_REPRESENTATION ( #6232, #33948 ) ;
#11077 = AXIS2_PLACEMENT_3D ( 'NONE', #16118, #32342, #27136 ) ;
#11078 = CIRCLE ( 'NONE', #32917, 20.00000000000000711 ) ;
#11079 = CARTESIAN_POINT ( 'NONE',  ( 7.999999999999992895, 0.000000000000000000, 0.000000000000000000 ) ) ;
#11080 = DIRECTION ( 'NONE',  ( 0.000000000000000000, 0.000000000000000000, 1.000000000000000000 ) ) ;
#11081 = ORIENTED_EDGE ( 'NONE', *, *, #10457, .F. ) ;
#11082 = CARTESIAN_POINT ( 'NONE',  ( 0.000000000000000000, -2.710505431213761085E-17, 38.00000000000000711 ) ) ;
#11083 = CARTESIAN_POINT ( 'NONE',  ( 5.400000000000071410, 0.9999999999999662492, 45.00000000000000711 ) ) ;
#11084 = ORIENTED_EDGE ( 'NONE', *, *, #7098, .T. ) ;
#11085 = CARTESIAN_POINT ( 'NONE',  ( -37.97545270896702618, -114.4734759653044023, 4.652725545821551734 ) ) ;
#11086 = EDGE_LOOP ( 'NONE', ( #32418, #2466, #31523, #10874 ) ) ;
#11087 = EDGE_CURVE ( 'NONE', #8762, #4534, #14418, .T. ) ;
#11089 = VERTEX_POINT ( 'NONE', #20918 ) ;
#11088 = AXIS2_PLACEMENT_3D ( 'NONE', #20671, #31667, #26463 ) ;
#11090 = ORIENTED_EDGE ( 'NONE', *, *, #28887, .T. ) ;
#11091 = CARTESIAN_POINT ( 'NONE',  ( -34.50000000000001421, -42.98076211353323828, 83.49999999999991473 ) ) ;
#11092 = EDGE_CURVE ( 'NONE', #26408, #16117, #32283, .T. ) ;
#11093 = EDGE_CURVE ( 'NONE', #26081, #14212, #23468, .T. ) ;
#11094 = DIRECTION ( 'NONE',  ( 0.000000000000000000, 0.000000000000000000, -1.000000000000000000 ) ) ;
#11095 = AXIS2_PLACEMENT_3D ( 'NONE', #8876, #24927, #33375 ) ;
#11096 = CARTESIAN_POINT ( 'NONE',  ( -35.50000000000000711, -114.0928965812550757, 9.511088712577292270 ) ) ;
#11097 = AXIS2_PLACEMENT_3D ( 'NONE', #28637, #7012, #9542 ) ;
#11098 = CARTESIAN_POINT ( 'NONE',  ( 0.000000000000000000, 3.872983346207416133, -1.000000000000000000 ) ) ;
#11099 = ADVANCED_FACE ( 'NONE', ( #1686 ), #1322, .T. ) ;
#11100 = AXIS2_PLACEMENT_3D ( 'NONE', #23881, #10725, #34869 ) ;
#11101 = DIRECTION ( 'NONE',  ( 0.000000000000000000, 0.000000000000000000, 1.000000000000000000 ) ) ;
#11102 = ADVANCED_FACE ( 'NONE', ( #9781, #23272 ), #4393, .T. ) ;
#11103 = CARTESIAN_POINT ( 'NONE',  ( 7.999999999999992895, 0.000000000000000000, 0.000000000000000000 ) ) ;
#11104 = LINE ( 'NONE', #5698, #32959 ) ;
#11105 = CARTESIAN_POINT ( 'NONE',  ( 0.000000000000000000, 0.000000000000000000, 0.000000000000000000 ) ) ;
#11106 = CARTESIAN_POINT ( 'NONE',  ( -38.99999693208653895, -115.9929510916434481, 12.62875129555797749 ) ) ;
#11107 = CARTESIAN_POINT ( 'NONE',  ( 8.000000000000007105, 11.27190672109271219, 0.3151488735049640111 ) ) ;
#11108 = DIRECTION ( 'NONE',  ( 0.000000000000000000, 0.000000000000000000, 1.000000000000000000 ) ) ;
#11109 = CIRCLE ( 'NONE', #12862, 15.49899999999998279 ) ;
#11110 = CYLINDRICAL_SURFACE ( 'NONE', #5556, 20.00000000000000711 ) ;
#11111 = DIRECTION ( 'NONE',  ( -1.000000000000000000, 0.000000000000000000, 0.000000000000000000 ) ) ;
#11112 = FACE_OUTER_BOUND ( 'NONE', #29860, .T. ) ;
#11113 = EDGE_LOOP ( 'NONE', ( #23557, #9154, #7866, #25493 ) ) ;
#11114 = CARTESIAN_POINT ( 'NONE',  ( -36.23083527818512550, -111.9754527089670404, 6.715225545821551734 ) ) ;
#11115 = CARTESIAN_POINT ( 'NONE',  ( 7.999999999999992895, -46.87740477351719193, 3.172455868805032608 ) ) ;
#11116 = DIRECTION ( 'NONE',  ( -1.000000000000000000, 0.000000000000000000, 0.000000000000000000 ) ) ;
#11117 = DIRECTION ( 'NONE',  ( 1.541976423090495387E-16, -1.000000000000000000, 0.000000000000000000 ) ) ;
#11118 = ORIENTED_EDGE ( 'NONE', *, *, #831, .F. ) ;
#11119 = ORIENTED_EDGE ( 'NONE', *, *, #33112, .T. ) ;
#11120 = VECTOR ( 'NONE', #5798, 1000.000000000000000 ) ;
#11121 = DIRECTION ( 'NONE',  ( 1.000000000000000000, -4.524158825347490025E-15, -1.169797080839617330E-15 ) ) ;
#11122 = CIRCLE ( 'NONE', #19180, 9.999999999999994671 ) ;
#11123 = DIRECTION ( 'NONE',  ( 0.000000000000000000, 0.000000000000000000, 1.000000000000000000 ) ) ;
#11124 = ORIENTED_EDGE ( 'NONE', *, *, #2462, .F. ) ;
#11125 = EDGE_LOOP ( 'NONE', ( #22611, #18583, #26906, #3197 ) ) ;
#11126 = EDGE_CURVE ( 'NONE', #26553, #10239, #12119, .T. ) ;
#11127 = EDGE_CURVE ( 'NONE', #3384, #4138, #13294, .T. ) ;
#11128 = DIRECTION ( 'NONE',  ( 1.000000000000000000, 0.000000000000000000, -0.000000000000000000 ) ) ;
#11129 = CARTESIAN_POINT ( 'NONE',  ( 4.000000000000003553, 51.85248208264525260, -3.914090171285633524 ) ) ;
#11130 =( NAMED_UNIT ( * ) PLANE_ANGLE_UNIT ( ) SI_UNIT ( $, .RADIAN. ) );
#11131 = DIRECTION ( 'NONE',  ( 0.000000000000000000, -0.6573494133204068612, 0.7535859266250379829 ) ) ;
#11132 = ORIENTED_EDGE ( 'NONE', *, *, #11048, .F. ) ;
#11133 = ORIENTED_EDGE ( 'NONE', *, *, #22650, .T. ) ;
#11134 = AXIS2_PLACEMENT_3D ( 'NONE', #1226, #6088, #28592 ) ;
#11135 = AXIS2_PLACEMENT_3D ( 'NONE', #10700, #2613, #8336 ) ;
#11136 = DIRECTION ( 'NONE',  ( 9.178431089824344374E-17, -6.938893903907203726E-17, -1.000000000000000000 ) ) ;
#11137 = DIRECTION ( 'NONE',  ( 0.000000000000000000, 0.000000000000000000, 1.000000000000000000 ) ) ;
#11138 = ORIENTED_EDGE ( 'NONE', *, *, #463, .F. ) ;
#11139 = CARTESIAN_POINT ( 'NONE',  ( 8.000000000000007105, -9.604183132802312173, -5.908880290975638161 ) ) ;
#11140 = CARTESIAN_POINT ( 'NONE',  ( -34.50000000000000000, -114.1807644833817648, -1.624782352598427959 ) ) ;
#11141 = AXIS2_PLACEMENT_3D ( 'NONE', #20693, #28997, #23049 ) ;
#11142 = CARTESIAN_POINT ( 'NONE',  ( -36.50000000000011369, -114.9929510916434339, 14.11852480586264846 ) ) ;
#11143 = CIRCLE ( 'NONE', #23212, 8.000000000000001776 ) ;
#11144 = CARTESIAN_POINT ( 'NONE',  ( -38.00000068757622529, -114.9929510916434339, 12.61439929482944855 ) ) ;
#11145 = DIRECTION ( 'NONE',  ( 1.000000000000000000, -1.110223024625156540E-16, 0.000000000000000000 ) ) ;
#11146 = CARTESIAN_POINT ( 'NONE',  ( -34.50000306791346816, -114.9929510916434339, 12.62875129555796150 ) ) ;
#11147 = DIRECTION ( 'NONE',  ( 1.000000000000000000, -0.000000000000000000, -0.000000000000000000 ) ) ;
#11148 = DIRECTION ( 'NONE',  ( 0.000000000000000000, 0.000000000000000000, 1.000000000000000000 ) ) ;
#11149 = DIRECTION ( 'NONE',  ( -1.000000000000000000, 0.000000000000000000, 0.000000000000000000 ) ) ;
#11150 = DIRECTION ( 'NONE',  ( -1.000000000000000000, 0.000000000000000000, 0.000000000000000000 ) ) ;
#11151 = DIRECTION ( 'NONE',  ( 0.000000000000000000, 0.000000000000000000, 1.000000000000000000 ) ) ;
#11152 = ORIENTED_EDGE ( 'NONE', *, *, #22212, .T. ) ;
#11153 = CARTESIAN_POINT ( 'NONE',  ( 8.000000000000000000, 1.693188892523948885, -15.40623615209870323 ) ) ;
#11154 = ORIENTED_EDGE ( 'NONE', *, *, #1002, .F. ) ;
#11155 = CARTESIAN_POINT ( 'NONE',  ( -39.07941549657748936, -111.8367748094582055, 3.941024454178448710 ) ) ;
#11156 = CARTESIAN_POINT ( 'NONE',  ( 8.000000000000000000, 16.71027810728552154, -2.620268201066000113 ) ) ;
#11157 = ORIENTED_EDGE ( 'NONE', *, *, #7739, .T. ) ;
#11158 = VERTEX_POINT ( 'NONE', #26538 ) ;
#11159 = LINE ( 'NONE', #35313, #15942 ) ;
#11160 = CARTESIAN_POINT ( 'NONE',  ( 0.000000000000000000, 0.000000000000000000, -32.00000000000000000 ) ) ;
#11161 = ORIENTED_EDGE ( 'NONE', *, *, #400, .F. ) ;
#11162 = CARTESIAN_POINT ( 'NONE',  ( -34.02454729103298092, -115.3019030900506294, 6.097274454178449155 ) ) ;
#11163 = CARTESIAN_POINT ( 'NONE',  ( 46.00000000000000000, 0.000000000000000000, 0.000000000000000000 ) ) ;
#11164 = AXIS2_PLACEMENT_3D ( 'NONE', #172, #531, #25558 ) ;
#11165 = ADVANCED_FACE ( 'NONE', ( #4582 ), #4221, .F. ) ;
#11166 = FACE_OUTER_BOUND ( 'NONE', #17342, .T. ) ;
#11167 = AXIS2_PLACEMENT_3D ( 'NONE', #7390, #28074, #11151 ) ;
#11168 = VERTEX_POINT ( 'NONE', #9957 ) ;
#11169 = ORIENTED_EDGE ( 'NONE', *, *, #18934, .T. ) ;
#11170 = DIRECTION ( 'NONE',  ( -1.000000000000000000, 0.000000000000000000, -0.000000000000000000 ) ) ;
#11171 = CARTESIAN_POINT ( 'NONE',  ( 0.000000000000000000, -2.710505431213761085E-17, 54.99999999999999289 ) ) ;
#11172 = VERTEX_POINT ( 'NONE', #12670 ) ;
#11173 = ORIENTED_EDGE ( 'NONE', *, *, #16267, .T. ) ;
#11174 = CARTESIAN_POINT ( 'NONE',  ( -35.50000000000000000, -112.8230659962028994, 2.866612799894348029 ) ) ;
#11175 = ADVANCED_FACE ( 'NONE', ( #25994 ), #23650, .T. ) ;
#11176 = CARTESIAN_POINT ( 'NONE',  ( 0.000000000000000000, 0.000000000000000000, 0.000000000000000000 ) ) ;
#11177 = ORIENTED_EDGE ( 'NONE', *, *, #23861, .F. ) ;
#11178 = CARTESIAN_POINT ( 'NONE',  ( -36.00585935943767169, -114.9929510916434339, 13.11852578240983291 ) ) ;
#11179 = CARTESIAN_POINT ( 'NONE',  ( -34.57658136524561598, -113.9929510916434339, 13.10177712753338675 ) ) ;
#11180 = DIRECTION ( 'NONE',  ( -1.000000000000000000, -1.836970198721029934E-16, -0.000000000000000000 ) ) ;
#11181 = DIRECTION ( 'NONE',  ( -1.783119874454246424E-31, -1.187911941725854497E-31, 1.000000000000000000 ) ) ;
#11182 = CARTESIAN_POINT ( 'NONE',  ( -34.50000000000000000, -113.9929510916434197, 10.50625754673586876 ) ) ;
#11183 = CARTESIAN_POINT ( 'NONE',  ( -38.81062062679291103, -114.9929510916434339, 13.37409560816442067 ) ) ;
#11184 = CARTESIAN_POINT ( 'NONE',  ( -38.00000000000000711, -115.9929510916434481, 11.21034663311206181 ) ) ;
#11185 = CARTESIAN_POINT ( 'NONE',  ( 0.000000000000000000, 2.494040418455619523, -18.62763138773847871 ) ) ;
#11187 = AXIS2_PLACEMENT_3D ( 'NONE', #1734, #10195, #26950 ) ;
#11186 = CARTESIAN_POINT ( 'NONE',  ( 0.9999999999999870104, -5.408326913195881325, -0.7999999999999951594 ) ) ;
#11188 = AXIS2_PLACEMENT_3D ( 'NONE', #861, #15425, #6978 ) ;
#11189 = ORIENTED_EDGE ( 'NONE', *, *, #25405, .F. ) ;
#11190 = EDGE_LOOP ( 'NONE', ( #17262, #1740, #15110, #19552 ) ) ;
#11191 = LINE ( 'NONE', #8830, #18954 ) ;
#11192 = DIRECTION ( 'NONE',  ( 1.000000000000000000, 1.734723475976807094E-16, 0.000000000000000000 ) ) ;
#11193 = AXIS2_PLACEMENT_3D ( 'NONE', #13686, #5757, #21948 ) ;
#11194 = VERTEX_POINT ( 'NONE', #24015 ) ;
#11195 = DIRECTION ( 'NONE',  ( -1.000000000000000000, 0.000000000000000000, 0.000000000000000000 ) ) ;
#11196 = VERTEX_POINT ( 'NONE', #18048 ) ;
#11197 = CARTESIAN_POINT ( 'NONE',  ( -35.50000000000000000, -113.0140978167137860, 0.8752176474016654106 ) ) ;
#11198 = CARTESIAN_POINT ( 'NONE',  ( -4.121423858225413461, -12.61643262889540473, -1.200000000000006617 ) ) ;
#11199 = CARTESIAN_POINT ( 'NONE',  ( -35.02454729103298803, -114.8876895276775087, 6.097274454178449155 ) ) ;
#11200 = DIRECTION ( 'NONE',  ( -1.000000000000000000, 0.000000000000000000, -0.000000000000000000 ) ) ;
#11201 = ORIENTED_EDGE ( 'NONE', *, *, #3391, .F. ) ;
#11202 =( LENGTH_UNIT ( ) NAMED_UNIT ( * ) SI_UNIT ( .MILLI., .METRE. ) );
#11203 = EDGE_CURVE ( 'NONE', #24596, #17756, #27093, .T. ) ;
#11204 = CARTESIAN_POINT ( 'NONE',  ( -35.50000000000000711, -112.7765286249690035, 1.847058736912741583 ) ) ;
#11205 = ORIENTED_EDGE ( 'NONE', *, *, #18232, .T. ) ;
#11206 = ORIENTED_EDGE ( 'NONE', *, *, #28162, .T. ) ;
#11207 = EDGE_CURVE ( 'NONE', #34510, #13434, #14981, .T. ) ;
#11208 = CARTESIAN_POINT ( 'NONE',  ( -37.76916472181487450, -111.9754527089670404, 8.534774454178448266 ) ) ;
#11209 = CARTESIAN_POINT ( 'NONE',  ( 7.999999999999992895, 27.79676263918241119, -37.88001506494740056 ) ) ;
#11210 = ORIENTED_EDGE ( 'NONE', *, *, #17748, .F. ) ;
#11211 = ORIENTED_EDGE ( 'NONE', *, *, #9124, .T. ) ;
#11212 = CARTESIAN_POINT ( 'NONE',  ( -34.50000000000000000, -113.8159288351371714, 1.978028123174813802 ) ) ;
#11213 = DIRECTION ( 'NONE',  ( 0.000000000000000000, 0.8660254037844398178, -0.4999999999999977796 ) ) ;
#11214 = CIRCLE ( 'NONE', #31336, 17.49900000000002720 ) ;
#11215 = CIRCLE ( 'NONE', #5494, 6.000000000000005329 ) ;
#11216 = EDGE_CURVE ( 'NONE', #7646, #3309, #20138, .T. ) ;
#11217 = PRODUCT_DEFINITION_CONTEXT ( 'detailed design', #18159, 'design' ) ;
#11218 = CARTESIAN_POINT ( 'NONE',  ( -3.799999999999999822, 4.382607293638566128E-16, 45.10000000000000142 ) ) ;
#11219 = EDGE_CURVE ( 'NONE', #5854, #908, #17267, .T. ) ;
#11220 = AXIS2_PLACEMENT_3D ( 'NONE', #34910, #10235, #13126 ) ;
#11221 = ADVANCED_FACE ( 'NONE', ( #2587 ), #30297, .T. ) ;
#11222 = AXIS2_PLACEMENT_3D ( 'NONE', #6249, #28575, #22797 ) ;
#11223 = CARTESIAN_POINT ( 'NONE',  ( -35.50000000000000000, -113.9929510916435049, 10.50625754673586876 ) ) ;
#11224 = PLANE ( 'NONE',  #5220 ) ;
#11225 = DIRECTION ( 'NONE',  ( 0.000000000000000000, -0.6845471059286791782, -0.7289686274214204342 ) ) ;
#11226 = CARTESIAN_POINT ( 'NONE',  ( -34.50000000000000000, -111.6790780953339066, 2.383953864837686343 ) ) ;
#11227 = CARTESIAN_POINT ( 'NONE',  ( -37.56132887387857267, -115.9929510916434481, 14.11732072679899197 ) ) ;
#11228 = CIRCLE ( 'NONE', #31352, 15.49899999999998279 ) ;
#11229 = FACE_OUTER_BOUND ( 'NONE', #13858, .T. ) ;
#11230 = PLANE ( 'NONE',  #34162 ) ;
#11231 = VERTEX_POINT ( 'NONE', #19475 ) ;
#11232 = CARTESIAN_POINT ( 'NONE',  ( -35.50000000000000711, -114.4026847875275337, 9.592046023459676718 ) ) ;
#11233 = CARTESIAN_POINT ( 'NONE',  ( 0.000000000000000000, 3.872983346207429900, 1.000000000000003109 ) ) ;
#11234 = CARTESIAN_POINT ( 'NONE',  ( 0.000000000000000000, 0.000000000000000000, -0.7999999999999951594 ) ) ;
#11235 = DIRECTION ( 'NONE',  ( 0.000000000000000000, 0.000000000000000000, 1.000000000000000000 ) ) ;
#11236 = EDGE_CURVE ( 'NONE', #20895, #6291, #8666, .T. ) ;
#11237 = VERTEX_POINT ( 'NONE', #19116 ) ;
#11238 = LINE ( 'NONE', #3860, #6496 ) ;
#11239 = CARTESIAN_POINT ( 'NONE',  ( 8.000000000000000000, -16.94522934049206597, -8.128228055639052485 ) ) ;
#11240 = AXIS2_PLACEMENT_3D ( 'NONE', #26939, #23866, #4793 ) ;
#11241 = FACE_OUTER_BOUND ( 'NONE', #30176, .T. ) ;
#11242 = DIRECTION ( 'NONE',  ( 0.000000000000000000, 0.000000000000000000, -1.000000000000000000 ) ) ;
#11243 = CARTESIAN_POINT ( 'NONE',  ( 0.000000000000000000, -2.710505431213761085E-17, -46.00000000000000000 ) ) ;
#11244 = DIRECTION ( 'NONE',  ( 0.000000000000000000, 0.000000000000000000, 1.000000000000000000 ) ) ;
#11245 = AXIS2_PLACEMENT_3D ( 'NONE', #32687, #21868, #2453 ) ;
#11246 = ORIENTED_EDGE ( 'NONE', *, *, #28248, .T. ) ;
#11247 = ADVANCED_FACE ( 'NONE', ( #2242 ), #32815, .T. ) ;
#11248 = DIRECTION ( 'NONE',  ( 0.000000000000000000, 0.000000000000000000, 1.000000000000000000 ) ) ;
#11249 = LINE ( 'NONE', #33222, #28359 ) ;
#11250 = ORIENTED_EDGE ( 'NONE', *, *, #17528, .F. ) ;
#11251 = EDGE_CURVE ( 'NONE', #192, #31803, #31092, .T. ) ;
#11252 = CARTESIAN_POINT ( 'NONE',  ( -37.47347596530441649, -113.0245472910329880, 5.027725545821551734 ) ) ;
#11253 = EDGE_CURVE ( 'NONE', #30036, #17467, #28802, .T. ) ;
#11254 = EDGE_LOOP ( 'NONE', ( #13848, #13986, #222, #19449 ) ) ;
#11255 = AXIS2_PLACEMENT_3D ( 'NONE', #2535, #8258, #30585 ) ;
#11256 = ORIENTED_EDGE ( 'NONE', *, *, #9857, .F. ) ;
#11257 = ORIENTED_EDGE ( 'NONE', *, *, #28839, .F. ) ;
#11258 = FACE_OUTER_BOUND ( 'NONE', #16587, .T. ) ;
#11259 = EDGE_CURVE ( 'NONE', #29210, #18916, #27605, .T. ) ;
#11260 = CARTESIAN_POINT ( 'NONE',  ( -35.50000000000000711, -113.0106174888879877, 1.881901162060937827 ) ) ;
#11261 = EDGE_CURVE ( 'NONE', #33467, #4873, #7964, .T. ) ;
#11262 = DIRECTION ( 'NONE',  ( -1.000000000000000000, 0.000000000000000000, 0.000000000000000000 ) ) ;
#11263 = AXIS2_PLACEMENT_3D ( 'NONE', #6716, #17696, #33551 ) ;
#11264 = CARTESIAN_POINT ( 'NONE',  ( 8.000000000000000000, 11.11653975335790179, 12.74840161668735661 ) ) ;
#11265 = DIRECTION ( 'NONE',  ( -1.000000000000000000, 0.000000000000000000, 0.000000000000000000 ) ) ;
#11266 = CYLINDRICAL_SURFACE ( 'NONE', #30927, 47.49900000000001654 ) ;
#11267 = AXIS2_PLACEMENT_3D ( 'NONE', #14444, #8694, #25454 ) ;
#11268 = AXIS2_PLACEMENT_3D ( 'NONE', #25012, #335, #16354 ) ;
#11269 = CARTESIAN_POINT ( 'NONE',  ( 0.000000000000000000, 26.17370628620710349, -39.63700417846138890 ) ) ;
#11270 = CARTESIAN_POINT ( 'NONE',  ( 8.000000000000000000, -14.18878633068163708, 6.236773481718040024 ) ) ;
#11271 = AXIS2_PLACEMENT_3D ( 'NONE', #1730, #25874, #31258 ) ;
#11272 = DIRECTION ( 'NONE',  ( 1.000000000000000000, -0.000000000000000000, -0.000000000000000000 ) ) ;
#11273 = CARTESIAN_POINT ( 'NONE',  ( -37.24999999999992184, -115.9929510916434481, 14.11852480586265024 ) ) ;
#11274 = LINE ( 'NONE', #2484, #20523 ) ;
#11275 = AXIS2_PLACEMENT_3D ( 'NONE', #20035, #31039, #6371 ) ;
#11276 = ADVANCED_FACE ( 'NONE', ( #35531 ), #2410, .T. ) ;
#11277 = CARTESIAN_POINT ( 'NONE',  ( 0.000000000000000000, -2.710505431213761085E-17, 29.09999999999999787 ) ) ;
#11278 = AXIS2_PLACEMENT_3D ( 'NONE', #4830, #15772, #31819 ) ;
#11279 = DIRECTION ( 'NONE',  ( 0.000000000000000000, 0.4999999999999929501, 0.8660254037844428154 ) ) ;
#11280 = DIRECTION ( 'NONE',  ( 0.000000000000000000, 0.000000000000000000, -1.000000000000000000 ) ) ;
#11281 = ADVANCED_FACE ( 'NONE', ( #24183 ), #30115, .T. ) ;
#11282 = DIRECTION ( 'NONE',  ( 1.000000000000000000, 1.734723475976807094E-16, 0.000000000000000000 ) ) ;
#11283 = CARTESIAN_POINT ( 'NONE',  ( 8.000000000000000000, -14.48509162075955281, -8.733917826871511636 ) ) ;
#11284 = EDGE_LOOP ( 'NONE', ( #27058, #22049, #25258, #24373 ) ) ;
#11285 = EDGE_CURVE ( 'NONE', #34584, #33861, #5453, .T. ) ;
#11286 = CARTESIAN_POINT ( 'NONE',  ( -37.05926240293131713, -112.0000000000000142, 9.621475545821551734 ) ) ;
#11287 = DIRECTION ( 'NONE',  ( -1.000000000000000000, -1.836970198721029934E-16, -0.000000000000000000 ) ) ;
#11288 = FACE_OUTER_BOUND ( 'NONE', #22352, .T. ) ;
#11289 = FACE_OUTER_BOUND ( 'NONE', #23835, .T. ) ;
#11290 = VERTEX_POINT ( 'NONE', #214 ) ;
#11291 = ORIENTED_EDGE ( 'NONE', *, *, #9207, .T. ) ;
#11293 = CARTESIAN_POINT ( 'NONE',  ( -21.15833593587365513, -16.18172400785637777, 71.02756813566458050 ) ) ;
#11292 = PRODUCT_DEFINITION_SHAPE ( 'NONE', 'NONE',  #35654 ) ;
#11294 = AXIS2_PLACEMENT_3D ( 'NONE', #23825, #1684, #29767 ) ;
#11295 = DIRECTION ( 'NONE',  ( 0.000000000000000000, 0.000000000000000000, -1.000000000000000000 ) ) ;
#11296 = ORIENTED_EDGE ( 'NONE', *, *, #17360, .F. ) ;
#11297 = EDGE_CURVE ( 'NONE', #15120, #32416, #2773, .T. ) ;
#11298 = VERTEX_POINT ( 'NONE', #10495 ) ;
#11299 = EDGE_CURVE ( 'NONE', #8148, #19482, #23639, .T. ) ;
#11300 = CIRCLE ( 'NONE', #4398, 47.49900000000000944 ) ;
#11301 = AXIS2_PLACEMENT_3D ( 'NONE', #19539, #14148, #2847 ) ;
#11302 = AXIS2_PLACEMENT_3D ( 'NONE', #31037, #28513, #34099 ) ;
#11303 = CARTESIAN_POINT ( 'NONE',  ( 0.000000000000000000, -7.162210897275381072, -51.50439529848838305 ) ) ;
#11304 = CYLINDRICAL_SURFACE ( 'NONE', #11381, 7.199999999999993960 ) ;
#11305 = AXIS2_PLACEMENT_3D ( 'NONE', #15304, #11912, #7036 ) ;
#11306 = PRODUCT_CONTEXT ( 'NONE', #8695, 'mechanical' ) ;
#11307 = CARTESIAN_POINT ( 'NONE',  ( -10.00000000000000000, 0.000000000000000000, 0.000000000000000000 ) ) ;
#11309 = VERTEX_POINT ( 'NONE', #21995 ) ;
#11308 = VECTOR ( 'NONE', #1949, 1000.000000000000000 ) ;
#11310 = VERTEX_POINT ( 'NONE', #32992 ) ;
#11311 = DIRECTION ( 'NONE',  ( -1.000000000000000000, 0.000000000000000000, 0.000000000000000000 ) ) ;
#11312 = LINE ( 'NONE', #33613, #10926 ) ;
#11313 = ORIENTED_EDGE ( 'NONE', *, *, #9962, .F. ) ;
#11314 = DIRECTION ( 'NONE',  ( 0.000000000000000000, 0.000000000000000000, -1.000000000000000000 ) ) ;
#11315 = CIRCLE ( 'NONE', #5595, 9.499000000000009436 ) ;
#11316 = CARTESIAN_POINT ( 'NONE',  ( -34.50000000000000000, -113.6807644833805995, -1.624782352598427959 ) ) ;
#11317 = CARTESIAN_POINT ( 'NONE',  ( -36.31249999999995026, -114.9929510916434339, 14.11852480586264846 ) ) ;
#11318 = AXIS2_PLACEMENT_3D ( 'NONE', #35262, #29197, #31872 ) ;
#11319 = CARTESIAN_POINT ( 'NONE',  ( -38.00000000000000711, -114.9929510916434339, 12.60752341388803721 ) ) ;
#11320 = CARTESIAN_POINT ( 'NONE',  ( 0.000000000000000000, 0.000000000000000000, 0.000000000000000000 ) ) ;
#11321 = CARTESIAN_POINT ( 'NONE',  ( -34.50000000000000000, -114.9929510916434339, 11.38636890470581164 ) ) ;
#11322 = CARTESIAN_POINT ( 'NONE',  ( -0.1085714285714300953, -3.798448662927791819, 0.000000000000000000 ) ) ;
#11323 = VECTOR ( 'NONE', #13252, 1000.000000000000000 ) ;
#11324 = EDGE_CURVE ( 'NONE', #24581, #21764, #2382, .T. ) ;
#11325 = CARTESIAN_POINT ( 'NONE',  ( 7.999999999999992895, 0.000000000000000000, 0.000000000000000000 ) ) ;
#11326 = DIRECTION ( 'NONE',  ( 0.000000000000000000, 0.9822872507286879440, 0.1873813145857286533 ) ) ;
#11327 = AXIS2_PLACEMENT_3D ( 'NONE', #17514, #23471, #26170 ) ;
#11328 = DIRECTION ( 'NONE',  ( 1.000000000000000000, 0.000000000000000000, 0.000000000000000000 ) ) ;
#11329 = DIRECTION ( 'NONE',  ( 0.000000000000000000, 0.000000000000000000, 1.000000000000000000 ) ) ;
#11330 = ADVANCED_FACE ( 'NONE', ( #4929 ), #8307, .T. ) ;
#11331 = ORIENTED_EDGE ( 'NONE', *, *, #11216, .T. ) ;
#11332 = AXIS2_PLACEMENT_3D ( 'NONE', #21373, #30032, #2853 ) ;
#11333 = CARTESIAN_POINT ( 'NONE',  ( 7.999999999999992895, -39.55064067543046491, -25.36340625197400200 ) ) ;
#11334 = ORIENTED_EDGE ( 'NONE', *, *, #16733, .T. ) ;
#11335 = COLOUR_RGB ( '', 0.66274510, 0.83137255, 0.94901961) ;
#11336 = CARTESIAN_POINT ( 'NONE',  ( -38.30190309005061522, -116.9754527089670546, 4.972274454178449155 ) ) ;
#11337 = AXIS2_PLACEMENT_3D ( 'NONE', #26504, #7572, #7744 ) ;
#11338 = DIRECTION ( 'NONE',  ( -1.000000000000000000, 0.000000000000000000, 0.000000000000000000 ) ) ;
#11339 = CARTESIAN_POINT ( 'NONE',  ( -35.50000000000000711, -115.9630435732166518, -0.9469505670456015434 ) ) ;
#11340 = ORIENTED_EDGE ( 'NONE', *, *, #32353, .F. ) ;
#11341 = ORIENTED_EDGE ( 'NONE', *, *, #31891, .T. ) ;
#11342 = DIRECTION ( 'NONE',  ( 0.000000000000000000, 0.000000000000000000, 1.000000000000000000 ) ) ;
#11343 = DIRECTION ( 'NONE',  ( 0.000000000000000000, 0.000000000000000000, -1.000000000000000000 ) ) ;
#11344 = ORIENTED_EDGE ( 'NONE', *, *, #11976, .T. ) ;
#11345 = AXIS2_PLACEMENT_3D ( 'NONE', #18623, #15915, #26932 ) ;
#11346 = CARTESIAN_POINT ( 'NONE',  ( 0.000000000000000000, 0.000000000000000000, 55.00000000000000000 ) ) ;
#11347 = AXIS2_PLACEMENT_3D ( 'NONE', #13574, #24741, #2079 ) ;
#11348 = LINE ( 'NONE', #33646, #25750 ) ;
#11349 = ORIENTED_EDGE ( 'NONE', *, *, #20539, .T. ) ;
#11350 = ORIENTED_EDGE ( 'NONE', *, *, #33214, .F. ) ;
#11351 = CARTESIAN_POINT ( 'NONE',  ( 4.000000000000003553, -3.975523202427916125, -13.42368113696675636 ) ) ;
#11352 = CIRCLE ( 'NONE', #5602, 20.00000000000000711 ) ;
#11353 = FACE_OUTER_BOUND ( 'NONE', #1373, .T. ) ;
#11354 = ORIENTED_EDGE ( 'NONE', *, *, #28766, .F. ) ;
#11355 = ORIENTED_EDGE ( 'NONE', *, *, #31244, .T. ) ;
#11356 = CARTESIAN_POINT ( 'NONE',  ( -34.50000000000000000, -114.9515981487115823, -2.624803185604625000 ) ) ;
#11357 = AXIS2_PLACEMENT_3D ( 'NONE', #12990, #26509, #27215 ) ;
#11358 = CIRCLE ( 'NONE', #26233, 47.49900000000001654 ) ;
#11359 = ORIENTED_EDGE ( 'NONE', *, *, #16074, .T. ) ;
#11360 = CIRCLE ( 'NONE', #14790, 6.000000000000005329 ) ;
#11361 = CARTESIAN_POINT ( 'NONE',  ( -35.56312645773537895, -114.9929510916434339, 12.87038173996308998 ) ) ;
#11362 = CARTESIAN_POINT ( 'NONE',  ( -34.50000000000000000, -113.9929510916434339, 12.59652202191340464 ) ) ;
#11363 = CYLINDRICAL_SURFACE ( 'NONE', #7923, 20.00000000000000355 ) ;
#11364 = DIRECTION ( 'NONE',  ( 0.000000000000000000, 0.2588190451025084160, 0.9659258262890716429 ) ) ;
#11365 = CARTESIAN_POINT ( 'NONE',  ( -34.50000000000000000, -113.9929510916434339, 12.50851088611648265 ) ) ;
#11366 = CARTESIAN_POINT ( 'NONE',  ( -38.42182118622945808, -114.9929510916434339, 13.81802396319329773 ) ) ;
#11367 = CARTESIAN_POINT ( 'NONE',  ( -35.50000000000000711, -114.9929510916434339, 10.94631322572069365 ) ) ;
#11368 = AXIS2_PLACEMENT_3D ( 'NONE', #3498, #3143, #6009 ) ;
#11369 = LINE ( 'NONE', #22335, #34301 ) ;
#11370 = LINE ( 'NONE', #22337, #22143 ) ;
#11371 = EDGE_CURVE ( 'NONE', #15707, #14196, #33977, .T. ) ;
#11372 = VECTOR ( 'NONE', #21803, 1000.000000000000000 ) ;
#11373 = VERTEX_POINT ( 'NONE', #30990 ) ;
#11374 = ORIENTED_EDGE ( 'NONE', *, *, #3107, .F. ) ;
#11375 = AXIS2_PLACEMENT_3D ( 'NONE', #22502, #195, #28277 ) ;
#11376 = DIRECTION ( 'NONE',  ( 1.000000000000000000, 0.000000000000000000, 0.000000000000000000 ) ) ;
#11377 = CARTESIAN_POINT ( 'NONE',  ( 8.000000000000000000, 15.46619997295644389, -1.007799283846741556 ) ) ;
#11378 = VECTOR ( 'NONE', #19017, 1000.000000000000000 ) ;
#11379 = AXIS2_PLACEMENT_3D ( 'NONE', #1968, #10426, #24455 ) ;
#11380 = ORIENTED_EDGE ( 'NONE', *, *, #22907, .T. ) ;
#11381 = AXIS2_PLACEMENT_3D ( 'NONE', #22273, #35447, #33267 ) ;
#11382 = FACE_OUTER_BOUND ( 'NONE', #486, .T. ) ;
#11383 = ORIENTED_EDGE ( 'NONE', *, *, #31451, .F. ) ;
#11384 = CARTESIAN_POINT ( 'NONE',  ( -35.50000000000000000, -114.9307644833806137, -0.6247823525984269599 ) ) ;
#11385 = DIRECTION ( 'NONE',  ( -1.000000000000000000, 0.000000000000000000, 0.000000000000000000 ) ) ;
#11386 = CARTESIAN_POINT ( 'NONE',  ( -37.76916472181487450, -111.9754527089670404, 2.534774454178448710 ) ) ;
#11387 = EDGE_CURVE ( 'NONE', #984, #11433, #10434, .T. ) ;
#11388 = AXIS2_PLACEMENT_3D ( 'NONE', #10047, #12936, #32198 ) ;
#11389 = CARTESIAN_POINT ( 'NONE',  ( 8.000000000000000000, 11.06713717293239441, 13.55483219355733837 ) ) ;
#11390 = EDGE_LOOP ( 'NONE', ( #28709, #11599, #22835, #7730 ) ) ;
#11391 = FACE_OUTER_BOUND ( 'NONE', #1668, .T. ) ;
#11392 = CARTESIAN_POINT ( 'NONE',  ( -35.50000000000000000, -116.9119893297194324, -1.269118781492768910 ) ) ;
#11393 = ORIENTED_EDGE ( 'NONE', *, *, #32404, .T. ) ;
#11394 = VERTEX_POINT ( 'NONE', #3287 ) ;
#11395 = CARTESIAN_POINT ( 'NONE',  ( -35.62769128460905677, -115.4561184093552413, 4.691024454178448266 ) ) ;
#11396 = DIRECTION ( 'NONE',  ( 0.000000000000000000, 0.000000000000000000, -1.000000000000000000 ) ) ;
#11397 = ORIENTED_EDGE ( 'NONE', *, *, #33945, .F. ) ;
#11398 = ORIENTED_EDGE ( 'NONE', *, *, #34979, .F. ) ;
#11399 = CARTESIAN_POINT ( 'NONE',  ( -34.50000000000000000, -112.0140900043112282, 0.8439677466545482121 ) ) ;
#11400 = DIRECTION ( 'NONE',  ( -1.000000000000000000, 0.000000000000000000, 0.000000000000000000 ) ) ;
#11401 = ORIENTED_EDGE ( 'NONE', *, *, #24224, .F. ) ;
#11402 = CARTESIAN_POINT ( 'NONE',  ( 7.999999999999992895, 0.000000000000000000, 0.000000000000000000 ) ) ;
#11403 = CARTESIAN_POINT ( 'NONE',  ( -35.50000000000000000, -113.9929510916434339, 12.26648026267477398 ) ) ;
#11404 = DIRECTION ( 'NONE',  ( 0.000000000000000000, 0.4999999999999929501, 0.8660254037844428154 ) ) ;
#11405 = CARTESIAN_POINT ( 'NONE',  ( 50.00000000000000000, 0.000000000000000000, 0.000000000000000000 ) ) ;
#11406 = AXIS2_PLACEMENT_3D ( 'NONE', #14331, #5887, #22606 ) ;
#11407 = CARTESIAN_POINT ( 'NONE',  ( -34.50000000000000000, -113.5133328644208746, 2.949007337991939259 ) ) ;
#11408 = CARTESIAN_POINT ( 'NONE',  ( -39.00000000000000000, -115.9929510916434481, 11.91443571948719615 ) ) ;
#11409 = DIRECTION ( 'NONE',  ( -1.000000000000000000, -0.000000000000000000, -0.000000000000000000 ) ) ;
#11410 = DIRECTION ( 'NONE',  ( 1.000000000000000000, 0.000000000000000000, -1.691777834109590845E-31 ) ) ;
#11411 = EDGE_CURVE ( 'NONE', #34524, #10671, #25786, .T. ) ;
#11412 = ADVANCED_FACE ( 'NONE', ( #564 ), #9380, .F. ) ;
#11413 = VERTEX_POINT ( 'NONE', #22692 ) ;
#11414 = CYLINDRICAL_SURFACE ( 'NONE', #29782, 4.000000000000000000 ) ;
#11415 = CARTESIAN_POINT ( 'NONE',  ( 4.000000000000003553, -49.25004636492376875, -16.68630974939810940 ) ) ;
#11416 = LINE ( 'NONE', #27811, #31768 ) ;
#11417 = ORIENTED_EDGE ( 'NONE', *, *, #16911, .F. ) ;
#11418 = CARTESIAN_POINT ( 'NONE',  ( -50.00000000000000000, -25.98076211353320275, 95.99999999999991473 ) ) ;
#11419 = CARTESIAN_POINT ( 'NONE',  ( 4.000000000000000000, 4.627536653468036720E-16, -55.00000000000000000 ) ) ;
#11420 = DIRECTION ( 'NONE',  ( -1.000000000000000000, 0.000000000000000000, -0.000000000000000000 ) ) ;
#11421 = DIRECTION ( 'NONE',  ( 0.000000000000000000, 0.000000000000000000, 1.000000000000000000 ) ) ;
#11422 = VECTOR ( 'NONE', #16468, 1000.000000000000000 ) ;
#11423 = ADVANCED_FACE ( 'NONE', ( #3817 ), #923, .T. ) ;
#11424 = DIRECTION ( 'NONE',  ( 1.000000000000000000, -5.339440136655842133E-16, -1.047965281155519420E-16 ) ) ;
#11425 = DIRECTION ( 'NONE',  ( 1.000000000000000000, 1.836970198721029934E-16, 0.000000000000000000 ) ) ;
#11426 = VERTEX_POINT ( 'NONE', #9200 ) ;
#11427 = AXIS2_PLACEMENT_3D ( 'NONE', #20178, #1664, #14796 ) ;
#11428 = CARTESIAN_POINT ( 'NONE',  ( 4.000000000000003553, 19.83898331853701080, -9.508666619816445120 ) ) ;
#11429 = CARTESIAN_POINT ( 'NONE',  ( 0.000000000000000000, 13.56094713063641599, -50.20060470671727870 ) ) ;
#11430 = CARTESIAN_POINT ( 'NONE',  ( 7.999999999999992895, -9.744342220503080298, -46.48873837489808380 ) ) ;
#11431 = ORIENTED_EDGE ( 'NONE', *, *, #20076, .T. ) ;
#11432 = CARTESIAN_POINT ( 'NONE',  ( -35.02454729103298803, -113.1123104723225197, 9.902725545821557063 ) ) ;
#11433 = VERTEX_POINT ( 'NONE', #5975 ) ;
#11434 = PRESENTATION_STYLE_ASSIGNMENT (( #26769 ) ) ;
#11435 = ORIENTED_EDGE ( 'NONE', *, *, #33739, .T. ) ;
#11436 = VERTEX_POINT ( 'NONE', #6150 ) ;
#11437 = DIRECTION ( 'NONE',  ( -1.000000000000000000, 0.000000000000000000, 0.000000000000000000 ) ) ;
#11438 = CARTESIAN_POINT ( 'NONE',  ( -35.50000000000000711, -116.0140978167138712, -0.3122823525984417259 ) ) ;
#11439 = EDGE_CURVE ( 'NONE', #23782, #10046, #1801, .T. ) ;
#11440 = DIRECTION ( 'NONE',  ( -1.047965281155519667E-16, -6.938893903907193865E-17, -1.000000000000000000 ) ) ;
#11441 = DIRECTION ( 'NONE',  ( 0.000000000000000000, 0.000000000000000000, 1.000000000000000000 ) ) ;
#11442 = DIRECTION ( 'NONE',  ( 0.000000000000000000, 0.000000000000000000, 1.000000000000000000 ) ) ;
#11443 = CYLINDRICAL_SURFACE ( 'NONE', #29816, 8.000000000000000000 ) ;
#11444 = CARTESIAN_POINT ( 'NONE',  ( -34.50000000000000000, -114.1189822439768449, 9.514224058074130852 ) ) ;
#11445 = DIRECTION ( 'NONE',  ( 0.000000000000000000, -1.000000000000000000, 0.000000000000000000 ) ) ;
#11446 = AXIS2_PLACEMENT_3D ( 'NONE', #11402, #16953, #16784 ) ;
#11447 = ADVANCED_FACE ( 'NONE', ( #30473 ), #20162, .T. ) ;
#11448 = EDGE_CURVE ( 'NONE', #892, #30005, #33998, .T. ) ;
#11449 = LINE ( 'NONE', #19365, #29531 ) ;
#11450 = EDGE_CURVE ( 'NONE', #584, #9372, #3464, .T. ) ;
#11451 = CARTESIAN_POINT ( 'NONE',  ( -35.50000000000000000, -114.1185248058629611, 8.507048908356933836 ) ) ;
#11452 = CARTESIAN_POINT ( 'NONE',  ( -35.50000000000000711, -112.0141059978162019, -0.6575071456984691309 ) ) ;
#11453 = DIRECTION ( 'NONE',  ( -1.734723475976806848E-16, -0.8660254037844410391, 0.4999999999999958367 ) ) ;
#11454 = CARTESIAN_POINT ( 'NONE',  ( 1.498621416870377088, 0.000000000000000000, 0.000000000000000000 ) ) ;
#11455 = DIRECTION ( 'NONE',  ( 1.836970198721029934E-16, -1.000000000000000000, 0.000000000000000000 ) ) ;
#11456 = LINE ( 'NONE', #32897, #5549 ) ;
#11457 = ORIENTED_EDGE ( 'NONE', *, *, #20666, .T. ) ;
#11458 = EDGE_CURVE ( 'NONE', #15970, #16062, #25390, .T. ) ;
#11459 = CARTESIAN_POINT ( 'NONE',  ( -34.97545270896703329, -114.7691647218148745, 7.090225545821550845 ) ) ;
#11460 = DIRECTION ( 'NONE',  ( 0.000000000000000000, 0.000000000000000000, 1.000000000000000000 ) ) ;
#11461 = DIRECTION ( 'NONE',  ( 0.000000000000000000, 0.000000000000000000, 1.000000000000000000 ) ) ;
#11462 = CARTESIAN_POINT ( 'NONE',  ( 8.000000000000000000, 3.968388925834817282, 21.63912866391138934 ) ) ;
#11463 = EDGE_CURVE ( 'NONE', #25236, #6112, #6972, .T. ) ;
#11464 = ORIENTED_EDGE ( 'NONE', *, *, #6859, .F. ) ;
#11465 = ORIENTED_EDGE ( 'NONE', *, *, #21473, .F. ) ;
#11466 = DIRECTION ( 'NONE',  ( 9.615983791445651082E-17, -6.938893903907203726E-17, -1.000000000000000000 ) ) ;
#11467 = DIRECTION ( 'NONE',  ( 0.000000000000000000, 0.5877852522924739143, -0.8090169943749468962 ) ) ;
#11468 = ORIENTED_EDGE ( 'NONE', *, *, #26688, .T. ) ;
#11469 = AXIS2_PLACEMENT_3D ( 'NONE', #7849, #18837, #15949 ) ;
#11470 = ORIENTED_EDGE ( 'NONE', *, *, #14972, .F. ) ;
#11471 = AXIS2_PLACEMENT_3D ( 'NONE', #9490, #3936, #31279 ) ;
#11472 = FACE_OUTER_BOUND ( 'NONE', #3964, .T. ) ;
#11473 = CARTESIAN_POINT ( 'NONE',  ( 30.00000000000000000, 14.30000000000001315, -3.000000000000002665 ) ) ;
#11474 = EDGE_CURVE ( 'NONE', #15158, #26182, #739, .T. ) ;
#11475 = CARTESIAN_POINT ( 'NONE',  ( 50.00005079999999680, 0.000000000000000000, 0.000000000000000000 ) ) ;
#11476 = ORIENTED_EDGE ( 'NONE', *, *, #21190, .F. ) ;
#11477 = VERTEX_POINT ( 'NONE', #22346 ) ;
#11478 = ADVANCED_FACE ( 'NONE', ( #11904 ), #2965, .T. ) ;
#11479 = DIRECTION ( 'NONE',  ( 1.000000000000000000, 0.000000000000000000, 0.000000000000000000 ) ) ;
#11480 = DIRECTION ( 'NONE',  ( 0.000000000000000000, 0.6845471059286899473, -0.7289686274214103312 ) ) ;
#11481 = EDGE_CURVE ( 'NONE', #3480, #4713, #11720, .T. ) ;
#11482 = ORIENTED_EDGE ( 'NONE', *, *, #14158, .F. ) ;
#11483 = FACE_OUTER_BOUND ( 'NONE', #26806, .T. ) ;
#11484 = CARTESIAN_POINT ( 'NONE',  ( -34.50000000000000000, -115.0140978167138712, -0.3122823525984416704 ) ) ;
#11485 = CARTESIAN_POINT ( 'NONE',  ( 7.999999999999992895, 45.78515115856044559, 12.64416602183680816 ) ) ;
#11486 = FACE_BOUND ( 'NONE', #21989, .T. ) ;
#11487 = CARTESIAN_POINT ( 'NONE',  ( -34.50000000000000000, -114.1185248058629611, 8.507048908356933836 ) ) ;
#11488 = EDGE_CURVE ( 'NONE', #2288, #17196, #31169, .T. ) ;
#11489 = AXIS2_PLACEMENT_3D ( 'NONE', #4245, #9272, #31943 ) ;
#11490 = CARTESIAN_POINT ( 'NONE',  ( 0.000000000000000000, 0.000000000000000000, -1.200000000000006617 ) ) ;
#11491 = CARTESIAN_POINT ( 'NONE',  ( 0.6000000000000035305, -12.74999999999999822, -1.200000000000006617 ) ) ;
#11492 = EDGE_CURVE ( 'NONE', #18961, #28703, #33340, .T. ) ;
#11493 = CARTESIAN_POINT ( 'NONE',  ( -36.99999999999989342, -114.9929510916434339, 14.11852480586264846 ) ) ;
#11494 = LINE ( 'NONE', #11322, #16465 ) ;
#11495 = PLANE ( 'NONE',  #14361 ) ;
#11496 = CIRCLE ( 'NONE', #25305, 52.00000000000000711 ) ;
#11497 = DIRECTION ( 'NONE',  ( -1.000000000000000000, 0.000000000000000000, 0.000000000000000000 ) ) ;
#11498 = DIRECTION ( 'NONE',  ( 1.000000000000000000, 0.000000000000000000, 0.000000000000000000 ) ) ;
#11499 = VERTEX_POINT ( 'NONE', #33874 ) ;
#11500 = CYLINDRICAL_SURFACE ( 'NONE', #11268, 7.199999999999993960 ) ;
#11501 = EDGE_LOOP ( 'NONE', ( #35233, #28614, #9117, #32742 ) ) ;
#11502 = CIRCLE ( 'NONE', #16081, 20.00000000000000355 ) ;
#11503 = CARTESIAN_POINT ( 'NONE',  ( 1.599999999999990319, 0.000000000000000000, 0.000000000000000000 ) ) ;
#11504 = CARTESIAN_POINT ( 'NONE',  ( -34.92058450342251064, -116.1632251905417945, 7.691024454178450043 ) ) ;
#11505 = AXIS2_PLACEMENT_3D ( 'NONE', #19168, #35397, #24070 ) ;
#11506 = CARTESIAN_POINT ( 'NONE',  ( -35.50000000000000711, -113.2224311500466030, -1.624782352598427959 ) ) ;
#11507 = EDGE_CURVE ( 'NONE', #4040, #8141, #29405, .T. ) ;
#11508 = EDGE_LOOP ( 'NONE', ( #12940, #13852, #10331, #34160 ) ) ;
#11509 = ORIENTED_EDGE ( 'NONE', *, *, #2075, .F. ) ;
#11510 = LINE ( 'NONE', #3771, #18856 ) ;
#11511 = DIRECTION ( 'NONE',  ( -1.000000000000000000, 0.000000000000000000, 0.000000000000000000 ) ) ;
#11512 = VERTEX_POINT ( 'NONE', #23425 ) ;
#11513 = DIRECTION ( 'NONE',  ( 0.000000000000000000, 0.000000000000000000, -1.000000000000000000 ) ) ;
#11514 = LINE ( 'NONE', #14211, #14807 ) ;
#11515 = EDGE_LOOP ( 'NONE', ( #8859, #21598, #29459, #8578 ) ) ;
#11516 = EDGE_LOOP ( 'NONE', ( #29734, #7685 ) ) ;
#11517 = DIRECTION ( 'NONE',  ( -1.000000000000000000, 0.000000000000000000, 0.000000000000000000 ) ) ;
#11518 = VECTOR ( 'NONE', #16072, 1000.000000000000000 ) ;
#11519 =( NAMED_UNIT ( * ) SI_UNIT ( $, .STERADIAN. ) SOLID_ANGLE_UNIT ( ) );
#11520 = ADVANCED_FACE ( 'NONE', ( #20699, #9561 ), #6675, .T. ) ;
#11521 = PLANE ( 'NONE',  #18467 ) ;
#11522 = ORIENTED_EDGE ( 'NONE', *, *, #7291, .F. ) ;
#11523 = EDGE_LOOP ( 'NONE', ( #33218, #2546, #2293, #21824 ) ) ;
#11524 = AXIS2_PLACEMENT_3D ( 'NONE', #20283, #34179, #6618 ) ;
#11525 = CARTESIAN_POINT ( 'NONE',  ( -35.50000000000000000, -111.0687598768285369, 1.355111303971038073 ) ) ;
#11526 = ADVANCED_FACE ( 'NONE', ( #4354 ), #31697, .T. ) ;
#11527 = EDGE_CURVE ( 'NONE', #2304, #30694, #17828, .T. ) ;
#11528 = CIRCLE ( 'NONE', #32225, 4.000000000000000000 ) ;
#11529 = AXIS2_PLACEMENT_3D ( 'NONE', #13866, #10824, #2904 ) ;
#11530 = ORIENTED_EDGE ( 'NONE', *, *, #32639, .T. ) ;
#11531 = VECTOR ( 'NONE', #11396, 1000.000000000000000 ) ;
#11532 = CARTESIAN_POINT ( 'NONE',  ( -35.50000000000000711, -114.9929510916434339, 11.91443571948719971 ) ) ;
#11533 = CARTESIAN_POINT ( 'NONE',  ( -34.50000000000000000, -114.1489256397697289, 9.518467544735724317 ) ) ;
#11534 = DIRECTION ( 'NONE',  ( -1.000000000000000000, -0.000000000000000000, 0.000000000000000000 ) ) ;
#11535 = EDGE_CURVE ( 'NONE', #13171, #14603, #1228, .T. ) ;
#11536 = LINE ( 'NONE', #9721, #4783 ) ;
#11537 = EDGE_CURVE ( 'NONE', #6545, #30873, #15300, .T. ) ;
#11538 = CARTESIAN_POINT ( 'NONE',  ( -34.51202277066418844, -113.9929510916434339, 12.81430620224972294 ) ) ;
#11539 = CARTESIAN_POINT ( 'NONE',  ( -39.00000206272865455, -114.9929510916434339, 12.61164896875035701 ) ) ;
#11540 = CARTESIAN_POINT ( 'NONE',  ( -35.50000000000000711, -114.1091535596544873, 9.513028657562415447 ) ) ;
#11541 = CARTESIAN_POINT ( 'NONE',  ( 8.000000000000000000, 0.000000000000000000, 0.000000000000000000 ) ) ;
#11542 = LINE ( 'NONE', #8654, #29616 ) ;
#11543 = EDGE_LOOP ( 'NONE', ( #17221, #96, #24374, #25839 ) ) ;
#11544 = EDGE_LOOP ( 'NONE', ( #14240, #34521, #5800, #980 ) ) ;
#11545 = CIRCLE ( 'NONE', #8657, 5.000000000000004441 ) ;
#11546 = CARTESIAN_POINT ( 'NONE',  ( 3.799999999999999822, -2.710505431213761085E-17, 38.00000000000000711 ) ) ;
#11547 = DIRECTION ( 'NONE',  ( -1.000000000000000000, 0.000000000000000000, 0.000000000000000000 ) ) ;
#11548 = ORIENTED_EDGE ( 'NONE', *, *, #13070, .F. ) ;
#11549 = DIRECTION ( 'NONE',  ( -1.000000000000000000, 0.000000000000000000, 0.000000000000000000 ) ) ;
#11550 = ORIENTED_EDGE ( 'NONE', *, *, #17150, .F. ) ;
#11551 = CARTESIAN_POINT ( 'NONE',  ( -35.50000000000000000, -113.0140978167138996, -0.6247823525984302906 ) ) ;
#11552 = DIRECTION ( 'NONE',  ( 0.000000000000000000, 0.000000000000000000, -1.000000000000000000 ) ) ;
#11553 = CARTESIAN_POINT ( 'NONE',  ( -37.99999999999998579, -113.9407375970686758, 8.253524454178448266 ) ) ;
#11554 = VERTEX_POINT ( 'NONE', #15480 ) ;
#11555 = AXIS2_PLACEMENT_3D ( 'NONE', #3437, #5943, #14385 ) ;
#11556 = PLANE ( 'NONE',  #10766 ) ;
#11557 = AXIS2_PLACEMENT_3D ( 'NONE', #10252, #32029, #7534 ) ;
#11558 = ORIENTED_EDGE ( 'NONE', *, *, #8625, .F. ) ;
#11559 = FACE_OUTER_BOUND ( 'NONE', #1749, .T. ) ;
#11560 = CARTESIAN_POINT ( 'NONE',  ( -35.50000000000000711, -112.7472371723319355, 1.839427296857320648 ) ) ;
#11561 = VERTEX_POINT ( 'NONE', #25954 ) ;
#11562 = ORIENTED_EDGE ( 'NONE', *, *, #29712, .T. ) ;
#11563 = LINE ( 'NONE', #22532, #4460 ) ;
#11564 =( NAMED_UNIT ( * ) SI_UNIT ( $, .STERADIAN. ) SOLID_ANGLE_UNIT ( ) );
#11565 = CARTESIAN_POINT ( 'NONE',  ( 7.999999999999992895, 0.000000000000000000, 0.000000000000000000 ) ) ;
#11566 = ORIENTED_EDGE ( 'NONE', *, *, #27965, .F. ) ;
#11567 = ORIENTED_EDGE ( 'NONE', *, *, #25536, .F. ) ;
#11568 = CARTESIAN_POINT ( 'NONE',  ( -34.50000000000000000, -112.0221129971568104, -0.7553032835231431319 ) ) ;
#11569 = FACE_OUTER_BOUND ( 'NONE', #31737, .T. ) ;
#11570 = EDGE_CURVE ( 'NONE', #19641, #29049, #9738, .T. ) ;
#11571 = ORIENTED_EDGE ( 'NONE', *, *, #25168, .F. ) ;
#11572 = ORIENTED_EDGE ( 'NONE', *, *, #11092, .T. ) ;
#11573 = CARTESIAN_POINT ( 'NONE',  ( 8.000000000000000000, 8.605879768205236147, 12.89022243466711615 ) ) ;
#11574 = CARTESIAN_POINT ( 'NONE',  ( -35.50000000000000000, -113.9929510916438460, 10.50625754673626133 ) ) ;
#11575 = CARTESIAN_POINT ( 'NONE',  ( -21.15833593587365513, -29.27980021920983944, 82.28589838486210795 ) ) ;
#11576 = DIRECTION ( 'NONE',  ( 0.000000000000000000, -0.8443279255020201823, 0.5358267949789886631 ) ) ;
#11577 = AXIS2_PLACEMENT_3D ( 'NONE', #27774, #28471, #16932 ) ;
#11578 = STYLED_ITEM ( 'NONE', ( #16606 ), #29257 ) ;
#11579 = CARTESIAN_POINT ( 'NONE',  ( -34.50000000000000000, -111.3577635893106361, 2.022004269840791402 ) ) ;
#11580 = CARTESIAN_POINT ( 'NONE',  ( -37.69578139638701941, -115.9929510916434481, 14.10650203519847778 ) ) ;
#11581 = DIRECTION ( 'NONE',  ( -1.000000000000000000, 0.000000000000000000, 0.000000000000000000 ) ) ;
#11582 = DIRECTION ( 'NONE',  ( -1.000000000000000000, 0.000000000000000000, 0.000000000000000000 ) ) ;
#11583 = DIRECTION ( 'NONE',  ( -1.000000000000000000, 0.000000000000000000, 0.000000000000000000 ) ) ;
#11584 = DIRECTION ( 'NONE',  ( 0.000000000000000000, 8.881784197001252323E-16, 1.000000000000000000 ) ) ;
#11585 = CARTESIAN_POINT ( 'NONE',  ( 7.999999999999992895, 51.19683565102457834, -9.104066087302935983 ) ) ;
#11586 = ORIENTED_EDGE ( 'NONE', *, *, #32309, .T. ) ;
#11587 = LINE ( 'NONE', #780, #19140 ) ;
#11588 = DIRECTION ( 'NONE',  ( 0.1305261922200566527, -0.9914448613738098270, -5.718426984394921662E-16 ) ) ;
#11589 = DIRECTION ( 'NONE',  ( 0.000000000000000000, 0.000000000000000000, 1.000000000000000000 ) ) ;
#11590 = DIRECTION ( 'NONE',  ( -1.000000000000000000, 0.000000000000000000, -0.000000000000000000 ) ) ;
#11591 = DIRECTION ( 'NONE',  ( -1.000000000000000000, 0.000000000000000000, 0.000000000000000000 ) ) ;
#11592 = DIRECTION ( 'NONE',  ( 0.000000000000000000, 0.5877852522924685852, 0.8090169943749507819 ) ) ;
#11593 = ORIENTED_EDGE ( 'NONE', *, *, #26784, .T. ) ;
#11594 = CYLINDRICAL_SURFACE ( 'NONE', #917, 47.49900000000001654 ) ;
#11595 = CARTESIAN_POINT ( 'NONE',  ( -46.00000000000000000, 0.000000000000000000, 70.00000000000000000 ) ) ;
#11596 = CYLINDRICAL_SURFACE ( 'NONE', #26056, 7.199999999999994849 ) ;
#11597 = EDGE_LOOP ( 'NONE', ( #14798, #9790, #33308, #24364 ) ) ;
#11598 = CARTESIAN_POINT ( 'NONE',  ( -37.35495115944176803, -115.0245472910329880, 5.965225545821550845 ) ) ;
#11599 = ORIENTED_EDGE ( 'NONE', *, *, #12102, .T. ) ;
#11600 = CIRCLE ( 'NONE', #15591, 7.999999999999992895 ) ;
#11601 =( NAMED_UNIT ( * ) SI_UNIT ( $, .STERADIAN. ) SOLID_ANGLE_UNIT ( ) );
#11602 = VERTEX_POINT ( 'NONE', #23785 ) ;
#11603 = ORIENTED_EDGE ( 'NONE', *, *, #6419, .T. ) ;
#11604 = PLANE ( 'NONE',  #20027 ) ;
#11605 = EDGE_CURVE ( 'NONE', #9760, #3460, #34594, .T. ) ;
#11606 = LINE ( 'NONE', #3699, #10283 ) ;
#11607 = DIRECTION ( 'NONE',  ( -1.000000000000000000, -0.000000000000000000, 0.000000000000000000 ) ) ;
#11608 = CARTESIAN_POINT ( 'NONE',  ( -35.50000000000000711, -114.9929296450195721, 10.49869535309826674 ) ) ;
#11609 = CARTESIAN_POINT ( 'NONE',  ( 8.000000000000000000, 0.000000000000000000, 0.000000000000000000 ) ) ;
#11610 = EDGE_CURVE ( 'NONE', #16063, #30657, #17315, .T. ) ;
#11611 = LINE ( 'NONE', #22584, #1046 ) ;
#11612 = CARTESIAN_POINT ( 'NONE',  ( -34.50000000000000000, -114.1712995509219724, 9.522174004479579068 ) ) ;
#11613 = DIRECTION ( 'NONE',  ( -1.000000000000000000, -0.000000000000000000, 0.000000000000000000 ) ) ;
#11614 = DIRECTION ( 'NONE',  ( 0.000000000000000000, 0.3090169943749477288, -0.9510565162951534202 ) ) ;
#11615 = CARTESIAN_POINT ( 'NONE',  ( -35.50000000000000000, -115.9915791193162420, 10.43066258751475139 ) ) ;
#11617 = CARTESIAN_POINT ( 'NONE',  ( -35.50000000000000711, -112.3995503592287690, -1.424448457485529618 ) ) ;
#11616 = CIRCLE ( 'NONE', #13363, 4.000000000000000000 ) ;
#11618 = DIRECTION ( 'NONE',  ( 0.000000000000000000, 1.000000000000000000, 3.469446951953614189E-15 ) ) ;
#11619 = CARTESIAN_POINT ( 'NONE',  ( 0.000000000000000000, -2.710505431213761085E-17, -30.90000000000000568 ) ) ;
#11620 = DIRECTION ( 'NONE',  ( 1.000000000000000000, 0.000000000000000000, 0.000000000000000000 ) ) ;
#11621 = LINE ( 'NONE', #33588, #28007 ) ;
#11622 = LINE ( 'NONE', #4090, #23558 ) ;
#11623 = VERTEX_POINT ( 'NONE', #23602 ) ;
#11624 = CARTESIAN_POINT ( 'NONE',  ( -37.76916472181486739, -116.0245472910329880, 7.465225545821551734 ) ) ;
#11625 = DIRECTION ( 'NONE',  ( -1.000000000000000000, 0.000000000000000000, 0.000000000000000000 ) ) ;
#11626 = DIRECTION ( 'NONE',  ( 0.000000000000000000, 0.000000000000000000, -1.000000000000000000 ) ) ;
#11627 = EDGE_CURVE ( 'NONE', #13488, #33428, #32274, .T. ) ;
#11628 = CARTESIAN_POINT ( 'NONE',  ( 8.000000000000000000, 16.59870953437680896, 3.253005020243904255 ) ) ;
#11629 = VERTEX_POINT ( 'NONE', #31877 ) ;
#11630 = AXIS2_PLACEMENT_3D ( 'NONE', #26568, #4253, #29268 ) ;
#11631 = ORIENTED_EDGE ( 'NONE', *, *, #19598, .F. ) ;
#11632 = DIRECTION ( 'NONE',  ( -1.783119874454246424E-31, -1.187911941725854497E-31, 1.000000000000000000 ) ) ;
#11633 = DIRECTION ( 'NONE',  ( -1.000000000000000000, 0.000000000000000000, 0.000000000000000000 ) ) ;
#11634 = ORIENTED_EDGE ( 'NONE', *, *, #27086, .T. ) ;
#11635 = ORIENTED_EDGE ( 'NONE', *, *, #12466, .T. ) ;
#11636 = EDGE_CURVE ( 'NONE', #7004, #17434, #4004, .T. ) ;
#11637 = LINE ( 'NONE', #22612, #2040 ) ;
#11638 = AXIS2_PLACEMENT_3D ( 'NONE', #35161, #10481, #35512 ) ;
#11639 = EDGE_CURVE ( 'NONE', #14247, #21046, #24241, .T. ) ;
#11640 = CARTESIAN_POINT ( 'NONE',  ( -90.00000000000002842, 0.000000000000000000, 6.938893903907228378E-15 ) ) ;
#11641 = CIRCLE ( 'NONE', #19674, 6.765000000000044977 ) ;
#11642 = APPLICATION_PROTOCOL_DEFINITION ( 'draft international standard', 'automotive_design', 1998, #9855 ) ;
#11643 = CARTESIAN_POINT ( 'NONE',  ( 4.000000000000003553, 0.6505223195682995341, 51.99593080916758936 ) ) ;
#11644 = VERTEX_POINT ( 'NONE', #1279 ) ;
#11645 = ORIENTED_EDGE ( 'NONE', *, *, #35025, .F. ) ;
#11646 = FACE_BOUND ( 'NONE', #33527, .T. ) ;
#11647 = ADVANCED_FACE ( 'NONE', ( #12265 ), #23239, .T. ) ;
#11648 = LINE ( 'NONE', #25354, #7467 ) ;
#11649 = VERTEX_POINT ( 'NONE', #33813 ) ;
#11650 = CARTESIAN_POINT ( 'NONE',  ( 8.000000000000000000, -1.693188892523641798, -15.40623615209873876 ) ) ;
#11651 = EDGE_CURVE ( 'NONE', #16526, #620, #3572, .T. ) ;
#11652 = CIRCLE ( 'NONE', #29491, 4.000000000000000000 ) ;
#11653 = CARTESIAN_POINT ( 'NONE',  ( -34.50000000000000000, -115.0140978167138712, -0.6247823525983134951 ) ) ;
#11654 = CARTESIAN_POINT ( 'NONE',  ( 7.999999999999992895, -45.78515115856053797, 12.64416602183649019 ) ) ;
#11655 = CARTESIAN_POINT ( 'NONE',  ( -10.00000000000000178, 0.000000000000000000, 0.000000000000000000 ) ) ;
#11656 = AXIS2_PLACEMENT_3D ( 'NONE', #4248, #9444, #23673 ) ;
#11657 = CARTESIAN_POINT ( 'NONE',  ( -39.00000000000000711, -114.9929510916434339, 12.53051367006571937 ) ) ;
#11658 = AXIS2_PLACEMENT_3D ( 'NONE', #6361, #33210, #6014 ) ;
#11659 = CARTESIAN_POINT ( 'NONE',  ( 7.999999999999992895, 47.49120266317496686, -0.8606222198176971538 ) ) ;
#11660 = CARTESIAN_POINT ( 'NONE',  ( 0.000000000000000000, -2.710505431213761085E-17, 38.90000000000000568 ) ) ;
#11661 = CARTESIAN_POINT ( 'NONE',  ( -38.99984940073101569, -114.9929510916434339, 12.64306614848957189 ) ) ;
#11662 = CARTESIAN_POINT ( 'NONE',  ( 7.999999999999992895, -46.87740477351719193, 3.172455868805032608 ) ) ;
#11663 = DIRECTION ( 'NONE',  ( 0.000000000000000000, 0.000000000000000000, 1.000000000000000000 ) ) ;
#11664 = CYLINDRICAL_SURFACE ( 'NONE', #24500, 15.49899999999998457 ) ;
#11665 = CARTESIAN_POINT ( 'NONE',  ( -36.49999999999999289, -9.059673409587547965, 113.4689433211305811 ) ) ;
#11666 = AXIS2_PLACEMENT_3D ( 'NONE', #29808, #24579, #2276 ) ;
#11667 = ORIENTED_EDGE ( 'NONE', *, *, #26633, .F. ) ;
#11668 = VECTOR ( 'NONE', #23406, 1000.000000000000000 ) ;
#11669 = CARTESIAN_POINT ( 'NONE',  ( 0.000000000000000000, 42.03146605346787368, 22.12489237027333289 ) ) ;
#11670 = ORIENTED_EDGE ( 'NONE', *, *, #11297, .F. ) ;
#11671 = AXIS2_PLACEMENT_3D ( 'NONE', #614, #27293, #22221 ) ;
#11672 = CARTESIAN_POINT ( 'NONE',  ( -39.99999999999999289, -113.9407375970686758, 5.253524454178449155 ) ) ;
#11673 = DIRECTION ( 'NONE',  ( 1.000000000000000000, 0.000000000000000000, 0.000000000000000000 ) ) ;
#11674 = EDGE_CURVE ( 'NONE', #542, #3462, #17402, .T. ) ;
#11675 = CARTESIAN_POINT ( 'NONE',  ( -35.50000000000000711, -113.0974311500471714, -1.624782352598427959 ) ) ;
#11676 = EDGE_LOOP ( 'NONE', ( #6846, #31793 ) ) ;
#11677 = ORIENTED_EDGE ( 'NONE', *, *, #27495, .T. ) ;
#11678 = LINE ( 'NONE', #22479, #32668 ) ;
#11679 = CARTESIAN_POINT ( 'NONE',  ( 7.999999999999992895, 0.000000000000000000, 0.000000000000000000 ) ) ;
#11680 = VERTEX_POINT ( 'NONE', #11485 ) ;
#11681 = AXIS2_PLACEMENT_3D ( 'NONE', #32740, #5560, #7709 ) ;
#11682 = EDGE_CURVE ( 'NONE', #4062, #21331, #23665, .T. ) ;
#11683 = CARTESIAN_POINT ( 'NONE',  ( 70.00000000000001421, -35.39471919948800149, 89.19850115919967948 ) ) ;
#11684 = VERTEX_POINT ( 'NONE', #11654 ) ;
#11685 = VERTEX_POINT ( 'NONE', #14352 ) ;
#11686 = EDGE_CURVE ( 'NONE', #24324, #5109, #6434, .T. ) ;
#11687 = CARTESIAN_POINT ( 'NONE',  ( -37.76916472181486739, -116.0245472910329880, 2.965225545821551290 ) ) ;
#11688 = EDGE_CURVE ( 'NONE', #30356, #28584, #8949, .T. ) ;
#11689 = CARTESIAN_POINT ( 'NONE',  ( 7.999999999999992895, -29.60891106212763191, -37.14118181634798788 ) ) ;
#11690 = ORIENTED_EDGE ( 'NONE', *, *, #20938, .F. ) ;
#11691 = ORIENTED_EDGE ( 'NONE', *, *, #23117, .T. ) ;
#11692 = CARTESIAN_POINT ( 'NONE',  ( -34.50000000000000000, -117.0140978167138854, -0.4685323525984310122 ) ) ;
#11693 = AXIS2_PLACEMENT_3D ( 'NONE', #14058, #22873, #19794 ) ;
#11694 = CIRCLE ( 'NONE', #30113, 9.499000000000000554 ) ;
#11695 = CIRCLE ( 'NONE', #18018, 15.49899999999998457 ) ;
#11696 = CARTESIAN_POINT ( 'NONE',  ( -9.999999999999994671, 0.000000000000000000, 0.000000000000000000 ) ) ;
#11697 = VERTEX_POINT ( 'NONE', #25534 ) ;
#11698 = CARTESIAN_POINT ( 'NONE',  ( -35.69272627125609176, -114.9929510916434339, 13.01835785830562209 ) ) ;
#11699 = EDGE_CURVE ( 'NONE', #32057, #9747, #17294, .T. ) ;
#11700 = CARTESIAN_POINT ( 'NONE',  ( -37.49023442168701337, -113.9929510916434339, 14.11852773550420359 ) ) ;
#11701 = CARTESIAN_POINT ( 'NONE',  ( 8.000000000000000000, 14.87816164169121080, -4.342730381189718436 ) ) ;
#11702 = CARTESIAN_POINT ( 'NONE',  ( 1.600000000000004086, -12.74999999999999822, -1.200000000000006617 ) ) ;
#11703 = CARTESIAN_POINT ( 'NONE',  ( -35.61121590948313553, -113.9929510916434339, 14.07058620477040733 ) ) ;
#11704 = FACE_OUTER_BOUND ( 'NONE', #7695, .T. ) ;
#11705 = CARTESIAN_POINT ( 'NONE',  ( -35.56312645773537895, -114.9929510916434339, 12.87038173996308998 ) ) ;
#11706 = AXIS2_PLACEMENT_3D ( 'NONE', #34353, #7150, #28768 ) ;
#11707 = DIRECTION ( 'NONE',  ( -1.000000000000000000, 0.000000000000000000, 0.000000000000000000 ) ) ;
#11708 = FACE_BOUND ( 'NONE', #34433, .T. ) ;
#11709 = ORIENTED_EDGE ( 'NONE', *, *, #26305, .F. ) ;
#11710 = ORIENTED_EDGE ( 'NONE', *, *, #31199, .F. ) ;
#11711 = CARTESIAN_POINT ( 'NONE',  ( 7.999999999999992895, -39.55064067543080597, 25.36340625197344778 ) ) ;
#11712 = DIRECTION ( 'NONE',  ( -1.000000000000000000, 0.000000000000000000, 0.000000000000000000 ) ) ;
#11713 = ADVANCED_FACE ( 'NONE', ( #20275 ), #849, .T. ) ;
#11714 = ORIENTED_EDGE ( 'NONE', *, *, #11639, .T. ) ;
#11715 = CARTESIAN_POINT ( 'NONE',  ( 0.000000000000000000, 0.000000000000000000, -43.60000000000000142 ) ) ;
#11716 = VERTEX_POINT ( 'NONE', #25896 ) ;
#11717 = CIRCLE ( 'NONE', #30164, 4.872650870659778199 ) ;
#11718 = AXIS2_PLACEMENT_3D ( 'NONE', #12515, #18801, #29802 ) ;
#11719 = CARTESIAN_POINT ( 'NONE',  ( -35.50000000000000000, -115.0140978167137860, -0.6247823525984395054 ) ) ;
#11720 = LINE ( 'NONE', #14064, #23056 ) ;
#11721 = EDGE_CURVE ( 'NONE', #12138, #26946, #26530, .T. ) ;
#11722 = CARTESIAN_POINT ( 'NONE',  ( -34.97545270896703329, -113.2308352781851539, 4.409774454178448266 ) ) ;
#11723 = ORIENTED_EDGE ( 'NONE', *, *, #18796, .T. ) ;
#11724 = CARTESIAN_POINT ( 'NONE',  ( -36.94073759706868287, -112.0000000000000142, 5.628524454178449155 ) ) ;
#11725 = ORIENTED_EDGE ( 'NONE', *, *, #7710, .T. ) ;
#11726 = DIRECTION ( 'NONE',  ( 1.000000000000000000, 0.000000000000000000, -0.000000000000000000 ) ) ;
#11727 = CARTESIAN_POINT ( 'NONE',  ( -35.50000000000000711, -113.6318576702834804, 1.956056246348823580 ) ) ;
#11728 = VERTEX_POINT ( 'NONE', #33618 ) ;
#11729 = EDGE_LOOP ( 'NONE', ( #30868, #32259, #17540, #31830 ) ) ;
#11730 = EDGE_CURVE ( 'NONE', #6546, #27973, #6085, .T. ) ;
#11731 = CARTESIAN_POINT ( 'NONE',  ( -37.05926240293131713, -115.9999999999999858, 4.878524454178449155 ) ) ;
#11732 = EDGE_CURVE ( 'NONE', #17296, #21628, #12743, .T. ) ;
#11733 = SHAPE_REPRESENTATION_RELATIONSHIP ( 'NONE' , 'NONE' ,  #22901, #29257 ) ;
#11734 = PLANE ( 'NONE',  #16422 ) ;
#11735 = ORIENTED_EDGE ( 'NONE', *, *, #12652, .F. ) ;
#11736 = EDGE_LOOP ( 'NONE', ( #11331, #8088 ) ) ;
#11737 = CARTESIAN_POINT ( 'NONE',  ( -34.50000000000000000, -112.0140978167138712, -0.1247823525984259746 ) ) ;
#11738 = CARTESIAN_POINT ( 'NONE',  ( -6.896599878636569869, -12.98179148322720167, -1.200000000000006617 ) ) ;
#11739 = EDGE_LOOP ( 'NONE', ( #20687, #12972, #14300, #25652 ) ) ;
#11740 = ORIENTED_EDGE ( 'NONE', *, *, #32747, .F. ) ;
#11741 = LINE ( 'NONE', #22188, #26991 ) ;
#11742 = AXIS2_PLACEMENT_3D ( 'NONE', #17603, #9696, #18145 ) ;
#11743 = CARTESIAN_POINT ( 'NONE',  ( -36.03906250000000000, -113.9929510916434339, 13.11852480586264846 ) ) ;
#11744 = AXIS2_PLACEMENT_3D ( 'NONE', #12071, #34583, #4536 ) ;
#11745 = FACE_OUTER_BOUND ( 'NONE', #21450, .T. ) ;
#11746 = CARTESIAN_POINT ( 'NONE',  ( 0.000000000000000000, -51.19683565102450729, 9.104066087303298360 ) ) ;
#11747 = CARTESIAN_POINT ( 'NONE',  ( -34.50000000000000000, -111.0140978167138570, 0.0002176474015659786963 ) ) ;
#11748 = CIRCLE ( 'NONE', #34857, 15.49900000000001121 ) ;
#11749 = CARTESIAN_POINT ( 'NONE',  ( -35.50000000000000000, -115.9929510916434481, 10.85830208992344303 ) ) ;
#11750 = UNCERTAINTY_MEASURE_WITH_UNIT (LENGTH_MEASURE( 1.000000000000000082E-05 ), #27484, 'distance_accuracy_value', 'NONE');
#11751 = DIRECTION ( 'NONE',  ( 0.000000000000000000, 0.000000000000000000, 1.000000000000000000 ) ) ;
#11752 = DIRECTION ( 'NONE',  ( 0.000000000000000000, -0.9048270524660235736, 0.4257792915650641663 ) ) ;
#11753 = DIRECTION ( 'NONE',  ( -0.000000000000000000, 0.000000000000000000, -1.000000000000000000 ) ) ;
#11754 = DIRECTION ( 'NONE',  ( -1.000000000000000000, 0.000000000000000000, 0.000000000000000000 ) ) ;
#11755 = CARTESIAN_POINT ( 'NONE',  ( 3.799999999999999822, 0.000000000000000000, 50.00000000000000000 ) ) ;
#11756 = EDGE_CURVE ( 'NONE', #3873, #22893, #21905, .T. ) ;
#11757 = ORIENTED_EDGE ( 'NONE', *, *, #20929, .F. ) ;
#11758 = CARTESIAN_POINT ( 'NONE',  ( 0.000000000000000000, 0.000000000000000000, -55.89999999999999858 ) ) ;
#11759 = CARTESIAN_POINT ( 'NONE',  ( -37.49999999999999289, -15.63316754279159326, 121.0048025873809792 ) ) ;
#11760 = EDGE_CURVE ( 'NONE', #13855, #22477, #25956, .T. ) ;
#11761 = FACE_OUTER_BOUND ( 'NONE', #8065, .T. ) ;
#11762 = CARTESIAN_POINT ( 'NONE',  ( 2.000000000000002220, 2.507828756375099332E-16, -4.725000000000016520 ) ) ;
#11763 = CONTEXT_DEPENDENT_SHAPE_REPRESENTATION ( #3941, #2974 ) ;
#11764 = DIRECTION ( 'NONE',  ( -1.174092375852890260E-15, 4.222049128630259891E-16, 1.000000000000000000 ) ) ;
#11765 = DIRECTION ( 'NONE',  ( -1.000000000000000000, 0.000000000000000000, 0.000000000000000000 ) ) ;
#11766 = ORIENTED_EDGE ( 'NONE', *, *, #29293, .T. ) ;
#11767 = VECTOR ( 'NONE', #12352, 1000.000000000000000 ) ;
#11768 = SURFACE_STYLE_USAGE ( .BOTH. , #612 ) ;
#11769 = CIRCLE ( 'NONE', #12943, 3.799999999999999822 ) ;
#11770 = CARTESIAN_POINT ( 'NONE',  ( -26.99999999999999289, 3.122849337825751800E-15, 0.000000000000000000 ) ) ;
#11771 = LINE ( 'NONE', #7260, #34120 ) ;
#11772 = ORIENTED_EDGE ( 'NONE', *, *, #26918, .F. ) ;
#11773 = ORIENTED_EDGE ( 'NONE', *, *, #20076, .F. ) ;
#11774 = CARTESIAN_POINT ( 'NONE',  ( -37.35495115944176803, -115.0245472910329880, 7.465225545821552622 ) ) ;
#11775 = ORIENTED_EDGE ( 'NONE', *, *, #961, .F. ) ;
#11776 = SHAPE_REPRESENTATION_RELATIONSHIP ( 'NONE' , 'NONE' ,  #1790, #17621 ) ;
#11777 = ORIENTED_EDGE ( 'NONE', *, *, #18109, .F. ) ;
#11778 = ORIENTED_EDGE ( 'NONE', *, *, #31008, .T. ) ;
#11779 = DIRECTION ( 'NONE',  ( -1.000000000000000000, 0.000000000000000000, 0.000000000000000000 ) ) ;
#11780 = CARTESIAN_POINT ( 'NONE',  ( -35.50000000000000711, -115.9821387493194891, -0.8839717462762166633 ) ) ;
#11781 = CYLINDRICAL_SURFACE ( 'NONE', #12798, 19.99999999999999645 ) ;
#11782 = AXIS2_PLACEMENT_3D ( 'NONE', #29228, #7951, #27057 ) ;
#11783 = CARTESIAN_POINT ( 'NONE',  ( -35.60016694755736921, -114.9929510916434339, 12.92579853460621209 ) ) ;
#11784 = CARTESIAN_POINT ( 'NONE',  ( 8.000000000000000000, 6.359167119270718871, -18.96209359615085788 ) ) ;
#11785 = DIRECTION ( 'NONE',  ( 1.000000000000000000, 1.734723475976807094E-16, 0.000000000000000000 ) ) ;
#11786 = CARTESIAN_POINT ( 'NONE',  ( -34.50000000000000000, -114.9929510916434339, 10.56126450660895699 ) ) ;
#11787 = CARTESIAN_POINT ( 'NONE',  ( 7.999999999999992895, 22.43957647427220081, -41.27978878573601662 ) ) ;
#11788 = VECTOR ( 'NONE', #32935, 1000.000000000000000 ) ;
#11789 = PRODUCT_DEFINITION_SHAPE ( 'NONE', 'NONE',  #5763 ) ;
#11790 = AXIS2_PLACEMENT_3D ( 'NONE', #10039, #29316, #32185 ) ;
#11791 = DIRECTION ( 'NONE',  ( 0.000000000000000000, 0.5000000000000062172, -0.8660254037844351549 ) ) ;
#11792 = ORIENTED_EDGE ( 'NONE', *, *, #15896, .F. ) ;
#11793 = CARTESIAN_POINT ( 'NONE',  ( -39.00000000000000000, -115.9929510916434481, 12.50851088611646311 ) ) ;
#11794 = DIRECTION ( 'NONE',  ( -1.000000000000000000, -0.000000000000000000, -0.000000000000000000 ) ) ;
#11795 = AXIS2_PLACEMENT_3D ( 'NONE', #16809, #17513, #3507 ) ;
#11796 = LINE ( 'NONE', #33582, #10743 ) ;
#11797 = CARTESIAN_POINT ( 'NONE',  ( 0.000000000000000000, -2.494040418455211849, -18.62763138773853200 ) ) ;
#11798 = CARTESIAN_POINT ( 'NONE',  ( 8.000000000000000000, -3.968388925834658743, -21.63912866391144263 ) ) ;
#11799 = AXIS2_PLACEMENT_3D ( 'NONE', #32292, #13749, #21835 ) ;
#11800 = EDGE_CURVE ( 'NONE', #35157, #24108, #15569, .T. ) ;
#11801 = FACE_OUTER_BOUND ( 'NONE', #16727, .T. ) ;
#11802 = CARTESIAN_POINT ( 'NONE',  ( 3.872983346207489852, 0.9999999999999522604, -44.50000000000000000 ) ) ;
#11803 = ORIENTED_EDGE ( 'NONE', *, *, #9303, .F. ) ;
#11804 = CARTESIAN_POINT ( 'NONE',  ( -37.47347596530441649, -113.0245472910329880, 6.527725545821552622 ) ) ;
#11805 = LINE ( 'NONE', #28208, #19824 ) ;
#11806 = CARTESIAN_POINT ( 'NONE',  ( 7.999999999999992895, -13.85708833599938217, -45.43276465116679930 ) ) ;
#11807 = EDGE_LOOP ( 'NONE', ( #33164, #4284, #31391, #32209 ) ) ;
#11808 = AXIS2_PLACEMENT_3D ( 'NONE', #35303, #9896, #10450 ) ;
#11809 = EDGE_LOOP ( 'NONE', ( #3815, #7616, #11891, #18548 ) ) ;
#11810 = CARTESIAN_POINT ( 'NONE',  ( 7.999999999999992895, -47.49120266317497396, 0.8606222198173640869 ) ) ;
#11811 = DIRECTION ( 'NONE',  ( -1.000000000000000000, 0.000000000000000000, 0.000000000000000000 ) ) ;
#11812 = EDGE_LOOP ( 'NONE', ( #4675, #28054, #2889, #24251 ) ) ;
#11813 = CARTESIAN_POINT ( 'NONE',  ( -39.99999999999999289, -114.0592624029313242, 4.746475545821549957 ) ) ;
#11814 = ADVANCED_FACE ( 'NONE', ( #6608 ), #24260, .T. ) ;
#11815 = ORIENTED_EDGE ( 'NONE', *, *, #24154, .T. ) ;
#11816 = DIRECTION ( 'NONE',  ( -1.000000000000000000, 5.339440136655843119E-16, 0.000000000000000000 ) ) ;
#11817 = AXIS2_PLACEMENT_3D ( 'NONE', #253, #16974, #30155 ) ;
#11818 = LINE ( 'NONE', #22798, #7399 ) ;
#11819 = SHAPE_DEFINITION_REPRESENTATION ( #872, #1790 ) ;
#11820 = VECTOR ( 'NONE', #23263, 1000.000000000000000 ) ;
#11821 = CARTESIAN_POINT ( 'NONE',  ( 3.799999999999999822, 4.653657836759942730E-16, -40.40000000000000568 ) ) ;
#11822 = EDGE_LOOP ( 'NONE', ( #4413, #20349, #34788, #4575 ) ) ;
#11823 = ORIENTED_EDGE ( 'NONE', *, *, #7975, .F. ) ;
#11824 = CIRCLE ( 'NONE', #6077, 17.49900000000001654 ) ;
#11825 = LINE ( 'NONE', #12366, #15615 ) ;
#11826 = DIRECTION ( 'NONE',  ( 0.000000000000000000, 0.5735764363510502672, -0.8191520442889889120 ) ) ;
#11827 = ORIENTED_EDGE ( 'NONE', *, *, #22973, .T. ) ;
#11828 = LINE ( 'NONE', #22808, #2740 ) ;
#11829 = AXIS2_PLACEMENT_3D ( 'NONE', #27477, #27291, #10723 ) ;
#11830 = AXIS2_PLACEMENT_3D ( 'NONE', #19927, #14893, #1234 ) ;
#11831 = CARTESIAN_POINT ( 'NONE',  ( -34.50000000000000000, -113.8474311500459777, -0.6247823525984269599 ) ) ;
#11832 = DIRECTION ( 'NONE',  ( -1.000000000000000000, 0.000000000000000000, 0.000000000000000000 ) ) ;
#11833 = CARTESIAN_POINT ( 'NONE',  ( -34.50000000000000000, -116.0140978167138712, 0.8752176474015622709 ) ) ;
#11834 = CARTESIAN_POINT ( 'NONE',  ( -34.50000000000000000, -114.2265172349312508, 8.519938377296172760 ) ) ;
#11835 = CARTESIAN_POINT ( 'NONE',  ( 50.00005079999998969, 9.714451465470119729E-14, 1.000000000000000888 ) ) ;
#11836 = CARTESIAN_POINT ( 'NONE',  ( -37.05926240293131713, -115.9999999999999858, 1.878524454178448710 ) ) ;
#11837 = CARTESIAN_POINT ( 'NONE',  ( -39.00000000000000711, -114.9929510916434339, 10.50625754673587231 ) ) ;
#11838 = DIRECTION ( 'NONE',  ( 1.000000000000000000, 0.000000000000000000, 0.000000000000000000 ) ) ;
#11839 = CARTESIAN_POINT ( 'NONE',  ( 0.000000000000000000, -21.80633394113452539, 2.912696353505745517 ) ) ;
#11840 = CARTESIAN_POINT ( 'NONE',  ( 0.000000000000000000, -2.710505431213761085E-17, 55.00000000000000000 ) ) ;
#11841 = FACE_OUTER_BOUND ( 'NONE', #20043, .T. ) ;
#11842 = ADVANCED_FACE ( 'NONE', ( #673 ), #20452, .F. ) ;
#11843 = AXIS2_PLACEMENT_3D ( 'NONE', #32452, #4927, #15872 ) ;
#11844 = ORIENTED_EDGE ( 'NONE', *, *, #30200, .F. ) ;
#11845 = EDGE_CURVE ( 'NONE', #2557, #33795, #14465, .T. ) ;
#11846 = CYLINDRICAL_SURFACE ( 'NONE', #25669, 7.199999999999993960 ) ;
#11847 = EDGE_LOOP ( 'NONE', ( #5929, #26121, #31442, #23776 ) ) ;
#11848 = CARTESIAN_POINT ( 'NONE',  ( -39.97545270896702618, -115.3019030900506152, 3.152725545821551734 ) ) ;
#11849 = AXIS2_PLACEMENT_3D ( 'NONE', #16918, #19275, #5623 ) ;
#11850 = CARTESIAN_POINT ( 'NONE',  ( 8.000000000000007105, 11.27190672109280811, -0.3151488735047974776 ) ) ;
#11851 = VECTOR ( 'NONE', #10230, 1000.000000000000000 ) ;
#11852 = CARTESIAN_POINT ( 'NONE',  ( -35.50000000000000711, -116.0124910254613297, -0.6902086197697608894 ) ) ;
#11853 = ORIENTED_EDGE ( 'NONE', *, *, #25078, .F. ) ;
#11854 = ORIENTED_EDGE ( 'NONE', *, *, #33776, .T. ) ;
#11855 = CIRCLE ( 'NONE', #29709, 6.000000000000005329 ) ;
#11856 = DIRECTION ( 'NONE',  ( -1.000000000000000000, 0.000000000000000000, 0.000000000000000000 ) ) ;
#11857 = CARTESIAN_POINT ( 'NONE',  ( -4.000000000000000000, 0.000000000000000000, 60.00000000000000000 ) ) ;
#11858 = ORIENTED_EDGE ( 'NONE', *, *, #26431, .F. ) ;
#11859 = EDGE_CURVE ( 'NONE', #6495, #27914, #30930, .T. ) ;
#11860 = VERTEX_POINT ( 'NONE', #34442 ) ;
#11861 = CIRCLE ( 'NONE', #14701, 17.49900000000000233 ) ;
#11862 = AXIS2_PLACEMENT_3D ( 'NONE', #29447, #26572, #6757 ) ;
#11863 = SHAPE_REPRESENTATION ( 'spur gear_iso_ISO - Spur gear 2M 18T 20PA 8FW ---S18A75H50L8.0S1', ( #21307 ), #1229 ) ;
#11864 = CARTESIAN_POINT ( 'NONE',  ( 0.000000000000000000, 0.000000000000000000, 55.00000000000000711 ) ) ;
#11865 = VERTEX_POINT ( 'NONE', #15318 ) ;
#11866 = ORIENTED_EDGE ( 'NONE', *, *, #2185, .F. ) ;
#11867 = CARTESIAN_POINT ( 'NONE',  ( -35.02454729103298092, -113.1123104723225055, 6.902725545821551734 ) ) ;
#11868 = CARTESIAN_POINT ( 'NONE',  ( 0.000000000000000000, 0.000000000000000000, 0.000000000000000000 ) ) ;
#11869 = CARTESIAN_POINT ( 'NONE',  ( -34.49999999999998579, -20.32009476567239048, 97.80456345124113682 ) ) ;
#11870 = VECTOR ( 'NONE', #17990, 1000.000000000000000 ) ;
#11871 = EDGE_LOOP ( 'NONE', ( #6588, #19200, #17019, #24811 ) ) ;
#11872 = ORIENTED_EDGE ( 'NONE', *, *, #20292, .F. ) ;
#11873 = CARTESIAN_POINT ( 'NONE',  ( -35.50000000000000000, -111.0397324434303101, -0.9506101647064429949 ) ) ;
#11874 = CYLINDRICAL_SURFACE ( 'NONE', #32735, 10.99999999999999289 ) ;
#11875 = ORIENTED_EDGE ( 'NONE', *, *, #20822, .F. ) ;
#11876 = CARTESIAN_POINT ( 'NONE',  ( -36.24999999999983658, -114.9929510916434339, 13.11852480586264669 ) ) ;
#11877 = ADVANCED_FACE ( 'NONE', ( #2220 ), #26871, .F. ) ;
#11878 = VECTOR ( 'NONE', #21107, 1000.000000000000000 ) ;
#11879 = CARTESIAN_POINT ( 'NONE',  ( -39.00000000000000000, -113.9929510916434339, 12.57451923796417681 ) ) ;
#11880 = CIRCLE ( 'NONE', #3267, 10.00000000000000000 ) ;
#11881 = CARTESIAN_POINT ( 'NONE',  ( 0.000000000000000000, 0.000000000000000000, 0.000000000000000000 ) ) ;
#11882 = FACE_OUTER_BOUND ( 'NONE', #15038, .T. ) ;
#11883 = CARTESIAN_POINT ( 'NONE',  ( -37.54906985245723661, -113.9929510916434339, 14.11777216781844757 ) ) ;
#11884 = FACE_OUTER_BOUND ( 'NONE', #8488, .T. ) ;
#11885 = CARTESIAN_POINT ( 'NONE',  ( -36.50000000000011369, -114.9929510916434339, 13.11852480586264669 ) ) ;
#11886 = CARTESIAN_POINT ( 'NONE',  ( 7.999999999999992895, -25.61928775981074935, 45.25098998563468911 ) ) ;
#11887 = EDGE_LOOP ( 'NONE', ( #4348, #16409, #14464, #3062 ) ) ;
#11888 = DIRECTION ( 'NONE',  ( -1.000000000000000000, 0.000000000000000000, 0.000000000000000000 ) ) ;
#11889 = CARTESIAN_POINT ( 'NONE',  ( 46.00000000000000000, 0.000000000000000000, 59.00000000000000000 ) ) ;
#11890 = EDGE_CURVE ( 'NONE', #580, #35153, #30570, .T. ) ;
#11891 = ORIENTED_EDGE ( 'NONE', *, *, #4438, .T. ) ;
#11892 = EDGE_CURVE ( 'NONE', #2418, #10666, #20893, .T. ) ;
#11893 = CARTESIAN_POINT ( 'NONE',  ( -35.87040530316090070, -114.9929510916434339, 13.10254527216545917 ) ) ;
#11894 = ORIENTED_EDGE ( 'NONE', *, *, #29552, .T. ) ;
#11895 = ADVANCED_FACE ( 'NONE', ( #15497 ), #29216, .T. ) ;
#11896 = CARTESIAN_POINT ( 'NONE',  ( 7.999999999999992895, 30.03615769709734451, 42.44795908869000556 ) ) ;
#11897 = LINE ( 'NONE', #3634, #11120 ) ;
#11898 = VECTOR ( 'NONE', #29313, 1000.000000000000000 ) ;
#11899 = VERTEX_POINT ( 'NONE', #13188 ) ;
#11900 = DIRECTION ( 'NONE',  ( -1.000000000000000000, 0.000000000000000000, 0.000000000000000000 ) ) ;
#11901 = ORIENTED_EDGE ( 'NONE', *, *, #1502, .F. ) ;
#11902 = CIRCLE ( 'NONE', #14773, 7.199999999999993960 ) ;
#11903 = CARTESIAN_POINT ( 'NONE',  ( -35.50000000000000000, -115.0140978167138712, 0.0002176474015578471800 ) ) ;
#11904 = FACE_OUTER_BOUND ( 'NONE', #1890, .T. ) ;
#11905 = CARTESIAN_POINT ( 'NONE',  ( -35.54388159064475872, -112.6276912846090568, 2.816024454178448710 ) ) ;
#11906 = EDGE_CURVE ( 'NONE', #4350, #17135, #12461, .T. ) ;
#11907 = EDGE_LOOP ( 'NONE', ( #14917, #25876, #20658, #31863 ) ) ;
#11908 = CARTESIAN_POINT ( 'NONE',  ( -35.02454729103298803, -114.8876895276775087, 1.597274454178448710 ) ) ;
#11909 = CIRCLE ( 'NONE', #24599, 7.020000000000045759 ) ;
#11910 = EDGE_CURVE ( 'NONE', #13661, #1926, #21077, .T. ) ;
#11911 = AXIS2_PLACEMENT_3D ( 'NONE', #4933, #4758, #26540 ) ;
#11912 = DIRECTION ( 'NONE',  ( 0.000000000000000000, 0.000000000000000000, -1.000000000000000000 ) ) ;
#11913 = CARTESIAN_POINT ( 'NONE',  ( -35.50000000000000711, -116.0140978167138712, -0.5622823525984409487 ) ) ;
#11914 = ORIENTED_EDGE ( 'NONE', *, *, #5616, .T. ) ;
#11915 = EDGE_LOOP ( 'NONE', ( #3775, #20931, #8456, #15439 ) ) ;
#11916 = CIRCLE ( 'NONE', #29741, 47.49900000000000944 ) ;
#11917 = AXIS2_PLACEMENT_3D ( 'NONE', #8013, #23880, #7650 ) ;
#11918 = CARTESIAN_POINT ( 'NONE',  ( 8.000000000000000000, 18.48663108841359559, 4.615718728112120139 ) ) ;
#11919 = AXIS2_PLACEMENT_3D ( 'NONE', #32421, #24328, #10466 ) ;
#11920 = DIRECTION ( 'NONE',  ( 0.000000000000000000, 0.000000000000000000, 1.000000000000000000 ) ) ;
#11921 = ORIENTED_EDGE ( 'NONE', *, *, #35497, .T. ) ;
#11922 = ORIENTED_EDGE ( 'NONE', *, *, #1708, .F. ) ;
#11923 = CARTESIAN_POINT ( 'NONE',  ( -34.50000000000000000, -116.0140896356112989, -0.6575071456984549201 ) ) ;
#11924 = DIRECTION ( 'NONE',  ( -1.000000000000000000, 5.339440136655840161E-16, 0.000000000000000000 ) ) ;
#11925 = ORIENTED_EDGE ( 'NONE', *, *, #1450, .F. ) ;
#11926 = PRODUCT_DEFINITION_CONTEXT ( 'detailed design', #17894, 'design' ) ;
#11927 = ORIENTED_EDGE ( 'NONE', *, *, #6617, .T. ) ;
#11928 = DIRECTION ( 'NONE',  ( 1.000000000000000000, -0.000000000000000000, 0.000000000000000000 ) ) ;
#11929 = EDGE_CURVE ( 'NONE', #30594, #18020, #18488, .T. ) ;
#11930 = VECTOR ( 'NONE', #18981, 1000.000000000000000 ) ;
#11931 = VECTOR ( 'NONE', #16122, 1000.000000000000227 ) ;
#11932 = CARTESIAN_POINT ( 'NONE',  ( -37.34375000000001421, -113.9929510916434339, 13.11852480586264846 ) ) ;
#11933 = ADVANCED_FACE ( 'NONE', ( #34787 ), #4564, .T. ) ;
#11934 = CARTESIAN_POINT ( 'NONE',  ( -34.50000000000000000, -113.3557509229967764, 1.923098431109107054 ) ) ;
#11935 = DIRECTION ( 'NONE',  ( -1.000000000000000000, -0.000000000000000000, 0.000000000000000000 ) ) ;
#11936 = EDGE_CURVE ( 'NONE', #27419, #2812, #10462, .T. ) ;
#11937 = CARTESIAN_POINT ( 'NONE',  ( -36.00585935943765747, -113.9929510916434339, 13.11852578240983291 ) ) ;
#11938 = CIRCLE ( 'NONE', #18279, 4.000000000000000000 ) ;
#11939 = CARTESIAN_POINT ( 'NONE',  ( -35.50000000000000000, -115.9927366631908825, 10.47601115720670073 ) ) ;
#11940 = CARTESIAN_POINT ( 'NONE',  ( 8.000000000000000000, 7.317194182740155206, 18.61340026142653770 ) ) ;
#11941 = AXIS2_PLACEMENT_3D ( 'NONE', #18913, #31885, #32075 ) ;
#11942 = CARTESIAN_POINT ( 'NONE',  ( 0.000000000000000000, -0.3212489022564151142, -16.91141623315864706 ) ) ;
#11943 = EDGE_CURVE ( 'NONE', #16982, #26196, #15033, .T. ) ;
#11944 = CARTESIAN_POINT ( 'NONE',  ( 7.999999999999992895, 40.47821179127763003, -32.64221760512717196 ) ) ;
#11945 = CARTESIAN_POINT ( 'NONE',  ( 8.000000000000000000, 0.000000000000000000, 0.000000000000000000 ) ) ;
#11946 = EDGE_CURVE ( 'NONE', #23114, #9009, #10110, .T. ) ;
#11947 = CIRCLE ( 'NONE', #2188, 8.000000000000007105 ) ;
#11948 = LINE ( 'NONE', #17506, #31206 ) ;
#11949 = ORIENTED_EDGE ( 'NONE', *, *, #9935, .T. ) ;
#11950 = DIRECTION ( 'NONE',  ( -1.000000000000000000, 0.000000000000000000, 0.000000000000000000 ) ) ;
#11951 = CARTESIAN_POINT ( 'NONE',  ( 8.000000000000000000, 4.460989585141205360, -16.92083251265323085 ) ) ;
#11952 = CARTESIAN_POINT ( 'NONE',  ( -1.387778780781445676E-14, 0.4273491293403097746, -0.7999999999999951594 ) ) ;
#11953 = DIRECTION ( 'NONE',  ( -0.000000000000000000, 0.000000000000000000, -1.000000000000000000 ) ) ;
#11954 = ITEM_DEFINED_TRANSFORMATION ( 'NONE', 'NONE', #16141,  #21307 ) ;
#11955 = DIRECTION ( 'NONE',  ( 1.000000000000000000, 0.000000000000000000, 0.000000000000000000 ) ) ;
#11956 = DIRECTION ( 'NONE',  ( 0.000000000000000000, 0.000000000000000000, 1.000000000000000000 ) ) ;
#11957 = EDGE_CURVE ( 'NONE', #14072, #1616, #29427, .T. ) ;
#11958 = CIRCLE ( 'NONE', #5646, 47.49900000000001654 ) ;
#11959 = VERTEX_POINT ( 'NONE', #18387 ) ;
#11960 = DIRECTION ( 'NONE',  ( 0.000000000000000000, 0.000000000000000000, -1.000000000000000000 ) ) ;
#11961 = DIRECTION ( 'NONE',  ( -1.000000000000000000, -0.000000000000000000, -0.000000000000000000 ) ) ;
#11962 = DIRECTION ( 'NONE',  ( 0.000000000000000000, -0.7071067811865442421, -0.7071067811865509034 ) ) ;
#11963 = ORIENTED_EDGE ( 'NONE', *, *, #15171, .T. ) ;
#11964 = ORIENTED_EDGE ( 'NONE', *, *, #8583, .T. ) ;
#11965 = CARTESIAN_POINT ( 'NONE',  ( -36.25098837183129774, -113.3347980657956242, 2.816024454178448710 ) ) ;
#11966 = ORIENTED_EDGE ( 'NONE', *, *, #25520, .F. ) ;
#11967 = AXIS2_PLACEMENT_3D ( 'NONE', #18682, #29682, #35274 ) ;
#11968 = ORIENTED_EDGE ( 'NONE', *, *, #2986, .F. ) ;
#11969 = VERTEX_POINT ( 'NONE', #15674 ) ;
#11970 = CARTESIAN_POINT ( 'NONE',  ( 8.000000000000000000, 10.46102064772339979, 19.35373470438986487 ) ) ;
#11971 =( REPRESENTATION_RELATIONSHIP ('NONE','NONE', #26607, #2005 ) REPRESENTATION_RELATIONSHIP_WITH_TRANSFORMATION ( #26355 )SHAPE_REPRESENTATION_RELATIONSHIP( ) );
#11972 = VECTOR ( 'NONE', #30771, 1000.000000000000114 ) ;
#11973 = DIRECTION ( 'NONE',  ( 1.174092375852890260E-15, -4.222049128630259891E-16, -1.000000000000000000 ) ) ;
#11974 = EDGE_CURVE ( 'NONE', #15571, #29853, #35193, .T. ) ;
#11975 = DIRECTION ( 'NONE',  ( 1.226634733346697831E-16, 0.2588190451025116356, 0.9659258262890706437 ) ) ;
#11976 = EDGE_CURVE ( 'NONE', #1074, #34100, #13893, .T. ) ;
#11977 = CARTESIAN_POINT ( 'NONE',  ( -35.50640865667918433, -114.9929510916434339, 12.69998175888958514 ) ) ;
#11978 = CARTESIAN_POINT ( 'NONE',  ( -3.799999999999999822, -2.710505431213761085E-17, 45.00000000000000000 ) ) ;
#11979 = DIRECTION ( 'NONE',  ( 0.000000000000000000, -6.983129352544641692E-15, 1.000000000000000000 ) ) ;
#11980 = CARTESIAN_POINT ( 'NONE',  ( -34.50000000000000000, -114.9656200615856818, 10.26631071845107179 ) ) ;
#11981 = CYLINDRICAL_SURFACE ( 'NONE', #26615, 20.00000000000000355 ) ;
#11982 = EDGE_CURVE ( 'NONE', #6343, #16796, #33442, .T. ) ;
#11983 = DIRECTION ( 'NONE',  ( -1.000000000000000000, 0.000000000000000000, 0.000000000000000000 ) ) ;
#11984 = VERTEX_POINT ( 'NONE', #9758 ) ;
#11985 = CARTESIAN_POINT ( 'NONE',  ( -35.50000000000000000, -115.9929510916434481, 10.52000928670414126 ) ) ;
#11986 = CARTESIAN_POINT ( 'NONE',  ( -35.50000000000000711, -112.9415908020655195, 1.873661708251232572 ) ) ;
#11987 = DIRECTION ( 'NONE',  ( 1.000000000000000000, 0.000000000000000000, 0.000000000000000000 ) ) ;
#11988 = EDGE_CURVE ( 'NONE', #7064, #24774, #15589, .T. ) ;
#11989 = DIRECTION ( 'NONE',  ( 0.000000000000000000, 0.4817536741017163782, -0.8763066800438630288 ) ) ;
#11990 = AXIS2_PLACEMENT_3D ( 'NONE', #19269, #13535, #35511 ) ;
#11991 = DIRECTION ( 'NONE',  ( 0.000000000000000000, 0.000000000000000000, -1.000000000000000000 ) ) ;
#11992 = VECTOR ( 'NONE', #23521, 1000.000000000000000 ) ;
#11993 = CARTESIAN_POINT ( 'NONE',  ( 0.000000000000000000, 11.27190672109271219, 0.3151488735049640111 ) ) ;
#11994 = DIRECTION ( 'NONE',  ( 0.000000000000000000, 0.000000000000000000, 1.000000000000000000 ) ) ;
#11995 = CARTESIAN_POINT ( 'NONE',  ( 0.000000000000000000, 0.000000000000000000, -0.7999999999999951594 ) ) ;
#11996 = LINE ( 'NONE', #6056, #31621 ) ;
#11997 = VERTEX_POINT ( 'NONE', #18026 ) ;
#11998 = CARTESIAN_POINT ( 'NONE',  ( -36.94073759706868287, -115.0000000000000000, 5.871475545821551734 ) ) ;
#11999 = CYLINDRICAL_SURFACE ( 'NONE', #35392, 20.00000000000000355 ) ;
#12000 = CARTESIAN_POINT ( 'NONE',  ( 0.000000000000000000, -13.60411018104326963, 12.96676809804144348 ) ) ;
#12001 = ORIENTED_EDGE ( 'NONE', *, *, #24318, .T. ) ;
#12002 = ORIENTED_EDGE ( 'NONE', *, *, #11127, .F. ) ;
#12003 = DIRECTION ( 'NONE',  ( 0.000000000000000000, 0.000000000000000000, 1.000000000000000000 ) ) ;
#12004 = LINE ( 'NONE', #4272, #6023 ) ;
#12005 = ORIENTED_EDGE ( 'NONE', *, *, #23577, .F. ) ;
#12006 = CARTESIAN_POINT ( 'NONE',  ( -34.00000000000000000, -114.0592624029313242, 7.503524454178450043 ) ) ;
#12007 = ORIENTED_EDGE ( 'NONE', *, *, #24199, .F. ) ;
#12008 = DIRECTION ( 'NONE',  ( 1.000000000000000000, -0.000000000000000000, 0.000000000000000000 ) ) ;
#12009 = DIRECTION ( 'NONE',  ( -1.000000000000000000, 0.000000000000000000, 0.000000000000000000 ) ) ;
#12010 = PRODUCT_CONTEXT ( 'NONE', #31941, 'mechanical' ) ;
#12011 = DIRECTION ( 'NONE',  ( 0.000000000000000000, 0.000000000000000000, 1.000000000000000000 ) ) ;
#12012 = ORIENTED_EDGE ( 'NONE', *, *, #18508, .F. ) ;
#12013 = EDGE_LOOP ( 'NONE', ( #2699, #16695, #7121, #20258 ) ) ;
#12014 = CIRCLE ( 'NONE', #14856, 22.00000000000000000 ) ;
#12015 = EDGE_CURVE ( 'NONE', #20300, #17882, #31723, .T. ) ;
#12016 = CARTESIAN_POINT ( 'NONE',  ( -44.00000000000000000, -12.99999999999999822, 0.000000000000000000 ) ) ;
#12017 = DIRECTION ( 'NONE',  ( -1.000000000000000000, 0.000000000000000000, 0.000000000000000000 ) ) ;
#12018 = VERTEX_POINT ( 'NONE', #27397 ) ;
#12019 = CARTESIAN_POINT ( 'NONE',  ( -9.999999999999994671, 0.000000000000000000, 0.000000000000000000 ) ) ;
#12020 = CARTESIAN_POINT ( 'NONE',  ( -34.50000000000000000, -112.8655373925166572, 1.864575885149403423 ) ) ;
#12021 = CARTESIAN_POINT ( 'NONE',  ( 8.000000000000000000, -0.3212489022566501484, 16.91141623315869680 ) ) ;
#12022 = CARTESIAN_POINT ( 'NONE',  ( 0.000000000000000000, -19.35373470438975119, -10.46102064772362183 ) ) ;
#12023 = CARTESIAN_POINT ( 'NONE',  ( -34.50000000000000000, -115.9929510916434481, 10.61627146648203990 ) ) ;
#12024 = CARTESIAN_POINT ( 'NONE',  ( 0.000000000000000000, 0.000000000000000000, 0.000000000000000000 ) ) ;
#12025 = DIRECTION ( 'NONE',  ( 1.000000000000000000, -0.000000000000000000, -0.000000000000000000 ) ) ;
#12026 = CARTESIAN_POINT ( 'NONE',  ( -38.25557080230232998, -114.9929510916434339, 13.92914543265419525 ) ) ;
#12027 = CARTESIAN_POINT ( 'NONE',  ( -0.2142857142857362840, -10.49781318335649161, 0.000000000000000000 ) ) ;
#12028 = DIRECTION ( 'NONE',  ( -1.000000000000000000, 0.000000000000000000, 0.000000000000000000 ) ) ;
#12029 = CARTESIAN_POINT ( 'NONE',  ( 0.000000000000000000, -2.710505431213761085E-17, 54.99999999999999289 ) ) ;
#12030 = DIRECTION ( 'NONE',  ( -1.000000000000000000, 0.000000000000000000, 0.000000000000000000 ) ) ;
#12031 = ORIENTED_EDGE ( 'NONE', *, *, #18572, .T. ) ;
#12032 = CARTESIAN_POINT ( 'NONE',  ( 65.00000000000001421, -29.60243954609234507, 93.25429903592612391 ) ) ;
#12033 = ORIENTED_EDGE ( 'NONE', *, *, #2822, .F. ) ;
#12034 = CARTESIAN_POINT ( 'NONE',  ( -35.81662171581203324, -110.9754527089670546, 5.215225545821552622 ) ) ;
#12035 = CARTESIAN_POINT ( 'NONE',  ( 7.999999999999992895, 0.000000000000000000, 0.000000000000000000 ) ) ;
#12036 = CARTESIAN_POINT ( 'NONE',  ( -35.50000000000000711, -116.0140978167138712, -0.3747823525984422255 ) ) ;
#12037 = ORIENTED_EDGE ( 'NONE', *, *, #34873, .T. ) ;
#12038 = VECTOR ( 'NONE', #12057, 1000.000000000000000 ) ;
#12039 = ORIENTED_EDGE ( 'NONE', *, *, #10364, .F. ) ;
#12040 = CARTESIAN_POINT ( 'NONE',  ( -34.49999999999998579, -26.68172400785649856, 80.78589838486213637 ) ) ;
#12041 = FACE_OUTER_BOUND ( 'NONE', #5264, .T. ) ;
#12042 = ORIENTED_EDGE ( 'NONE', *, *, #2000, .F. ) ;
#12043 = ORIENTED_EDGE ( 'NONE', *, *, #5603, .F. ) ;
#12044 = CIRCLE ( 'NONE', #6876, 52.00000000000000711 ) ;
#12045 = FACE_OUTER_BOUND ( 'NONE', #11887, .T. ) ;
#12046 = ORIENTED_EDGE ( 'NONE', *, *, #18914, .F. ) ;
#12047 = CARTESIAN_POINT ( 'NONE',  ( -35.54388159064475872, -115.3723087153909432, 4.183975545821551734 ) ) ;
#12048 = DIRECTION ( 'NONE',  ( 1.000000000000000000, 0.000000000000000000, 0.000000000000000000 ) ) ;
#12049 = FACE_OUTER_BOUND ( 'NONE', #20126, .T. ) ;
#12050 = ORIENTED_EDGE ( 'NONE', *, *, #19171, .T. ) ;
#12051 = EDGE_LOOP ( 'NONE', ( #14533, #4056, #7580, #22935 ) ) ;
#12052 = CARTESIAN_POINT ( 'NONE',  ( -35.50000000000000000, -115.3399256288223569, -2.599147725881697291 ) ) ;
#12053 = EDGE_CURVE ( 'NONE', #2729, #15714, #25980, .T. ) ;
#12054 = UNCERTAINTY_MEASURE_WITH_UNIT (LENGTH_MEASURE( 1.000000000000000082E-05 ), #13181, 'distance_accuracy_value', 'NONE');
#12055 = PLANE ( 'NONE',  #12065 ) ;
#12056 = ORIENTED_EDGE ( 'NONE', *, *, #21968, .T. ) ;
#12057 = DIRECTION ( 'NONE',  ( 0.000000000000000000, 0.000000000000000000, 1.000000000000000000 ) ) ;
#12058 = VECTOR ( 'NONE', #19054, 1000.000000000000000 ) ;
#12059 = CARTESIAN_POINT ( 'NONE',  ( -34.50000000000000000, -114.0371586325023117, 9.504435485030890973 ) ) ;
#12060 = DIRECTION ( 'NONE',  ( 0.000000000000000000, 0.9510565162951545304, -0.3090169943749448977 ) ) ;
#12061 = CARTESIAN_POINT ( 'NONE',  ( 4.000000000000000000, 4.627536653468036720E-16, 54.99999999999999289 ) ) ;
#12062 = EDGE_CURVE ( 'NONE', #4579, #19119, #2996, .T. ) ;
#12063 = CYLINDRICAL_SURFACE ( 'NONE', #14952, 8.000000000000001776 ) ;
#12064 = CARTESIAN_POINT ( 'NONE',  ( -36.00976557831293690, -113.9929510916434339, 14.11852773550420359 ) ) ;
#12066 = CYLINDRICAL_SURFACE ( 'NONE', #34294, 7.199999999999993960 ) ;
#12065 = AXIS2_PLACEMENT_3D ( 'NONE', #32214, #8068, #35112 ) ;
#12067 = CARTESIAN_POINT ( 'NONE',  ( -35.93473953453761283, -114.9929510916434339, 13.11451721564123574 ) ) ;
#12068 = CARTESIAN_POINT ( 'NONE',  ( 8.000000000000000000, 18.62763138773855687, 2.494040418455418351 ) ) ;
#12069 = EDGE_LOOP ( 'NONE', ( #29502, #26685, #15598, #20219, #14461, #1068 ) ) ;
#12070 = CARTESIAN_POINT ( 'NONE',  ( 7.999999999999992895, 0.000000000000000000, 0.000000000000000000 ) ) ;
#12071 = CARTESIAN_POINT ( 'NONE',  ( 7.999999999999992895, 0.000000000000000000, 0.000000000000000000 ) ) ;
#12072 = ORIENTED_EDGE ( 'NONE', *, *, #25639, .T. ) ;
#12073 = CARTESIAN_POINT ( 'NONE',  ( -35.50000000000000711, -114.8847986568751907, 10.03799953695244618 ) ) ;
#12074 = ORIENTED_EDGE ( 'NONE', *, *, #12143, .T. ) ;
#12075 = DIRECTION ( 'NONE',  ( 0.000000000000000000, 0.5877852522924685852, 0.8090169943749507819 ) ) ;
#12076 = EDGE_LOOP ( 'NONE', ( #12777, #4920, #2215, #18524 ) ) ;
#12077 = CARTESIAN_POINT ( 'NONE',  ( -34.49999999999998579, -28.69486372867093849, 81.70096189432322831 ) ) ;
#12078 = ORIENTED_EDGE ( 'NONE', *, *, #1342, .F. ) ;
#12079 = CARTESIAN_POINT ( 'NONE',  ( -35.50000000000000000, -113.0140978167136581, -0.6247823525984268489 ) ) ;
#12080 = DIRECTION ( 'NONE',  ( -1.000000000000000000, 0.000000000000000000, 0.000000000000000000 ) ) ;
#12081 = CARTESIAN_POINT ( 'NONE',  ( 7.999999999999992895, -51.19683565102450729, 9.104066087303298360 ) ) ;
#12082 = AXIS2_PLACEMENT_3D ( 'NONE', #22942, #17532, #1349 ) ;
#12083 = ORIENTED_EDGE ( 'NONE', *, *, #24046, .F. ) ;
#12084 = CARTESIAN_POINT ( 'NONE',  ( -37.05926240293131713, -115.9999999999999858, 1.878524454178448710 ) ) ;
#12085 = EDGE_CURVE ( 'NONE', #19855, #21964, #23081, .T. ) ;
#12086 = VECTOR ( 'NONE', #19062, 1000.000000000000000 ) ;
#12087 = ADVANCED_BREP_SHAPE_REPRESENTATION ( '', ( #10186, #21307 ), #13295 ) ;
#12088 = CARTESIAN_POINT ( 'NONE',  ( 0.1085714285714300953, -3.798448662927791819, -0.7999999999999951594 ) ) ;
#12089 = CARTESIAN_POINT ( 'NONE',  ( -35.50000000000000711, -115.1770117227680998, -1.611965039240062181 ) ) ;
#12090 = ORIENTED_EDGE ( 'NONE', *, *, #6617, .F. ) ;
#12091 = ORIENTED_EDGE ( 'NONE', *, *, #28004, .T. ) ;
#12092 = DIRECTION ( 'NONE',  ( -1.000000000000000000, 0.000000000000000000, 0.000000000000000000 ) ) ;
#12093 = AXIS2_PLACEMENT_3D ( 'NONE', #34602, #23791, #32596 ) ;
#12094 = PRESENTATION_STYLE_ASSIGNMENT (( #1122 ) ) ;
#12095 = DIRECTION ( 'NONE',  ( -1.226634733346697831E-16, -0.7071067811865466846, -0.7071067811865483499 ) ) ;
#12096 = ORIENTED_EDGE ( 'NONE', *, *, #16687, .T. ) ;
#12097 = ORIENTED_EDGE ( 'NONE', *, *, #23308, .F. ) ;
#12098 = CARTESIAN_POINT ( 'NONE',  ( -34.50000000000000000, -115.3362660311619692, -1.573728109101206085 ) ) ;
#12099 = CARTESIAN_POINT ( 'NONE',  ( 8.000000000000007105, 8.725776631572825792, 3.753907720749072308 ) ) ;
#12100 = EDGE_CURVE ( 'NONE', #6142, #31456, #27142, .T. ) ;
#12101 = PRODUCT_DEFINITION_SHAPE ( 'NONE', 'NONE',  #35626 ) ;
#12102 = EDGE_CURVE ( 'NONE', #23663, #28798, #27705, .T. ) ;
#12103 = ADVANCED_FACE ( 'NONE', ( #33807 ), #32969, .F. ) ;
#12104 = VERTEX_POINT ( 'NONE', #16200 ) ;
#12105 = ORIENTED_EDGE ( 'NONE', *, *, #20001, .F. ) ;
#12106 = CARTESIAN_POINT ( 'NONE',  ( 1.110223024625156540E-13, -1.000000000000042633, -44.50000000000000000 ) ) ;
#12107 = CARTESIAN_POINT ( 'NONE',  ( -37.51635661748575501, -113.9929510916434339, 13.11827392651459512 ) ) ;
#12108 = CARTESIAN_POINT ( 'NONE',  ( -34.50000000000000000, -112.7765286249690035, 1.847058736912741583 ) ) ;
#12109 = AXIS2_PLACEMENT_3D ( 'NONE', #17942, #1757, #18121 ) ;
#12110 = DIRECTION ( 'NONE',  ( 1.000000000000000000, -5.339440136655842133E-16, -1.047965281155519420E-16 ) ) ;
#12111 = ADVANCED_FACE ( 'NONE', ( #21970 ), #29743, .F. ) ;
#12112 = CARTESIAN_POINT ( 'NONE',  ( -35.97955704204053262, -113.9929510916434339, 13.11812344617474402 ) ) ;
#12113 = EDGE_CURVE ( 'NONE', #1241, #5458, #5431, .T. ) ;
#12114 = CARTESIAN_POINT ( 'NONE',  ( -35.50000000000000000, -115.9929510916434481, 12.26648026267477398 ) ) ;
#12115 = UNCERTAINTY_MEASURE_WITH_UNIT (LENGTH_MEASURE( 1.000000000000000082E-05 ), #4060, 'distance_accuracy_value', 'NONE');
#12116 = CARTESIAN_POINT ( 'NONE',  ( 0.000000000000000000, -24.47917365149978153, 45.87777302070926311 ) ) ;
#12117 = AXIS2_PLACEMENT_3D ( 'NONE', #2140, #29133, #34535 ) ;
#12118 = CARTESIAN_POINT ( 'NONE',  ( 0.000000000000000000, 0.000000000000000000, -0.7999999999999951594 ) ) ;
#12119 = CIRCLE ( 'NONE', #12693, 52.00000000000000711 ) ;
#12120 = DIRECTION ( 'NONE',  ( 0.000000000000000000, -0.6845471059286951654, 0.7289686274214054462 ) ) ;
#12121 = CARTESIAN_POINT ( 'NONE',  ( -55.00000000000000000, -25.98076211353320275, 84.99999999999994316 ) ) ;
#12122 = CYLINDRICAL_SURFACE ( 'NONE', #161, 3.799999999999999822 ) ;
#12123 = ORIENTED_EDGE ( 'NONE', *, *, #17374, .T. ) ;
#12124 = DIRECTION ( 'NONE',  ( -1.000000000000000000, 0.000000000000000000, -0.000000000000000000 ) ) ;
#12125 = CARTESIAN_POINT ( 'NONE',  ( -35.50000000000000711, -113.6318576702834804, 1.956056246348823580 ) ) ;
#12126 = DIRECTION ( 'NONE',  ( -1.000000000000000000, 0.000000000000000000, -0.000000000000000000 ) ) ;
#12127 = CARTESIAN_POINT ( 'NONE',  ( -1.519999999999993578, 0.000000000000000000, 0.000000000000000000 ) ) ;
#12128 = DIRECTION ( 'NONE',  ( -1.000000000000000000, 0.000000000000000000, 0.000000000000000000 ) ) ;
#12129 = ADVANCED_FACE ( 'NONE', ( #24338 ), #35506, .T. ) ;
#12130 = EDGE_LOOP ( 'NONE', ( #3026, #15043, #21222, #19499 ) ) ;
#12131 = CYLINDRICAL_SURFACE ( 'NONE', #33708, 10.99999999999999645 ) ;
#12132 = CARTESIAN_POINT ( 'NONE',  ( -34.50000000000000000, -111.1162063037085801, -1.269118781493287607 ) ) ;
#12133 = ADVANCED_FACE ( 'NONE', ( #24862 ), #5611, .T. ) ;
#12134 = CARTESIAN_POINT ( 'NONE',  ( -1.599999999999989875, -3.455569164145799535E-16, -4.980000000000017302 ) ) ;
#12135 = ORIENTED_EDGE ( 'NONE', *, *, #27500, .T. ) ;
#12136 = EDGE_LOOP ( 'NONE', ( #30615, #21113 ) ) ;
#12137 = CARTESIAN_POINT ( 'NONE',  ( -37.35495115944176092, -112.9754527089670688, 4.034774454178449155 ) ) ;
#12138 = VERTEX_POINT ( 'NONE', #13357 ) ;
#12139 = SHAPE_REPRESENTATION_RELATIONSHIP ( 'NONE' , 'NONE' ,  #4547, #10385 ) ;
#12140 = ORIENTED_EDGE ( 'NONE', *, *, #20014, .T. ) ;
#12141 = VERTEX_POINT ( 'NONE', #22805 ) ;
#12142 = CARTESIAN_POINT ( 'NONE',  ( -35.50000000000000000, -114.8057644833805853, -0.6247823525984269599 ) ) ;
#12143 = EDGE_CURVE ( 'NONE', #19005, #17954, #21792, .T. ) ;
#12144 = EDGE_CURVE ( 'NONE', #28744, #14626, #25415, .T. ) ;
#12145 = ADVANCED_FACE ( 'NONE', ( #30268 ), #27579, .T. ) ;
#12146 = VECTOR ( 'NONE', #3641, 1000.000000000000000 ) ;
#12147 = AXIS2_PLACEMENT_3D ( 'NONE', #31663, #22847, #1250 ) ;
#12148 = CARTESIAN_POINT ( 'NONE',  ( -1.599999999999989653, -4.694161725993254197E-16, -6.765000000000044977 ) ) ;
#12149 = FACE_OUTER_BOUND ( 'NONE', #16778, .T. ) ;
#12150 = CARTESIAN_POINT ( 'NONE',  ( -35.52552712174884419, -114.9929510916434339, 12.77960891308624447 ) ) ;
#12151 = DIRECTION ( 'NONE',  ( 1.000000000000000000, 0.000000000000000000, 0.000000000000000000 ) ) ;
#12152 = CARTESIAN_POINT ( 'NONE',  ( 8.000000000000000000, 0.000000000000000000, 0.000000000000000000 ) ) ;
#12153 = EDGE_CURVE ( 'NONE', #11623, #20005, #21928, .T. ) ;
#12154 = CARTESIAN_POINT ( 'NONE',  ( -34.50000000000000000, -114.9929510916434339, 12.56351784598954424 ) ) ;
#12155 = DIRECTION ( 'NONE',  ( 0.000000000000000000, 0.5877852522924681411, 0.8090169943749510040 ) ) ;
#12156 = CARTESIAN_POINT ( 'NONE',  ( 4.000000000000003553, -21.80633394113448276, -2.912696353506054159 ) ) ;
#12157 = EDGE_LOOP ( 'NONE', ( #18346, #2513 ) ) ;
#12158 = CARTESIAN_POINT ( 'NONE',  ( -35.50000000000000000, -115.9929510916434481, 10.53376102667243508 ) ) ;
#12159 = CARTESIAN_POINT ( 'NONE',  ( -35.50000000000000711, -112.0140978167138712, 0.0002176474015661141945 ) ) ;
#12160 = DIRECTION ( 'NONE',  ( 8.708451184622495809E-17, -6.938893903907203726E-17, -1.000000000000000000 ) ) ;
#12161 = PLANE ( 'NONE',  #3181 ) ;
#12162 = DIRECTION ( 'NONE',  ( -1.000000000000000000, -0.000000000000000000, -0.000000000000000000 ) ) ;
#12163 = DIRECTION ( 'NONE',  ( 0.000000000000000000, 0.000000000000000000, 1.000000000000000000 ) ) ;
#12164 = CARTESIAN_POINT ( 'NONE',  ( 0.000000000000000000, 0.000000000000000000, 0.000000000000000000 ) ) ;
#12165 = CARTESIAN_POINT ( 'NONE',  ( 44.00000000000000000, 1.616533774874506480E-14, 0.000000000000000000 ) ) ;
#12166 = DIRECTION ( 'NONE',  ( 8.708451184622495809E-17, -6.938893903907203726E-17, -1.000000000000000000 ) ) ;
#12167 = ORIENTED_EDGE ( 'NONE', *, *, #16956, .F. ) ;
#12168 = VECTOR ( 'NONE', #8285, 1000.000000000000000 ) ;
#12169 =( GEOMETRIC_REPRESENTATION_CONTEXT ( 3 ) GLOBAL_UNCERTAINTY_ASSIGNED_CONTEXT ( ( #30555 ) ) GLOBAL_UNIT_ASSIGNED_CONTEXT ( ( #8317, #401, #9391 ) ) REPRESENTATION_CONTEXT ( 'NONE', 'WORKASPACE' ) );
#12170 = CARTESIAN_POINT ( 'NONE',  ( -35.97545270896705460, -114.3549511594417680, 8.590225545821549957 ) ) ;
#12171 = CIRCLE ( 'NONE', #1835, 19.99999999999999289 ) ;
#12172 = CARTESIAN_POINT ( 'NONE',  ( 8.000000000000000000, 12.96676809804168862, -13.60411018104304048 ) ) ;
#12173 = CARTESIAN_POINT ( 'NONE',  ( 39.30000000000000426, 7.219292880973646134E-15, 0.000000000000000000 ) ) ;
#12174 = EDGE_CURVE ( 'NONE', #11237, #18917, #26555, .T. ) ;
#12175 = VERTEX_POINT ( 'NONE', #25527 ) ;
#12176 = VERTEX_POINT ( 'NONE', #843 ) ;
#12177 = EDGE_CURVE ( 'NONE', #10949, #17665, #11825, .T. ) ;
#12178 = DIRECTION ( 'NONE',  ( 1.000000000000000000, -1.110223024625156540E-16, 0.000000000000000000 ) ) ;
#12179 = EDGE_CURVE ( 'NONE', #9296, #17469, #24287, .T. ) ;
#12180 = LINE ( 'NONE', #23329, #11767 ) ;
#12181 = ORIENTED_EDGE ( 'NONE', *, *, #10570, .T. ) ;
#12182 = CARTESIAN_POINT ( 'NONE',  ( -35.69809690994941320, -116.9754527089670546, 8.777725545821549957 ) ) ;
#12183 = ORIENTED_EDGE ( 'NONE', *, *, #25579, .F. ) ;
#12184 = SURFACE_STYLE_USAGE ( .BOTH. , #1382 ) ;
#12185 = COLOUR_RGB ( '', 0.66274510, 0.83137255, 0.94901961) ;
#12186 = CARTESIAN_POINT ( 'NONE',  ( -37.49999999999999289, -11.24969279549607748, 111.5585998451919778 ) ) ;
#12187 = CARTESIAN_POINT ( 'NONE',  ( -46.00000000000000000, 9.797174393178825657E-16, -8.000000000000000000 ) ) ;
#12188 = DIRECTION ( 'NONE',  ( 1.000000000000000000, -5.339440136655842133E-16, -1.047965281155519420E-16 ) ) ;
#12189 = EDGE_CURVE ( 'NONE', #1876, #27933, #31276, .T. ) ;
#12190 = ADVANCED_FACE ( 'NONE', ( #17395 ), #18115, .T. ) ;
#12191 = PRODUCT_CONTEXT ( 'NONE', #6862, 'mechanical' ) ;
#12192 = DIRECTION ( 'NONE',  ( -1.174092375852890457E-15, 4.222049128630259891E-16, 1.000000000000000000 ) ) ;
#12193 = VERTEX_POINT ( 'NONE', #26061 ) ;
#12194 = VERTEX_POINT ( 'NONE', #6786 ) ;
#12195 = DIRECTION ( 'NONE',  ( 0.000000000000000000, 0.9848077530122073542, 0.1736481776669339394 ) ) ;
#12196 = CARTESIAN_POINT ( 'NONE',  ( 7.999999999999992895, -39.64889472655756464, 33.64468972902493960 ) ) ;
#12197 =( GEOMETRIC_REPRESENTATION_CONTEXT ( 3 ) GLOBAL_UNCERTAINTY_ASSIGNED_CONTEXT ( ( #23214 ) ) GLOBAL_UNIT_ASSIGNED_CONTEXT ( ( #13706, #30608, #14216 ) ) REPRESENTATION_CONTEXT ( 'NONE', 'WORKASPACE' ) );
#12198 = ORIENTED_EDGE ( 'NONE', *, *, #34763, .T. ) ;
#12199 = CIRCLE ( 'NONE', #18513, 20.00000000000000711 ) ;
#12200 = PLANE ( 'NONE',  #29172 ) ;
#12201 = CARTESIAN_POINT ( 'NONE',  ( -34.50000000000000000, -115.0140978167138428, -0.6247823525979866455 ) ) ;
#12202 = DIRECTION ( 'NONE',  ( -1.000000000000000000, 0.000000000000000000, 0.000000000000000000 ) ) ;
#12203 = DIRECTION ( 'NONE',  ( -1.000000000000000000, -0.000000000000000000, -0.000000000000000000 ) ) ;
#12204 = CARTESIAN_POINT ( 'NONE',  ( -34.50000000000000000, -114.2450133963102843, 8.522190569412378736 ) ) ;
#12205 = DIRECTION ( 'NONE',  ( -1.000000000000000000, -0.000000000000000000, -0.000000000000000000 ) ) ;
#12206 = FACE_OUTER_BOUND ( 'NONE', #23888, .T. ) ;
#12207 = CARTESIAN_POINT ( 'NONE',  ( -37.52454134262690388, -114.9929510916434339, 14.11837420659362152 ) ) ;
#12208 = CARTESIAN_POINT ( 'NONE',  ( 4.000000000000000000, 4.898587196589412829E-16, -39.50000000000000711 ) ) ;
#12209 = CARTESIAN_POINT ( 'NONE',  ( 0.000000000000000000, -43.83938735307256707, -18.28286404005846677 ) ) ;
#12210 = CIRCLE ( 'NONE', #20816, 52.00000000000000711 ) ;
#12211 = DIRECTION ( 'NONE',  ( 0.000000000000000000, 0.000000000000000000, 1.000000000000000000 ) ) ;
#12212 = LINE ( 'NONE', #34181, #13514 ) ;
#12213 = CARTESIAN_POINT ( 'NONE',  ( 7.999999999999992895, 44.61570720899095477, -14.73072383765580717 ) ) ;
#12214 = ORIENTED_EDGE ( 'NONE', *, *, #5165, .F. ) ;
#12215 = CARTESIAN_POINT ( 'NONE',  ( -39.07941549657749647, -116.1632251905417803, 4.558975545821549957 ) ) ;
#12216 = CARTESIAN_POINT ( 'NONE',  ( -42.49999999999999289, -8.980762113533204527, 86.49999999999994316 ) ) ;
#12217 = CARTESIAN_POINT ( 'NONE',  ( -35.50000000000000000, -113.0140978167138712, -0.4997823525984338988 ) ) ;
#12218 = EDGE_CURVE ( 'NONE', #7350, #33894, #1217, .T. ) ;
#12219 = ORIENTED_EDGE ( 'NONE', *, *, #30477, .F. ) ;
#12220 = ORIENTED_EDGE ( 'NONE', *, *, #7091, .T. ) ;
#12221 = EDGE_CURVE ( 'NONE', #32738, #14850, #20095, .T. ) ;
#12222 = CARTESIAN_POINT ( 'NONE',  ( 50.00000000000000000, 1.347111479062088405E-15, 11.00000000000000000 ) ) ;
#12223 = B_SPLINE_CURVE_WITH_KNOTS ( 'NONE', 3,
 ( #31246, #17010, #1010, #20063, #6226, #22954, #14485, #9279, #28367, #11986, #20235, #25495, #33580, #17542, #6566, #8914, #25320, #3710, #31069, #19700, #1187, #9103, #812, #30891, #23132, #28548, #3896, #19878, #22773, #14852, #14142, #25861, #8733, #33774, #6048, #12159, #31422, #34128, #20410, #6752, #17728, #3185, #469, #11452, #22418, #33410, #30716, #28020, #3367, #14314, #639, #11617, #17188, #4082, #34848, #4615, #9639, #24052, #32135, #18262, #23310, #12701, #7106, #4252, #34491, #4787, #28903, #7465, #29267, #20773, #26029, #1905, #15189, #26747, #20600, #18445, #29442, #1357, #31598, #34310, #18079, #15730, #31774, #12333, #12880, #26198, #2088, #6933, #13067, #35037, #17906, #1536, #12519, #29080, #28731, #23496, #9810, #23677, #4429, #15372, #26383, #1717 ),
 .UNSPECIFIED., .F., .F.,
 ( 4, 2, 2, 2, 2, 2, 2, 2, 2, 2, 2, 2, 2, 2, 2, 2, 2, 2, 2, 2, 2, 2, 2, 2, 2, 2, 2, 2, 2, 2, 2, 2, 2, 2, 2, 2, 2, 2, 2, 2, 2, 2, 2, 2, 2, 2, 2, 2, 2, 2, 4 ),
 ( 0.000000000000000000, 0.05194669433742771930, 0.07792004150614158242, 0.09090671509049851051, 0.09740005188267697456, 0.1038933886748554386, 0.1123700156520060500, 0.1208466426291566476, 0.1377998965834578704, 0.1717064044920602883, 0.2056129124006627062, 0.2225661663549639291, 0.2310427933321145266, 0.2395194203092651519, 0.2482763131408625423, 0.2570332059724599327, 0.2745469916356546580, 0.3095745629620442196, 0.3446021342884337813, 0.3621159199516285621, 0.3708728127832259247, 0.3796297056148233429, 0.3887999023441631730, 0.3979700990735030031, 0.4163104925321826633, 0.4529912794495420392, 0.4896720663669014151, 0.5080124598255810753, 0.5171826565549209054, 0.5263528532842607355, 0.5380287103930572190, 0.5497045675018538136, 0.5730562817194468916, 0.6197597101546329368, 0.6664631385898189819, 0.6898148528074120600, 0.7014907099162086546, 0.7131665670250051381, 0.7223367637543449682, 0.7315069604836847983, 0.7498473539423643475, 0.7865281408597235568, 0.8232089277770826552, 0.8415493212357623154, 0.8507195179651021455, 0.8598897146944418646, 0.8686466075260392827, 0.8774035003576365899, 0.8949172860208314262, 0.9299448573472208768, 1.000000000000000000 ),
 .UNSPECIFIED. ) ;
#12224 = AXIS2_PLACEMENT_3D ( 'NONE', #23633, #12110, #26339 ) ;
#12225 = DIRECTION ( 'NONE',  ( 0.000000000000000000, -0.9510565162951565288, 0.3090169943749383474 ) ) ;
#12226 = EDGE_LOOP ( 'NONE', ( #9073, #28655, #7831, #30469 ) ) ;
#12227 = VECTOR ( 'NONE', #18641, 1000.000000000000000 ) ;
#12228 = EDGE_LOOP ( 'NONE', ( #35230, #260, #21912, #1195 ) ) ;
#12229 = CIRCLE ( 'NONE', #28902, 7.199999999999992184 ) ;
#12230 = FACE_OUTER_BOUND ( 'NONE', #16013, .T. ) ;
#12231 = CARTESIAN_POINT ( 'NONE',  ( -36.94073759706868287, -115.9999999999999858, 2.871475545821551290 ) ) ;
#12232 = DIRECTION ( 'NONE',  ( 0.000000000000000000, 0.000000000000000000, 1.000000000000000000 ) ) ;
#12233 = DIRECTION ( 'NONE',  ( -1.000000000000000000, 0.000000000000000000, 0.000000000000000000 ) ) ;
#12234 = ORIENTED_EDGE ( 'NONE', *, *, #18508, .T. ) ;
#12235 = VERTEX_POINT ( 'NONE', #4285 ) ;
#12236 = CIRCLE ( 'NONE', #32358, 0.2000000000000000944 ) ;
#12237 = CARTESIAN_POINT ( 'NONE',  ( -35.50000000000000000, -116.7615919857705080, -1.632210089000343700 ) ) ;
#12238 = CIRCLE ( 'NONE', #16823, 7.199999999999993072 ) ;
#12239 = DIRECTION ( 'NONE',  ( 0.000000000000000000, -0.5000000000000067724, 0.8660254037844348218 ) ) ;
#12240 = LINE ( 'NONE', #3977, #31013 ) ;
#12241 = ORIENTED_EDGE ( 'NONE', *, *, #587, .T. ) ;
#12242 = CARTESIAN_POINT ( 'NONE',  ( -38.00000000000000711, -114.9929510916434339, 12.26648026267477043 ) ) ;
#12243 = AXIS2_PLACEMENT_3D ( 'NONE', #33208, #33547, #17324 ) ;
#12244 = CARTESIAN_POINT ( 'NONE',  ( -37.52454134262689678, -113.9929510916434339, 14.11837420659362152 ) ) ;
#12245 = VECTOR ( 'NONE', #17987, 1000.000000000000000 ) ;
#12246 = CARTESIAN_POINT ( 'NONE',  ( 0.000000000000000000, 0.000000000000000000, -33.50000000000000711 ) ) ;
#12247 = CYLINDRICAL_SURFACE ( 'NONE', #5375, 19.99999999999998579 ) ;
#12248 = CARTESIAN_POINT ( 'NONE',  ( -38.99879592093640213, -113.9929510916434339, 12.67985367974111277 ) ) ;
#12249 = CARTESIAN_POINT ( 'NONE',  ( 0.000000000000000000, 0.000000000000000000, 65.00000000000000000 ) ) ;
#12250 = CARTESIAN_POINT ( 'NONE',  ( -37.37500000000009237, -114.9929510916434339, 13.11852480586264669 ) ) ;
#12251 = DIRECTION ( 'NONE',  ( -1.000000000000000000, 0.000000000000000000, 0.000000000000000000 ) ) ;
#12252 = EDGE_LOOP ( 'NONE', ( #10191, #7038, #33614, #16507 ) ) ;
#12253 = CARTESIAN_POINT ( 'NONE',  ( 0.000000000000000000, 0.000000000000000000, 0.000000000000000000 ) ) ;
#12254 = DIRECTION ( 'NONE',  ( 1.000000000000000000, 0.000000000000000000, 0.000000000000000000 ) ) ;
#12255 = ORIENTED_EDGE ( 'NONE', *, *, #12327, .T. ) ;
#12256 = CARTESIAN_POINT ( 'NONE',  ( -35.50000000000000711, -114.9929510916434339, 12.56351784598954424 ) ) ;
#12257 = ORIENTED_EDGE ( 'NONE', *, *, #17786, .T. ) ;
#12258 = DIRECTION ( 'NONE',  ( -1.000000000000000000, 0.000000000000000000, 0.000000000000000000 ) ) ;
#12259 = EDGE_LOOP ( 'NONE', ( #22081, #20039, #22951, #527 ) ) ;
#12260 = CARTESIAN_POINT ( 'NONE',  ( 8.000000000000007105, 9.919332006307222116, 5.363026430117163734 ) ) ;
#12261 = VERTEX_POINT ( 'NONE', #1390 ) ;
#12262 = CIRCLE ( 'NONE', #17404, 17.49900000000001299 ) ;
#12263 = EDGE_CURVE ( 'NONE', #35453, #12842, #15053, .T. ) ;
#12264 = CARTESIAN_POINT ( 'NONE',  ( -34.50000000000000000, -113.0140978167140702, 0.8752176474015694874 ) ) ;
#12265 = FACE_OUTER_BOUND ( 'NONE', #6069, .T. ) ;
#12266 = DIRECTION ( 'NONE',  ( 0.000000000000000000, -0.4999999999999891753, -0.8660254037844450359 ) ) ;
#12267 = ORIENTED_EDGE ( 'NONE', *, *, #12218, .F. ) ;
#12268 = CARTESIAN_POINT ( 'NONE',  ( -35.54388159064475872, -112.6276912846090568, 4.316024454178448266 ) ) ;
#12269 = DIRECTION ( 'NONE',  ( -1.000000000000000000, 0.000000000000000000, 0.000000000000000000 ) ) ;
#12270 = CIRCLE ( 'NONE', #15123, 8.000000000000010658 ) ;
#12271 = CARTESIAN_POINT ( 'NONE',  ( -35.50000000000000711, -114.9307644833806137, -1.624782352598427959 ) ) ;
#12272 = AXIS2_PLACEMENT_3D ( 'NONE', #12378, #1402, #6613 ) ;
#12273 = ORIENTED_EDGE ( 'NONE', *, *, #27989, .T. ) ;
#12274 = ORIENTED_EDGE ( 'NONE', *, *, #23106, .T. ) ;
#12275 = FACE_OUTER_BOUND ( 'NONE', #1061, .T. ) ;
#12276 = EDGE_CURVE ( 'NONE', #28609, #28924, #25007, .T. ) ;
#12277 = CIRCLE ( 'NONE', #19181, 0.5000000000000004441 ) ;
#12278 = PRESENTATION_STYLE_ASSIGNMENT (( #4190 ) ) ;
#12279 = CARTESIAN_POINT ( 'NONE',  ( -3.800000000000018918, 1.765716931999654070E-14, -0.7999999999999907185 ) ) ;
#12280 = ORIENTED_EDGE ( 'NONE', *, *, #4919, .F. ) ;
#12281 = ORIENTED_EDGE ( 'NONE', *, *, #11087, .F. ) ;
#12282 = CARTESIAN_POINT ( 'NONE',  ( -34.50000000000000000, -112.1403507321855528, -1.128496220798856253 ) ) ;
#12283 = ORIENTED_EDGE ( 'NONE', *, *, #4352, .T. ) ;
#12284 = ORIENTED_EDGE ( 'NONE', *, *, #2120, .T. ) ;
#12285 = CARTESIAN_POINT ( 'NONE',  ( -42.49999999999999289, -25.98076211353322051, 84.99999999999992895 ) ) ;
#12286 = AXIS2_PLACEMENT_3D ( 'NONE', #11061, #27456, #35077 ) ;
#12287 = CARTESIAN_POINT ( 'NONE',  ( -37.99839555572501837, -113.9929510916434339, 12.65937477241749143 ) ) ;
#12288 = CARTESIAN_POINT ( 'NONE',  ( 7.999999999999992895, 42.03146605346787368, 22.12489237027333289 ) ) ;
#12289 = CARTESIAN_POINT ( 'NONE',  ( -35.50000000000000000, -113.9929510916434339, 11.38636890470581164 ) ) ;
#12290 = CARTESIAN_POINT ( 'NONE',  ( -35.50000000000000000, -115.9929492010520846, 10.50058572605509966 ) ) ;
#12291 = FACE_OUTER_BOUND ( 'NONE', #7029, .T. ) ;
#12293 = CIRCLE ( 'NONE', #16307, 14.00000000000000000 ) ;
#12292 = DIRECTION ( 'NONE',  ( 0.000000000000000000, 0.000000000000000000, -1.000000000000000000 ) ) ;
#12294 = VECTOR ( 'NONE', #35419, 1000.000000000000000 ) ;
#12295 = CYLINDRICAL_SURFACE ( 'NONE', #3929, 17.49900000000000233 ) ;
#12296 = DIRECTION ( 'NONE',  ( 0.000000000000000000, 0.000000000000000000, 1.000000000000000000 ) ) ;
#12297 = CARTESIAN_POINT ( 'NONE',  ( -37.49999999999999289, -11.52052244843579309, 118.1848168619253556 ) ) ;
#12298 = ORIENTED_EDGE ( 'NONE', *, *, #20257, .T. ) ;
#12299 = CARTESIAN_POINT ( 'NONE',  ( 8.000000000000007105, -10.15474465512046542, 9.637487275701101197 ) ) ;
#12300 = EDGE_CURVE ( 'NONE', #11168, #22745, #17936, .T. ) ;
#12301 = FACE_OUTER_BOUND ( 'NONE', #14684, .T. ) ;
#12302 = LINE ( 'NONE', #34461, #5254 ) ;
#12303 = EDGE_CURVE ( 'NONE', #13869, #28836, #28312, .T. ) ;
#12304 = CARTESIAN_POINT ( 'NONE',  ( -35.50000000000000711, -114.1712995509219724, 9.522174004479579068 ) ) ;
#12305 = CARTESIAN_POINT ( 'NONE',  ( 0.000000000000000000, -2.710505431213761085E-17, -55.00000000000000000 ) ) ;
#12306 = CIRCLE ( 'NONE', #806, 52.00000000000000711 ) ;
#12307 = VERTEX_POINT ( 'NONE', #34163 ) ;
#12308 = CARTESIAN_POINT ( 'NONE',  ( 7.999999999999992895, -46.77034588191288833, -22.72740077717277885 ) ) ;
#12309 = CARTESIAN_POINT ( 'NONE',  ( -34.50000000000000000, -114.8057644833805853, -2.624782352598442614 ) ) ;
#12310 = CARTESIAN_POINT ( 'NONE',  ( 46.00000000000000000, 0.000000000000000000, -11.00000000000000000 ) ) ;
#12311 = ORIENTED_EDGE ( 'NONE', *, *, #24960, .T. ) ;
#12312 = ORIENTED_EDGE ( 'NONE', *, *, #25817, .F. ) ;
#12313 = CARTESIAN_POINT ( 'NONE',  ( -36.64504884055821776, -112.9754527089670688, 9.715225545821551734 ) ) ;
#12314 = ADVANCED_FACE ( 'NONE', ( #3740 ), #15406, .T. ) ;
#12315 = ORIENTED_EDGE ( 'NONE', *, *, #15009, .T. ) ;
#12316 = EDGE_CURVE ( 'NONE', #26583, #24162, #4171, .T. ) ;
#12317 = ORIENTED_EDGE ( 'NONE', *, *, #5289, .T. ) ;
#12318 = ORIENTED_EDGE ( 'NONE', *, *, #27523, .T. ) ;
#12319 = CARTESIAN_POINT ( 'NONE',  ( -35.50000000000000000, -115.0140978167138712, -0.6247823525984407267 ) ) ;
#12320 = AXIS2_PLACEMENT_3D ( 'NONE', #31833, #34191, #23555 ) ;
#12321 = CIRCLE ( 'NONE', #11744, 52.00000000000000711 ) ;
#12322 = CARTESIAN_POINT ( 'NONE',  ( 8.000000000000000000, -17.47118961583598917, -0.9861715913089493801 ) ) ;
#12323 = DIRECTION ( 'NONE',  ( -1.000000000000000000, 0.000000000000000000, 0.000000000000000000 ) ) ;
#12324 = CARTESIAN_POINT ( 'NONE',  ( -35.96730626674924025, -114.9929510916434339, 13.11752178341330044 ) ) ;
#12325 = CARTESIAN_POINT ( 'NONE',  ( 4.000000000000003553, -39.64889472655708857, -33.64468972902551513 ) ) ;
#12326 = DIRECTION ( 'NONE',  ( -1.000000000000000000, 0.000000000000000000, -0.000000000000000000 ) ) ;
#12327 = EDGE_CURVE ( 'NONE', #1275, #24879, #12734, .T. ) ;
#12328 = CARTESIAN_POINT ( 'NONE',  ( -34.50000000000000000, -114.9929510916434339, 12.59102132592610523 ) ) ;
#12329 = CARTESIAN_POINT ( 'NONE',  ( 7.999999999999992895, -36.06787431788704623, 37.45808914225477793 ) ) ;
#12330 = CARTESIAN_POINT ( 'NONE',  ( 8.000000000000000000, -12.49559743815772528, -9.169462670380713831 ) ) ;
#12331 = ORIENTED_EDGE ( 'NONE', *, *, #383, .F. ) ;
#12332 = CARTESIAN_POINT ( 'NONE',  ( -35.50000000000000000, -115.9929510916434481, 12.44250253426871033 ) ) ;
#12333 = CARTESIAN_POINT ( 'NONE',  ( -35.50000000000000711, -115.8137639216009234, -1.239329810084483841 ) ) ;
#12334 = FACE_OUTER_BOUND ( 'NONE', #27825, .T. ) ;
#12335 = FACE_BOUND ( 'NONE', #12894, .T. ) ;
#12336 = CYLINDRICAL_SURFACE ( 'NONE', #11862, 7.020000000000045759 ) ;
#12337 = CARTESIAN_POINT ( 'NONE',  ( 7.999999999999992895, 51.85248208264524550, -3.914090171285633524 ) ) ;
#12338 = CIRCLE ( 'NONE', #15196, 8.000000000000008882 ) ;
#12339 = EDGE_CURVE ( 'NONE', #25964, #6849, #9905, .T. ) ;
#12340 = AXIS2_PLACEMENT_3D ( 'NONE', #14017, #30586, #30239 ) ;
#12341 = DIRECTION ( 'NONE',  ( 0.000000000000000000, 0.000000000000000000, -1.000000000000000000 ) ) ;
#12342 = CARTESIAN_POINT ( 'NONE',  ( 7.999999999999992895, 0.000000000000000000, 0.000000000000000000 ) ) ;
#12343 = ORIENTED_EDGE ( 'NONE', *, *, #14474, .T. ) ;
#12344 = EDGE_CURVE ( 'NONE', #21924, #35157, #15758, .T. ) ;
#12345 = ADVANCED_FACE ( 'NONE', ( #35071, #7668 ), #18477, .F. ) ;
#12346 = CARTESIAN_POINT ( 'NONE',  ( -37.74901162816868805, -113.3347980657955958, 7.933975545821553510 ) ) ;
#12347 = DIRECTION ( 'NONE',  ( -0.000000000000000000, -0.7535859266250379829, -0.6573494133204068612 ) ) ;
#12348 = DIRECTION ( 'NONE',  ( 9.266685234918781277E-17, -6.938893903907202493E-17, -1.000000000000000000 ) ) ;
#12349 = AXIS2_PLACEMENT_3D ( 'NONE', #30591, #11338, #22304 ) ;
#12350 = ORIENTED_EDGE ( 'NONE', *, *, #34791, .F. ) ;
#12351 = ORIENTED_EDGE ( 'NONE', *, *, #7661, .F. ) ;
#12352 = DIRECTION ( 'NONE',  ( -1.000000000000000000, 0.000000000000000000, 0.000000000000000000 ) ) ;
#12353 = ORIENTED_EDGE ( 'NONE', *, *, #17822, .F. ) ;
#12354 = CARTESIAN_POINT ( 'NONE',  ( -34.02454729103297382, -112.6980969099494132, 6.902725545821551734 ) ) ;
#12355 = EDGE_CURVE ( 'NONE', #31732, #12363, #21384, .T. ) ;
#12356 = ORIENTED_EDGE ( 'NONE', *, *, #19965, .T. ) ;
#12357 = EDGE_CURVE ( 'NONE', #25593, #4447, #24086, .T. ) ;
#12358 = CARTESIAN_POINT ( 'NONE',  ( 4.000000000000000000, 4.627536653468036720E-16, -46.00000000000000000 ) ) ;
#12359 = LINE ( 'NONE', #26410, #16578 ) ;
#12360 = CARTESIAN_POINT ( 'NONE',  ( 7.999999999999992895, 2.123073309835184830, 47.45152853935336168 ) ) ;
#12361 = CARTESIAN_POINT ( 'NONE',  ( 0.000000000000000000, 42.41764978026606059, -20.20639853260303198 ) ) ;
#12362 = ORIENTED_EDGE ( 'NONE', *, *, #21354, .T. ) ;
#12363 = VERTEX_POINT ( 'NONE', #4990 ) ;
#12364 = CIRCLE ( 'NONE', #2030, 0.04100000000000673939 ) ;
#12365 = AXIS2_PLACEMENT_3D ( 'NONE', #5705, #22251, #33250 ) ;
#12366 = CARTESIAN_POINT ( 'NONE',  ( 46.00000000000000000, 9.797174393178825657E-16, 8.000000000000000000 ) ) ;
#12367 = CARTESIAN_POINT ( 'NONE',  ( 3.800000000000018918, -1.719180353632054840E-14, -0.7999999999999996003 ) ) ;
#12368 = VERTEX_POINT ( 'NONE', #16291 ) ;
#12369 = CARTESIAN_POINT ( 'NONE',  ( -39.49999999999999289, -1.338792908815551458E-14, 114.0000000000000000 ) ) ;
#12370 = EDGE_CURVE ( 'NONE', #25880, #4840, #1885, .T. ) ;
#12371 = CARTESIAN_POINT ( 'NONE',  ( -34.50000000000000000, -112.0140900043112282, 0.8439677466545482121 ) ) ;
#12372 = DIRECTION ( 'NONE',  ( -1.000000000000000000, -1.734723475976807094E-16, -0.000000000000000000 ) ) ;
#12373 = CYLINDRICAL_SURFACE ( 'NONE', #24789, 13.99999999999999822 ) ;
#12374 = AXIS2_PLACEMENT_3D ( 'NONE', #17564, #22976, #11816 ) ;
#12375 = CARTESIAN_POINT ( 'NONE',  ( -34.50000306791346816, -115.9929510916434481, 12.62875129555796150 ) ) ;
#12376 = EDGE_CURVE ( 'NONE', #11899, #35547, #28881, .T. ) ;
#12377 = CARTESIAN_POINT ( 'NONE',  ( -42.49999999999999289, -18.77980021920990694, 100.4724318643354053 ) ) ;
#12378 = CARTESIAN_POINT ( 'NONE',  ( 0.000000000000000000, -2.710505431213761085E-17, 30.00000000000000000 ) ) ;
#12379 = EDGE_CURVE ( 'NONE', #35153, #31912, #26964, .T. ) ;
#12380 = CARTESIAN_POINT ( 'NONE',  ( -39.00000000000000711, -114.9929510916434339, 11.21034663311206181 ) ) ;
#12381 = CARTESIAN_POINT ( 'NONE',  ( -34.50000000000001421, -10.50833024919764469, 77.79903810567677169 ) ) ;
#12382 = DIRECTION ( 'NONE',  ( 0.000000000000000000, 0.000000000000000000, 1.000000000000000000 ) ) ;
#12383 = CARTESIAN_POINT ( 'NONE',  ( 2.000000000000001776, 0.000000000000000000, 0.000000000000000000 ) ) ;
#12384 = DIRECTION ( 'NONE',  ( 0.000000000000000000, 0.000000000000000000, -1.000000000000000000 ) ) ;
#12385 = APPLICATION_CONTEXT ( 'automotive_design' ) ;
#12386 = DIRECTION ( 'NONE',  ( 0.000000000000000000, 0.9510565162951521989, 0.3090169943749515036 ) ) ;
#12387 = ORIENTED_EDGE ( 'NONE', *, *, #34596, .F. ) ;
#12388 = EDGE_CURVE ( 'NONE', #16691, #29018, #32916, .T. ) ;
#12389 = CARTESIAN_POINT ( 'NONE',  ( -38.18337828418795965, -110.9754527089670546, 8.534774454178448266 ) ) ;
#12390 = EDGE_CURVE ( 'NONE', #35547, #11899, #6460, .T. ) ;
#12391 = CARTESIAN_POINT ( 'NONE',  ( 0.000000000000000000, 0.000000000000000000, -39.50000000000000711 ) ) ;
#12392 = CARTESIAN_POINT ( 'NONE',  ( -35.50000000000000000, -113.0140978167139991, -0.6247823525984269599 ) ) ;
#12393 = EDGE_LOOP ( 'NONE', ( #32335, #8512, #12801, #5940 ) ) ;
#12394 = ORIENTED_EDGE ( 'NONE', *, *, #28206, .T. ) ;
#12396 = DIRECTION ( 'NONE',  ( 0.000000000000000000, 0.000000000000000000, -1.000000000000000000 ) ) ;
#12395 = PRODUCT ( 'spur gear_iso_ISO - Spur gear 2M 12T 20PA 8FW ---S12A75H50L8.0S1', 'spur gear_iso_ISO - Spur gear 2M 12T 20PA 8FW ---S12A75H50L8.0S1', '', ( #14689 ) ) ;
#12397 = AXIS2_PLACEMENT_3D ( 'NONE', #30511, #22041, #16451 ) ;
#12398 = FACE_OUTER_BOUND ( 'NONE', #31871, .T. ) ;
#12399 = ORIENTED_EDGE ( 'NONE', *, *, #22440, .T. ) ;
#12400 = ORIENTED_EDGE ( 'NONE', *, *, #5952, .F. ) ;
#12401 = ORIENTED_EDGE ( 'NONE', *, *, #17864, .T. ) ;
#12402 = VECTOR ( 'NONE', #2629, 1000.000000000000000 ) ;
#12403 = ADVANCED_FACE ( 'NONE', ( #10561 ), #13443, .T. ) ;
#12404 = DIRECTION ( 'NONE',  ( -1.000000000000000000, 0.000000000000000000, 0.000000000000000000 ) ) ;
#12405 = CARTESIAN_POINT ( 'NONE',  ( -36.11231047232249836, -115.9754527089670262, 7.277725545821551734 ) ) ;
#12406 = DIRECTION ( 'NONE',  ( 0.000000000000000000, 0.000000000000000000, 1.000000000000000000 ) ) ;
#12408 = ORIENTED_EDGE ( 'NONE', *, *, #32954, .T. ) ;
#12407 = AXIS2_PLACEMENT_3D ( 'NONE', #3758, #20284, #25546 ) ;
#12409 = ORIENTED_EDGE ( 'NONE', *, *, #23489, .T. ) ;
#12410 = CARTESIAN_POINT ( 'NONE',  ( -35.50000000000000000, -114.1807644833817648, -2.624782352598442614 ) ) ;
#12411 = FACE_OUTER_BOUND ( 'NONE', #6866, .T. ) ;
#12412 = CARTESIAN_POINT ( 'NONE',  ( 7.999999999999992895, 5.667686777402359155, -46.64153600743598105 ) ) ;
#12413 = ORIENTED_EDGE ( 'NONE', *, *, #4280, .F. ) ;
#12414 = CARTESIAN_POINT ( 'NONE',  ( -38.00000000000000711, -114.9929510916434339, 12.17846912687782179 ) ) ;
#12415 = EDGE_CURVE ( 'NONE', #27904, #33894, #114, .T. ) ;
#12416 = EDGE_CURVE ( 'NONE', #25674, #7004, #18511, .T. ) ;
#12417 = CARTESIAN_POINT ( 'NONE',  ( -34.50000000000000000, -114.9929510916434339, 11.38636890470581164 ) ) ;
#12418 = AXIS2_PLACEMENT_3D ( 'NONE', #17510, #14452, #17870 ) ;
#12419 = CYLINDRICAL_SURFACE ( 'NONE', #24061, 47.49900000000001654 ) ;
#12420 = CARTESIAN_POINT ( 'NONE',  ( -37.37500000000009237, -114.9929510916434339, 13.11852480586264669 ) ) ;
#12421 = CARTESIAN_POINT ( 'NONE',  ( 0.000000000000000000, 0.000000000000000000, 0.000000000000000000 ) ) ;
#12422 = CARTESIAN_POINT ( 'NONE',  ( -36.87500000000098765, -113.9929510916434339, 14.11852480586265024 ) ) ;
#12423 = CARTESIAN_POINT ( 'NONE',  ( -4.000000000000000000, -2.710505431213761085E-17, -45.00000000000000000 ) ) ;
#12424 = CIRCLE ( 'NONE', #5548, 20.00000000000000355 ) ;
#12425 = AXIS2_PLACEMENT_3D ( 'NONE', #687, #21945, #30068 ) ;
#12426 = CARTESIAN_POINT ( 'NONE',  ( -37.34375000000001421, -114.9929510916434339, 13.11852480586264669 ) ) ;
#12427 = DIRECTION ( 'NONE',  ( -1.000000000000000000, 8.673617379883896189E-17, 1.502314598737167413E-16 ) ) ;
#12428 = ORIENTED_EDGE ( 'NONE', *, *, #9982, .F. ) ;
#12429 = CIRCLE ( 'NONE', #13588, 19.99999999999998579 ) ;
#12430 = DIRECTION ( 'NONE',  ( -1.000000000000000000, -0.000000000000000000, -0.000000000000000000 ) ) ;
#12431 = FACE_OUTER_BOUND ( 'NONE', #16458, .T. ) ;
#12432 = EDGE_LOOP ( 'NONE', ( #53, #23773 ) ) ;
#12433 = CARTESIAN_POINT ( 'NONE',  ( -35.50000000000000711, -114.9860996047076895, 10.38555023491505835 ) ) ;
#12434 = VERTEX_POINT ( 'NONE', #18299 ) ;
#12435 = CARTESIAN_POINT ( 'NONE',  ( -36.11231047232249125, -112.0245472910329880, 2.722274454178448266 ) ) ;
#12436 = AXIS2_PLACEMENT_3D ( 'NONE', #29662, #21900, #24620 ) ;
#12437 = EDGE_LOOP ( 'NONE', ( #27860, #32855, #3787, #16372 ) ) ;
#12438 = CARTESIAN_POINT ( 'NONE',  ( 46.00000000000000000, -25.98076211353320275, 84.99999999999992895 ) ) ;
#12439 = VERTEX_POINT ( 'NONE', #10741 ) ;
#12440 =( REPRESENTATION_RELATIONSHIP ('NONE','NONE', #26607, #8186 ) REPRESENTATION_RELATIONSHIP_WITH_TRANSFORMATION ( #16807 )SHAPE_REPRESENTATION_RELATIONSHIP( ) );
#12441 = CARTESIAN_POINT ( 'NONE',  ( -34.50000000000000000, -113.0140978167138996, -0.6247823525984302906 ) ) ;
#12442 = CARTESIAN_POINT ( 'NONE',  ( -1.799999999999995159, -5.412337245047654898E-16, -7.800000000000051337 ) ) ;
#12443 = FACE_OUTER_BOUND ( 'NONE', #19328, .T. ) ;
#12444 = ORIENTED_EDGE ( 'NONE', *, *, #22765, .T. ) ;
#12445 = CARTESIAN_POINT ( 'NONE',  ( -38.37230871539094323, -112.5438815906447729, 6.941024454178449155 ) ) ;
#12446 = DIRECTION ( 'NONE',  ( 0.000000000000000000, 0.000000000000000000, 1.000000000000000000 ) ) ;
#12447 = CARTESIAN_POINT ( 'NONE',  ( -35.50000000000000711, -114.6807644833805000, -1.624782352598427959 ) ) ;
#12448 = VERTEX_POINT ( 'NONE', #21708 ) ;
#12449 = ORIENTED_EDGE ( 'NONE', *, *, #33171, .T. ) ;
#12450 = CARTESIAN_POINT ( 'NONE',  ( 0.000000000000000000, 0.000000000000000000, 65.00000000000000000 ) ) ;
#12451 = COLOUR_RGB ( '', 0.40784314, 0.44705882, 0.49803922) ;
#12452 = AXIS2_PLACEMENT_3D ( 'NONE', #35426, #10757, #8738 ) ;
#12453 = FILL_AREA_STYLE ('',( #4364 ) ) ;
#12454 = DIRECTION ( 'NONE',  ( -1.000000000000000000, 0.000000000000000000, 0.000000000000000000 ) ) ;
#12455 = ORIENTED_EDGE ( 'NONE', *, *, #544, .F. ) ;
#12456 = ORIENTED_EDGE ( 'NONE', *, *, #275, .T. ) ;
#12457 = CARTESIAN_POINT ( 'NONE',  ( -34.50000000000000000, -116.0140978167138712, 0.6252176474015648244 ) ) ;
#12458 = AXIS2_PLACEMENT_3D ( 'NONE', #29990, #32323, #10905 ) ;
#12459 = CARTESIAN_POINT ( 'NONE',  ( -35.50000000000000711, -114.0000000000000853, 2.000000000000001776 ) ) ;
#12460 = AXIS2_PLACEMENT_3D ( 'NONE', #13626, #24618, #17013 ) ;
#12461 = LINE ( 'NONE', #4372, #9290 ) ;
#12462 = ORIENTED_EDGE ( 'NONE', *, *, #16722, .F. ) ;
#12463 = EDGE_LOOP ( 'NONE', ( #25660, #3638 ) ) ;
#12464 = DIRECTION ( 'NONE',  ( 0.000000000000000000, 0.5000000000000011102, -0.8660254037844380415 ) ) ;
#12465 = CIRCLE ( 'NONE', #13071, 19.99999999999998579 ) ;
#12466 = EDGE_CURVE ( 'NONE', #27894, #3460, #32785, .T. ) ;
#12467 = CARTESIAN_POINT ( 'NONE',  ( -37.62959469683911351, -113.9929510916434339, 13.10254527216511633 ) ) ;
#12468 = CARTESIAN_POINT ( 'NONE',  ( 4.000000000000003553, -44.25018368420724357, -27.31155879685229237 ) ) ;
#12469 = CARTESIAN_POINT ( 'NONE',  ( -35.50000000000000000, -113.9929510916434339, 12.59102132592610346 ) ) ;
#12470 = AXIS2_PLACEMENT_3D ( 'NONE', #34130, #20412, #15917 ) ;
#12471 = CARTESIAN_POINT ( 'NONE',  ( -35.60016694755736211, -115.9929510916434481, 12.92579853460621386 ) ) ;
#12472 = VECTOR ( 'NONE', #2316, 1000.000000000000000 ) ;
#12473 = LINE ( 'NONE', #28857, #11820 ) ;
#12474 = CYLINDRICAL_SURFACE ( 'NONE', #29041, 20.00000000000000711 ) ;
#12475 = CIRCLE ( 'NONE', #28591, 3.799999999999999822 ) ;
#12476 = ORIENTED_EDGE ( 'NONE', *, *, #18756, .F. ) ;
#12477 = DIRECTION ( 'NONE',  ( 0.000000000000000000, -1.067522139062650474E-15, -1.000000000000000000 ) ) ;
#12478 = DIRECTION ( 'NONE',  ( 0.000000000000000000, 0.000000000000000000, -1.000000000000000000 ) ) ;
#12479 = LINE ( 'NONE', #25989, #32966 ) ;
#12480 =( GEOMETRIC_REPRESENTATION_CONTEXT ( 3 ) GLOBAL_UNCERTAINTY_ASSIGNED_CONTEXT ( ( #16835 ) ) GLOBAL_UNIT_ASSIGNED_CONTEXT ( ( #29362, #21045, #26483 ) ) REPRESENTATION_CONTEXT ( 'NONE', 'WORKASPACE' ) );
#12481 = CIRCLE ( 'NONE', #16470, 4.800000000000006040 ) ;
#12482 = EDGE_LOOP ( 'NONE', ( #11374, #11257, #10372, #19567 ) ) ;
#12483 = VECTOR ( 'NONE', #34815, 1000.000000000000000 ) ;
#12484 = DIRECTION ( 'NONE',  ( 0.000000000000000000, 0.9822872507286892763, -0.1873813145857214646 ) ) ;
#12485 = CARTESIAN_POINT ( 'NONE',  ( -35.50000000000000711, -114.3474311500471430, -1.624782352598427959 ) ) ;
#12486 = CARTESIAN_POINT ( 'NONE',  ( -2.000000000000001776, 0.000000000000000000, 0.000000000000000000 ) ) ;
#12487 = VECTOR ( 'NONE', #10417, 1000.000000000000000 ) ;
#12488 = CARTESIAN_POINT ( 'NONE',  ( 8.000000000000000000, 0.000000000000000000, 0.000000000000000000 ) ) ;
#12489 = LINE ( 'NONE', #9784, #17630 ) ;
#12490 = ORIENTED_EDGE ( 'NONE', *, *, #14695, .F. ) ;
#12491 = CARTESIAN_POINT ( 'NONE',  ( 0.000000000000000000, 49.25004636492413823, -16.68630974939705425 ) ) ;
#12492 = CARTESIAN_POINT ( 'NONE',  ( -34.50000000000000000, -117.0140978167138854, 0.0002176474015577929428 ) ) ;
#12493 = CARTESIAN_POINT ( 'NONE',  ( 9.714451465470119729E-14, 0.9999999999999870104, 45.00000000000000711 ) ) ;
#12494 = ORIENTED_EDGE ( 'NONE', *, *, #27762, .T. ) ;
#12495 = ORIENTED_EDGE ( 'NONE', *, *, #6406, .T. ) ;
#12496 = CARTESIAN_POINT ( 'NONE',  ( -36.33479806579561000, -114.7490116281687165, 3.191024454178448710 ) ) ;
#12497 = VECTOR ( 'NONE', #10357, 1000.000000000000114 ) ;
#12498 = ORIENTED_EDGE ( 'NONE', *, *, #32968, .F. ) ;
#12499 = ORIENTED_EDGE ( 'NONE', *, *, #6635, .T. ) ;
#12500 = CARTESIAN_POINT ( 'NONE',  ( -35.50000000000000000, -113.0974311500471714, -0.6247823525984269599 ) ) ;
#12501 = AXIS2_PLACEMENT_3D ( 'NONE', #12738, #29484, #20632 ) ;
#12502 = DIRECTION ( 'NONE',  ( -1.000000000000000000, 0.000000000000000000, -0.000000000000000000 ) ) ;
#12503 = VECTOR ( 'NONE', #15410, 1000.000000000000000 ) ;
#12504 = CIRCLE ( 'NONE', #22845, 8.000000000000007105 ) ;
#12505 = DIRECTION ( 'NONE',  ( 0.000000000000000000, 0.000000000000000000, 1.000000000000000000 ) ) ;
#12506 = AXIS2_PLACEMENT_3D ( 'NONE', #5942, #19445, #25031 ) ;
#12507 = EDGE_CURVE ( 'NONE', #4187, #4766, #18976, .T. ) ;
#12508 = CARTESIAN_POINT ( 'NONE',  ( -36.03125000000004263, -114.9929510916434339, 13.11852480586264669 ) ) ;
#12509 = CARTESIAN_POINT ( 'NONE',  ( 8.000000000000000000, 8.128228055638880178, 16.94522934049213347 ) ) ;
#12510 = ADVANCED_FACE ( 'NONE', ( #34886 ), #27305, .T. ) ;
#12511 = AXIS2_PLACEMENT_3D ( 'NONE', #10545, #35585, #10909 ) ;
#12512 = CARTESIAN_POINT ( 'NONE',  ( -35.24442919769869320, -114.9929510916434339, 13.92914543265605509 ) ) ;
#12513 = CARTESIAN_POINT ( 'NONE',  ( 7.999999999999992895, 38.92705108641732892, 27.21837053747812263 ) ) ;
#12514 = UNCERTAINTY_MEASURE_WITH_UNIT (LENGTH_MEASURE( 1.000000000000000082E-05 ), #1096, 'distance_accuracy_value', 'NONE');
#12515 = CARTESIAN_POINT ( 'NONE',  ( 7.999999999999992895, 42.41764978026606769, 20.20639853260304619 ) ) ;
#12516 = ORIENTED_EDGE ( 'NONE', *, *, #1409, .F. ) ;
#12517 = EDGE_CURVE ( 'NONE', #7610, #34437, #23578, .T. ) ;
#12518 = CARTESIAN_POINT ( 'NONE',  ( -35.49999931242378182, -115.9929510916434481, 12.61439929482945743 ) ) ;
#12519 = CARTESIAN_POINT ( 'NONE',  ( -35.50000000000000711, -116.0140978167138712, -0.5622823525984409487 ) ) ;
#12520 = SURFACE_STYLE_USAGE ( .BOTH. , #20411 ) ;
#12521 = FACE_OUTER_BOUND ( 'NONE', #24417, .T. ) ;
#12522 = FACE_OUTER_BOUND ( 'NONE', #12716, .T. ) ;
#12523 = AXIS2_PLACEMENT_3D ( 'NONE', #28503, #30680, #25093 ) ;
#12524 = FACE_OUTER_BOUND ( 'NONE', #20120, .T. ) ;
#12525 = CARTESIAN_POINT ( 'NONE',  ( 8.000000000000007105, 0.000000000000000000, 0.000000000000000000 ) ) ;
#12526 = CIRCLE ( 'NONE', #17103, 0.5000000000000004441 ) ;
#12527 = CARTESIAN_POINT ( 'NONE',  ( -6.896599878636569869, -12.98179148322720167, -1.200000000000006617 ) ) ;
#12528 = CARTESIAN_POINT ( 'NONE',  ( 0.3000000000000016542, -14.69693845669907439, 0.000000000000000000 ) ) ;
#12529 = ORIENTED_EDGE ( 'NONE', *, *, #34154, .T. ) ;
#12530 = AXIS2_PLACEMENT_3D ( 'NONE', #31855, #28809, #18352 ) ;
#12531 = CARTESIAN_POINT ( 'NONE',  ( -37.74901162816868805, -113.3347980657955958, 9.433975545821549957 ) ) ;
#12532 = FACE_OUTER_BOUND ( 'NONE', #8630, .T. ) ;
#12533 = CIRCLE ( 'NONE', #30355, 4.000000000000000000 ) ;
#12534 = DIRECTION ( 'NONE',  ( -1.000000000000000000, 0.000000000000000000, 0.000000000000000000 ) ) ;
#12535 = ORIENTED_EDGE ( 'NONE', *, *, #5088, .F. ) ;
#12536 = ORIENTED_EDGE ( 'NONE', *, *, #7507, .F. ) ;
#12537 = AXIS2_PLACEMENT_3D ( 'NONE', #20836, #25309, #8586 ) ;
#12538 = CARTESIAN_POINT ( 'NONE',  ( 8.000000000000000000, 6.860320204751340079, -13.89802171851375689 ) ) ;
#12539 = DIRECTION ( 'NONE',  ( 0.000000000000000000, 0.3420201433256629953, 0.9396926207859105373 ) ) ;
#12540 = EDGE_LOOP ( 'NONE', ( #14344, #445, #6103, #33565 ) ) ;
#12541 = CARTESIAN_POINT ( 'NONE',  ( -34.00000000000000000, -113.9407375970686758, 5.496475545821551734 ) ) ;
#12542 = ORIENTED_EDGE ( 'NONE', *, *, #26421, .T. ) ;
#12543 = CIRCLE ( 'NONE', #34398, 7.199999999999994849 ) ;
#12544 = EDGE_CURVE ( 'NONE', #18180, #6280, #8638, .T. ) ;
#12545 = CARTESIAN_POINT ( 'NONE',  ( 0.000000000000000000, 0.000000000000000000, 0.000000000000000000 ) ) ;
#12546 = ORIENTED_EDGE ( 'NONE', *, *, #24656, .T. ) ;
#12547 = DIRECTION ( 'NONE',  ( -1.000000000000000000, -0.000000000000000000, -0.000000000000000000 ) ) ;
#12548 = CARTESIAN_POINT ( 'NONE',  ( 4.000000000000000000, 4.898587196589412829E-16, 65.00000000000000000 ) ) ;
#12549 = CARTESIAN_POINT ( 'NONE',  ( 5.400000000000003020, 1.000000000000000888, -22.00000000000000000 ) ) ;
#12550 = ORIENTED_EDGE ( 'NONE', *, *, #13609, .T. ) ;
#12551 = ORIENTED_EDGE ( 'NONE', *, *, #33117, .F. ) ;
#12552 = EDGE_CURVE ( 'NONE', #28129, #18999, #24956, .T. ) ;
#12553 = CARTESIAN_POINT ( 'NONE',  ( 70.00000600000001327, -25.98076211353320986, 88.99999999999994316 ) ) ;
#12554 = CARTESIAN_POINT ( 'NONE',  ( 7.999999999999992895, 41.20225022064637699, 23.63323037071417332 ) ) ;
#12555 = EDGE_CURVE ( 'NONE', #25713, #28225, #2914, .T. ) ;
#12556 = EDGE_CURVE ( 'NONE', #31962, #26553, #16475, .T. ) ;
#12557 = ORIENTED_EDGE ( 'NONE', *, *, #32459, .T. ) ;
#12558 = DIRECTION ( 'NONE',  ( 0.000000000000000000, 0.000000000000000000, 1.000000000000000000 ) ) ;
#12559 = DIRECTION ( 'NONE',  ( -1.000000000000000000, -0.000000000000000000, -0.000000000000000000 ) ) ;
#12560 = DIRECTION ( 'NONE',  ( -1.000000000000000000, -0.000000000000000000, -0.000000000000000000 ) ) ;
#12561 = CIRCLE ( 'NONE', #15414, 22.00000000000000000 ) ;
#12562 = CARTESIAN_POINT ( 'NONE',  ( -34.51202277066418844, -115.9929510916434481, 12.81430620224972294 ) ) ;
#12563 = DIRECTION ( 'NONE',  ( 1.000000000000000000, -5.339440136655842133E-16, -1.047965281155519420E-16 ) ) ;
#12564 = CARTESIAN_POINT ( 'NONE',  ( -36.11231047232249836, -112.0245472910329880, 2.722274454178448710 ) ) ;
#12565 = ADVANCED_FACE ( 'NONE', ( #30363, #279 ), #33573, .F. ) ;
#12566 = CARTESIAN_POINT ( 'NONE',  ( -34.80050084267116972, -115.9929510916434481, 13.54034599209289347 ) ) ;
#12567 = CARTESIAN_POINT ( 'NONE',  ( -34.49999999999998579, -20.32009476567239048, 97.80456345124112261 ) ) ;
#12568 = VECTOR ( 'NONE', #30557, 1000.000000000000000 ) ;
#12569 = EDGE_CURVE ( 'NONE', #1645, #10783, #24179, .T. ) ;
#12570 = DIRECTION ( 'NONE',  ( 1.000000000000000000, -0.000000000000000000, 0.000000000000000000 ) ) ;
#12571 = DIRECTION ( 'NONE',  ( 0.000000000000000000, 0.000000000000000000, -1.000000000000000000 ) ) ;
#12572 = CYLINDRICAL_SURFACE ( 'NONE', #26150, 4.000000000000000000 ) ;
#12573 = CYLINDRICAL_SURFACE ( 'NONE', #2119, 0.9999999999999974465 ) ;
#12574 = FACE_OUTER_BOUND ( 'NONE', #28922, .T. ) ;
#12575 = ORIENTED_EDGE ( 'NONE', *, *, #6007, .T. ) ;
#12576 = CARTESIAN_POINT ( 'NONE',  ( -38.18337828418796676, -117.0245472910329738, 5.965225545821550845 ) ) ;
#12577 = LINE ( 'NONE', #24104, #34798 ) ;
#12578 = CARTESIAN_POINT ( 'NONE',  ( -35.50000000000000000, -113.0601156079281253, 0.8807106166081309917 ) ) ;
#12579 = ORIENTED_EDGE ( 'NONE', *, *, #4454, .F. ) ;
#12580 = ORIENTED_EDGE ( 'NONE', *, *, #16775, .F. ) ;
#12581 = DIRECTION ( 'NONE',  ( 1.000000000000000000, 0.000000000000000000, 0.000000000000000000 ) ) ;
#12582 = DIRECTION ( 'NONE',  ( 1.110223024625156540E-16, 1.000000000000000000, 0.000000000000000000 ) ) ;
#12583 = EDGE_LOOP ( 'NONE', ( #33053, #27784, #14832, #5589 ) ) ;
#12584 = ORIENTED_EDGE ( 'NONE', *, *, #20902, .F. ) ;
#12585 = ORIENTED_EDGE ( 'NONE', *, *, #7577, .T. ) ;
#12586 = AXIS2_PLACEMENT_3D ( 'NONE', #32267, #32439, #10658 ) ;
#12587 = ADVANCED_FACE ( 'NONE', ( #27666 ), #10306, .F. ) ;
#12588 = AXIS2_PLACEMENT_3D ( 'NONE', #20590, #31938, #10157 ) ;
#12589 = DIRECTION ( 'NONE',  ( -1.226634733346698078E-16, 0.2588190451025185190, 0.9659258262890689783 ) ) ;
#12590 = PRODUCT_RELATED_PRODUCT_CATEGORY ( 'part', '', ( #4077 ) ) ;
#12591 = FACE_OUTER_BOUND ( 'NONE', #9697, .T. ) ;
#12592 = ADVANCED_FACE ( 'NONE', ( #35125 ), #21574, .T. ) ;
#12593 = CARTESIAN_POINT ( 'NONE',  ( 48.00000000000000000, -25.98076211353320986, 84.99999999999992895 ) ) ;
#12594 = CARTESIAN_POINT ( 'NONE',  ( 7.999999999999992895, 0.000000000000000000, 0.000000000000000000 ) ) ;
#12595 = ORIENTED_EDGE ( 'NONE', *, *, #478, .F. ) ;
#12596 = ORIENTED_EDGE ( 'NONE', *, *, #32840, .T. ) ;
#12597 = CARTESIAN_POINT ( 'NONE',  ( -35.50000000000000000, -114.6807644833805000, -2.624782352598442614 ) ) ;
#12598 = DIRECTION ( 'NONE',  ( -1.000000000000000000, -0.000000000000000000, -0.000000000000000000 ) ) ;
#12599 = EDGE_CURVE ( 'NONE', #15022, #17024, #1633, .T. ) ;
#12600 = EDGE_CURVE ( 'NONE', #22531, #17419, #28989, .T. ) ;
#12601 = CARTESIAN_POINT ( 'NONE',  ( 8.000000000000000000, -17.47118961583602470, 0.9861715913087032437 ) ) ;
#12602 = VERTEX_POINT ( 'NONE', #15283 ) ;
#12603 = CARTESIAN_POINT ( 'NONE',  ( 0.000000000000000000, 0.000000000000000000, -53.39999999999999858 ) ) ;
#12604 = CARTESIAN_POINT ( 'NONE',  ( -34.50000000000000000, -114.6604609523327838, 9.751889438017201428 ) ) ;
#12605 = CARTESIAN_POINT ( 'NONE',  ( -1.519999999999993578, 6.984000000000004427, -4.163336342344337027E-14 ) ) ;
#12606 = AXIS2_PLACEMENT_3D ( 'NONE', #33402, #8725, #30535 ) ;
#12607 = CARTESIAN_POINT ( 'NONE',  ( -37.56526046546250086, -114.9929510916434339, 13.11451721564129258 ) ) ;
#12608 = DIRECTION ( 'NONE',  ( 0.000000000000000000, 0.000000000000000000, 1.000000000000000000 ) ) ;
#12609 = CARTESIAN_POINT ( 'NONE',  ( -34.50000000000000000, -114.0650276068786582, 9.507762098804159123 ) ) ;
#12610 = DIRECTION ( 'NONE',  ( -1.000000000000000000, 0.000000000000000000, 0.000000000000000000 ) ) ;
#12611 = EDGE_CURVE ( 'NONE', #1909, #23255, #12788, .T. ) ;
#12612 = CARTESIAN_POINT ( 'NONE',  ( 0.000000000000000000, 35.20873326984081331, 31.88259874184044662 ) ) ;
#12613 = SURFACE_SIDE_STYLE ('',( #18174 ) ) ;
#12614 = EDGE_LOOP ( 'NONE', ( #15302, #1647, #16182, #24021 ) ) ;
#12615 = CYLINDRICAL_SURFACE ( 'NONE', #890, 7.199999999999993960 ) ;
#12616 = DIRECTION ( 'NONE',  ( 0.000000000000000000, -0.9848077530122092416, 0.1736481776669233923 ) ) ;
#12617 = ORIENTED_EDGE ( 'NONE', *, *, #24673, .T. ) ;
#12618 = CARTESIAN_POINT ( 'NONE',  ( -35.50025087934803736, -114.9929510916434339, 12.63488142334835196 ) ) ;
#12619 = ORIENTED_EDGE ( 'NONE', *, *, #13652, .F. ) ;
#12620 = CIRCLE ( 'NONE', #23530, 7.020000000000045759 ) ;
#12621 = CARTESIAN_POINT ( 'NONE',  ( -35.54388159064475872, -112.6276912846090568, 2.816024454178448710 ) ) ;
#12622 = DIRECTION ( 'NONE',  ( 0.000000000000000000, 0.000000000000000000, 1.000000000000000000 ) ) ;
#12623 = ORIENTED_EDGE ( 'NONE', *, *, #16121, .F. ) ;
#12624 = CARTESIAN_POINT ( 'NONE',  ( 8.000000000000000000, 3.678165988948789877, -15.05623113391063406 ) ) ;
#12625 = ORIENTED_EDGE ( 'NONE', *, *, #17612, .F. ) ;
#12626 = CARTESIAN_POINT ( 'NONE',  ( -34.50000000000000000, -113.0140978167141128, -0.6247823525984907977 ) ) ;
#12627 = DIRECTION ( 'NONE',  ( 0.000000000000000000, 0.000000000000000000, -1.000000000000000000 ) ) ;
#12628 = CARTESIAN_POINT ( 'NONE',  ( -37.05926240293131713, -115.9999999999999858, 7.878524454178450043 ) ) ;
#12629 = VERTEX_POINT ( 'NONE', #12612 ) ;
#12630 = CARTESIAN_POINT ( 'NONE',  ( -38.30190309005061522, -116.9754527089670546, 3.472274454178448710 ) ) ;
#12631 = EDGE_CURVE ( 'NONE', #15081, #8016, #33345, .T. ) ;
#12632 = EDGE_CURVE ( 'NONE', #8203, #5984, #24132, .T. ) ;
#12633 = CARTESIAN_POINT ( 'NONE',  ( 0.000000000000000000, 10.15474465512070168, -9.637487275700989287 ) ) ;
#12634 = CARTESIAN_POINT ( 'NONE',  ( -35.50000000000000711, -112.0140978167138712, 0.3752176474015640473 ) ) ;
#12635 = VERTEX_POINT ( 'NONE', #32405 ) ;
#12637 = ORIENTED_EDGE ( 'NONE', *, *, #10768, .T. ) ;
#12636 = EDGE_CURVE ( 'NONE', #1779, #1275, #15515, .T. ) ;
#12638 = CARTESIAN_POINT ( 'NONE',  ( 0.000000000000000000, 7.613867765417669631, 5.679790370316101011 ) ) ;
#12639 = VECTOR ( 'NONE', #20225, 1000.000000000000000 ) ;
#12640 = CARTESIAN_POINT ( 'NONE',  ( 8.000000000000000000, 15.92965478239619515, 15.17386234660388666 ) ) ;
#12641 = ORIENTED_EDGE ( 'NONE', *, *, #29358, .F. ) ;
#12642 = ORIENTED_EDGE ( 'NONE', *, *, #10848, .T. ) ;
#12643 = AXIS2_PLACEMENT_3D ( 'NONE', #17802, #31147, #1086 ) ;
#12644 = CARTESIAN_POINT ( 'NONE',  ( -34.50000000000000000, -115.9821387493194891, -0.8839717462762166633 ) ) ;
#12645 = DIRECTION ( 'NONE',  ( 1.000000000000000000, 0.000000000000000000, -0.000000000000000000 ) ) ;
#12646 = EDGE_CURVE ( 'NONE', #4835, #26059, #21939, .T. ) ;
#12647 = DIRECTION ( 'NONE',  ( -1.000000000000000000, 0.000000000000000000, 0.000000000000000000 ) ) ;
#12648 = AXIS2_PLACEMENT_3D ( 'NONE', #32719, #476, #16310 ) ;
#12649 = AXIS2_PLACEMENT_3D ( 'NONE', #33842, #139, #314 ) ;
#12650 = VERTEX_POINT ( 'NONE', #5402 ) ;
#12651 = VERTEX_POINT ( 'NONE', #21758 ) ;
#12652 = EDGE_CURVE ( 'NONE', #28118, #27575, #16879, .T. ) ;
#12653 = AXIS2_PLACEMENT_3D ( 'NONE', #10961, #21747, #7711 ) ;
#12654 = CARTESIAN_POINT ( 'NONE',  ( 65.00000000000001421, -27.28312344603513040, 77.61394185240837373 ) ) ;
#12655 = CARTESIAN_POINT ( 'NONE',  ( -34.50000000000000000, -113.9929510916430075, 10.50625754673586876 ) ) ;
#12656 = FACE_OUTER_BOUND ( 'NONE', #17600, .T. ) ;
#12657 = CARTESIAN_POINT ( 'NONE',  ( -36.62499999999902656, -113.9929510916434339, 13.11852480586264846 ) ) ;
#12658 = CARTESIAN_POINT ( 'NONE',  ( -37.80727372874345349, -115.9929510916434481, 13.01835785830664705 ) ) ;
#12659 = FACE_OUTER_BOUND ( 'NONE', #23340, .T. ) ;
#12660 = DIRECTION ( 'NONE',  ( -0.000000000000000000, -0.000000000000000000, -1.000000000000000000 ) ) ;
#12661 = ORIENTED_EDGE ( 'NONE', *, *, #4568, .T. ) ;
#12662 = AXIS2_PLACEMENT_3D ( 'NONE', #4072, #26190, #18072 ) ;
#12663 = CARTESIAN_POINT ( 'NONE',  ( -9.999999999999994671, 0.000000000000000000, 0.000000000000000000 ) ) ;
#12664 = CARTESIAN_POINT ( 'NONE',  ( 8.000000000000007105, -13.61301047812919762, 3.268936481846118625 ) ) ;
#12665 = DIRECTION ( 'NONE',  ( 1.000000000000000000, 0.000000000000000000, 0.000000000000000000 ) ) ;
#12666 = ORIENTED_EDGE ( 'NONE', *, *, #11297, .T. ) ;
#12667 = CIRCLE ( 'NONE', #35115, 47.49900000000002365 ) ;
#12668 = DIRECTION ( 'NONE',  ( 0.000000000000000000, 0.000000000000000000, 1.000000000000000000 ) ) ;
#12669 = CARTESIAN_POINT ( 'NONE',  ( -35.50000000000000711, -112.7765286249690035, 1.847058736912741583 ) ) ;
#12670 = CARTESIAN_POINT ( 'NONE',  ( -34.49999999999998579, -24.48076211353329157, 98.91941090707499029 ) ) ;
#12671 = FACE_OUTER_BOUND ( 'NONE', #4934, .T. ) ;
#12672 = AXIS2_PLACEMENT_3D ( 'NONE', #14630, #6365, #3333 ) ;
#12673 = VECTOR ( 'NONE', #8626, 1000.000000000000000 ) ;
#12674 = CIRCLE ( 'NONE', #32791, 52.00000000000000711 ) ;
#12675 = CARTESIAN_POINT ( 'NONE',  ( -35.50000000000000711, -114.0371586325023117, 9.504435485030890973 ) ) ;
#12676 = FACE_BOUND ( 'NONE', #5515, .T. ) ;
#12677 = ORIENTED_EDGE ( 'NONE', *, *, #19432, .F. ) ;
#12678 = ADVANCED_FACE ( 'NONE', ( #16348 ), #19231, .T. ) ;
#12679 = DIRECTION ( 'NONE',  ( 0.000000000000000000, 0.000000000000000000, 1.000000000000000000 ) ) ;
#12680 = CARTESIAN_POINT ( 'NONE',  ( -34.50000000000000000, -111.0397324434303101, -0.9506101647064429949 ) ) ;
#12681 = CYLINDRICAL_SURFACE ( 'NONE', #5949, 0.7500000000000006661 ) ;
#12682 = ORIENTED_EDGE ( 'NONE', *, *, #34440, .F. ) ;
#12683 = VERTEX_POINT ( 'NONE', #7906 ) ;
#12684 = CARTESIAN_POINT ( 'NONE',  ( -37.66520193420439000, -113.2509883718312977, 5.441024454178449155 ) ) ;
#12685 = ORIENTED_EDGE ( 'NONE', *, *, #3578, .F. ) ;
#12686 = ORIENTED_EDGE ( 'NONE', *, *, #5934, .F. ) ;
#12687 = CARTESIAN_POINT ( 'NONE',  ( -35.50000000000000000, -115.0140978167138712, 0.6252176474015650465 ) ) ;
#12688 = LINE ( 'NONE', #20761, #28681 ) ;
#12689 = CARTESIAN_POINT ( 'NONE',  ( 39.30000000000000426, -10.49999999999999112, 0.000000000000000000 ) ) ;
#12690 = AXIS2_PLACEMENT_3D ( 'NONE', #6442, #858, #8958 ) ;
#12691 = CARTESIAN_POINT ( 'NONE',  ( -37.99959864031215773, -114.9929510916434339, 12.63896776382213538 ) ) ;
#12692 = DIRECTION ( 'NONE',  ( 1.000000000000000000, -0.000000000000000000, -0.000000000000000000 ) ) ;
#12693 = AXIS2_PLACEMENT_3D ( 'NONE', #34813, #15340, #21102 ) ;
#12694 = CIRCLE ( 'NONE', #10415, 4.800000000000000711 ) ;
#12695 = CARTESIAN_POINT ( 'NONE',  ( -34.50300906734827322, -114.9929510916434339, 12.71660600561482468 ) ) ;
#12696 = LINE ( 'NONE', #4607, #24910 ) ;
#12697 = PRODUCT_DEFINITION_SHAPE ( 'NONE', 'NONE',  #22682 ) ;
#12698 = CYLINDRICAL_SURFACE ( 'NONE', #16308, 47.49900000000001654 ) ;
#12699 = VERTEX_POINT ( 'NONE', #10975 ) ;
#12700 = CARTESIAN_POINT ( 'NONE',  ( -35.99386409314529800, -115.9929510916434481, 13.11852378322482515 ) ) ;
#12701 = CARTESIAN_POINT ( 'NONE',  ( -35.50000000000000711, -113.1807644833805426, -1.624782352598427959 ) ) ;
#12702 =( NAMED_UNIT ( * ) PLANE_ANGLE_UNIT ( ) SI_UNIT ( $, .RADIAN. ) );
#12703 = LINE ( 'NONE', #7290, #13049 ) ;
#12704 = DIRECTION ( 'NONE',  ( 0.000000000000000000, -0.4999999999999928946, -0.8660254037844427044 ) ) ;
#12705 = ORIENTED_EDGE ( 'NONE', *, *, #5977, .F. ) ;
#12706 = CARTESIAN_POINT ( 'NONE',  ( -44.00000000000000000, 10.58300524425835398, 3.000000000000002665 ) ) ;
#12707 = DIRECTION ( 'NONE',  ( -1.000000000000000000, 0.000000000000000000, 0.000000000000000000 ) ) ;
#12708 = CARTESIAN_POINT ( 'NONE',  ( 50.00005079999998969, 14.30000000000000071, -3.000000000000002665 ) ) ;
#12709 = CARTESIAN_POINT ( 'NONE',  ( 9.714451465470119729E-14, 0.9999999999999870104, -32.00000000000000000 ) ) ;
#12710 = ORIENTED_EDGE ( 'NONE', *, *, #20745, .T. ) ;
#12711 = AXIS2_PLACEMENT_3D ( 'NONE', #26783, #23351, #7146 ) ;
#12712 = CARTESIAN_POINT ( 'NONE',  ( -35.99999999999999289, -114.0592624029313242, 3.003524454178448710 ) ) ;
#12713 = FACE_OUTER_BOUND ( 'NONE', #22053, .T. ) ;
#12714 = CARTESIAN_POINT ( 'NONE',  ( -42.49999999999999289, -29.98076211353321341, 84.99999999999994316 ) ) ;
#12715 = VERTEX_POINT ( 'NONE', #22294 ) ;
#12716 = EDGE_LOOP ( 'NONE', ( #17306, #23208, #23005, #24943 ) ) ;
#12717 = EDGE_CURVE ( 'NONE', #4367, #34778, #12667, .T. ) ;
#12718 =( NAMED_UNIT ( * ) SI_UNIT ( $, .STERADIAN. ) SOLID_ANGLE_UNIT ( ) );
#12719 = FACE_OUTER_BOUND ( 'NONE', #34783, .T. ) ;
#12720 = ORIENTED_EDGE ( 'NONE', *, *, #14319, .F. ) ;
#12721 = CARTESIAN_POINT ( 'NONE',  ( -38.97545270896704039, -114.8876895276775087, 3.152725545821551290 ) ) ;
#12722 = EDGE_LOOP ( 'NONE', ( #11465, #3603, #5222, #31894 ) ) ;
#12723 = AXIS2_PLACEMENT_3D ( 'NONE', #26898, #1111, #19800 ) ;
#12724 = AXIS2_PLACEMENT_3D ( 'NONE', #10780, #21742, #5555 ) ;
#12725 = DIRECTION ( 'NONE',  ( 0.000000000000000000, 0.000000000000000000, 1.000000000000000000 ) ) ;
#12726 = VERTEX_POINT ( 'NONE', #2712 ) ;
#12727 = EDGE_LOOP ( 'NONE', ( #28179, #26141, #22339, #13080 ) ) ;
#12728 = CARTESIAN_POINT ( 'NONE',  ( 0.000000000000000000, -9.744342220503712682, 46.48873837489796301 ) ) ;
#12729 = CARTESIAN_POINT ( 'NONE',  ( 8.000000000000000000, -8.931325931664709117, 16.53603053422203573 ) ) ;
#12730 = EDGE_CURVE ( 'NONE', #4610, #169, #11496, .T. ) ;
#12731 = CARTESIAN_POINT ( 'NONE',  ( -90.00000000000002842, 1.297889732222515536E-15, 6.765000000000052083 ) ) ;
#12732 = ORIENTED_EDGE ( 'NONE', *, *, #30751, .T. ) ;
#12733 = ORIENTED_EDGE ( 'NONE', *, *, #20910, .F. ) ;
#12734 = LINE ( 'NONE', #12016, #19100 ) ;
#12735 = CARTESIAN_POINT ( 'NONE',  ( 0.000000000000000000, -3.975523202428068892, 13.42368113696675103 ) ) ;
#12736 = ORIENTED_EDGE ( 'NONE', *, *, #9012, .F. ) ;
#12737 = CARTESIAN_POINT ( 'NONE',  ( -42.49999999999999289, -17.68172400785659448, 96.37435565298210349 ) ) ;
#12738 = CARTESIAN_POINT ( 'NONE',  ( -10.00000000000000178, 0.000000000000000000, 0.000000000000000000 ) ) ;
#12739 = DIRECTION ( 'NONE',  ( 9.178431089824344374E-17, -6.938893903907203726E-17, -1.000000000000000000 ) ) ;
#12740 = CARTESIAN_POINT ( 'NONE',  ( -34.50000000000000000, -115.9929510916434481, 11.21034663311132107 ) ) ;
#12741 = CARTESIAN_POINT ( 'NONE',  ( 12.55910585664917711, 0.7408941433508786645, -1.200000000000006617 ) ) ;
#12742 = CARTESIAN_POINT ( 'NONE',  ( -35.00000000000000000, -114.0592624029313242, 3.003524454178448710 ) ) ;
#12743 = CIRCLE ( 'NONE', #32871, 17.49900000000001299 ) ;
#12744 = CARTESIAN_POINT ( 'NONE',  ( -34.50120407906360498, -115.9929510916434481, 12.67985367974112343 ) ) ;
#12746 = DIRECTION ( 'NONE',  ( -1.000000000000000000, 0.000000000000000000, 0.000000000000000000 ) ) ;
#12745 = VECTOR ( 'NONE', #26058, 1000.000000000000000 ) ;
#12747 = CARTESIAN_POINT ( 'NONE',  ( -42.49999999999999289, -21.98076211353320630, 86.49999999999995737 ) ) ;
#12748 = DIRECTION ( 'NONE',  ( 0.000000000000000000, 0.000000000000000000, 1.000000000000000000 ) ) ;
#12749 = LINE ( 'NONE', #12926, #34196 ) ;
#12750 = DIRECTION ( 'NONE',  ( -1.000000000000000000, -0.000000000000000000, 0.000000000000000000 ) ) ;
#12751 = DIRECTION ( 'NONE',  ( 0.000000000000000000, 0.000000000000000000, -1.000000000000000000 ) ) ;
#12752 = ORIENTED_EDGE ( 'NONE', *, *, #17168, .F. ) ;
#12753 = CARTESIAN_POINT ( 'NONE',  ( -35.02454729103298803, -113.1123104723225197, 3.902725545821551290 ) ) ;
#12754 = FACE_OUTER_BOUND ( 'NONE', #33986, .T. ) ;
#12755 = CARTESIAN_POINT ( 'NONE',  ( -35.50000000000000000, -113.0140978167156902, -0.6247823525984268489 ) ) ;
#12756 = ORIENTED_EDGE ( 'NONE', *, *, #24984, .T. ) ;
#12757 = VERTEX_POINT ( 'NONE', #3054 ) ;
#12758 = ADVANCED_FACE ( 'NONE', ( #32933 ), #16539, .T. ) ;
#12759 = CARTESIAN_POINT ( 'NONE',  ( 29.99999999999999645, 10.58300524425836819, -3.000000000000002665 ) ) ;
#12760 = ORIENTED_EDGE ( 'NONE', *, *, #9054, .T. ) ;
#12761 = EDGE_CURVE ( 'NONE', #28899, #19518, #24158, .T. ) ;
#12762 = ORIENTED_EDGE ( 'NONE', *, *, #6614, .F. ) ;
#12763 = ORIENTED_EDGE ( 'NONE', *, *, #20089, .T. ) ;
#12764 = DIRECTION ( 'NONE',  ( 0.000000000000000000, 0.000000000000000000, -1.000000000000000000 ) ) ;
#12765 = CARTESIAN_POINT ( 'NONE',  ( 8.000000000000007105, 3.268936481846187903, 13.61301047812924025 ) ) ;
#12766 = EDGE_CURVE ( 'NONE', #20884, #6031, #30501, .T. ) ;
#12767 = PRESENTATION_LAYER_ASSIGNMENT (  '', '', ( #30571 ) ) ;
#12768 = AXIS2_PLACEMENT_3D ( 'NONE', #15013, #14841, #4241 ) ;
#12769 = DIRECTION ( 'NONE',  ( -0.000000000000000000, -0.2538061376417689030, -0.9672551082808338307 ) ) ;
#12770 = ADVANCED_FACE ( 'NONE', ( #24657 ), #12063, .T. ) ;
#12771 = CARTESIAN_POINT ( 'NONE',  ( 8.000000000000000000, -8.931325931664709117, 16.53603053422203573 ) ) ;
#12772 = EDGE_LOOP ( 'NONE', ( #30269, #14176, #25739, #35452 ) ) ;
#12773 = ORIENTED_EDGE ( 'NONE', *, *, #12100, .T. ) ;
#12774 = CARTESIAN_POINT ( 'NONE',  ( -35.50000000000000711, -112.0141053790792114, 0.9054673897245171243 ) ) ;
#12775 = DIRECTION ( 'NONE',  ( -1.000000000000000000, 8.673617379884106963E-17, -1.502314598737155580E-16 ) ) ;
#12776 = DIRECTION ( 'NONE',  ( 0.000000000000000000, 0.000000000000000000, -1.000000000000000000 ) ) ;
#12777 = ORIENTED_EDGE ( 'NONE', *, *, #8517, .F. ) ;
#12778 = CARTESIAN_POINT ( 'NONE',  ( 6.896599878636562764, -12.98179148322720167, 0.000000000000000000 ) ) ;
#12779 = CIRCLE ( 'NONE', #32905, 9.999999999999994671 ) ;
#12780 = CARTESIAN_POINT ( 'NONE',  ( -34.50000000000000000, -112.0414288467712112, 1.115164475686276191 ) ) ;
#12781 = CARTESIAN_POINT ( 'NONE',  ( -34.50000000000000000, -114.2598117360253696, 9.542047897280109936 ) ) ;
#12782 = CARTESIAN_POINT ( 'NONE',  ( 4.000000000000000000, 13.24207120356986422, -14.98824707027428005 ) ) ;
#12783 = CARTESIAN_POINT ( 'NONE',  ( -35.56312645773537895, -114.9929510916434339, 12.87038173996308998 ) ) ;
#12784 = DIRECTION ( 'NONE',  ( 1.000000000000000000, -5.339440136655842133E-16, -1.047965281155519420E-16 ) ) ;
#12785 = CARTESIAN_POINT ( 'NONE',  ( -34.50000000000000000, -114.9928438774171582, 10.49113435197128652 ) ) ;
#12786 = DIRECTION ( 'NONE',  ( -1.000000000000000000, 0.000000000000000000, 0.000000000000000000 ) ) ;
#12787 = EDGE_CURVE ( 'NONE', #25508, #23788, #13236, .T. ) ;
#12788 = LINE ( 'NONE', #2189, #10945 ) ;
#12789 = FACE_OUTER_BOUND ( 'NONE', #32290, .T. ) ;
#12790 = ORIENTED_EDGE ( 'NONE', *, *, #16113, .F. ) ;
#12791 = CARTESIAN_POINT ( 'NONE',  ( 0.000000000000000000, 16.71027810728552154, 4.579731798933998732 ) ) ;
#12792 = DIRECTION ( 'NONE',  ( -1.734723475976807094E-16, 1.000000000000000000, -1.067522139062650474E-15 ) ) ;
#12793 = EDGE_LOOP ( 'NONE', ( #27218, #17105, #11603, #9209 ) ) ;
#12794 = CIRCLE ( 'NONE', #26599, 15.49899999999998101 ) ;
#12795 = CARTESIAN_POINT ( 'NONE',  ( -37.34375000000001421, -114.9929510916434339, 13.11852480586264669 ) ) ;
#12796 = ORIENTED_EDGE ( 'NONE', *, *, #12809, .T. ) ;
#12797 = AXIS2_PLACEMENT_3D ( 'NONE', #1751, #20627, #28936 ) ;
#12798 = AXIS2_PLACEMENT_3D ( 'NONE', #17893, #33759, #14650 ) ;
#12799 = CARTESIAN_POINT ( 'NONE',  ( -38.97545270896704039, -113.1123104723225197, 3.847274454178449599 ) ) ;
#12800 = DIRECTION ( 'NONE',  ( 0.000000000000000000, 0.000000000000000000, 1.000000000000000000 ) ) ;
#12801 = ORIENTED_EDGE ( 'NONE', *, *, #10063, .F. ) ;
#12802 = CARTESIAN_POINT ( 'NONE',  ( -55.00000000000000000, 0.000000000000000000, 0.000000000000000000 ) ) ;
#12803 = ORIENTED_EDGE ( 'NONE', *, *, #1360, .F. ) ;
#12804 = EDGE_CURVE ( 'NONE', #30169, #34014, #23000, .T. ) ;
#12805 = CARTESIAN_POINT ( 'NONE',  ( -34.50000000000000000, -113.0140978167140702, 0.8752176474015603835 ) ) ;
#12806 = DIRECTION ( 'NONE',  ( -1.000000000000000000, 0.000000000000000000, 0.000000000000000000 ) ) ;
#12807 = DIRECTION ( 'NONE',  ( -0.000000000000000000, -0.000000000000000000, -1.000000000000000000 ) ) ;
#12808 = EDGE_CURVE ( 'NONE', #19295, #11649, #27043, .T. ) ;
#12809 = EDGE_CURVE ( 'NONE', #5782, #31873, #30582, .T. ) ;
#12810 = ORIENTED_EDGE ( 'NONE', *, *, #23357, .T. ) ;
#12811 = CARTESIAN_POINT ( 'NONE',  ( -34.02454729103298092, -115.3019030900506294, 1.597274454178448932 ) ) ;
#12812 = FACE_OUTER_BOUND ( 'NONE', #3102, .T. ) ;
#12813 = DIRECTION ( 'NONE',  ( -1.000000000000000000, 0.000000000000000000, 0.000000000000000000 ) ) ;
#12814 = VERTEX_POINT ( 'NONE', #25005 ) ;
#12815 = ORIENTED_EDGE ( 'NONE', *, *, #32745, .T. ) ;
#12816 = CARTESIAN_POINT ( 'NONE',  ( 8.000000000000000000, -18.62763138773848581, -2.494040418455559127 ) ) ;
#12817 = EDGE_CURVE ( 'NONE', #18374, #10377, #30420, .T. ) ;
#12818 = CARTESIAN_POINT ( 'NONE',  ( -49.99999999999999289, -26.99999999999999645, 113.9999999999999858 ) ) ;
#12819 = EDGE_LOOP ( 'NONE', ( #31866, #33088, #29829, #9563 ) ) ;
#12820 = EDGE_LOOP ( 'NONE', ( #25504, #22788, #31334, #14223 ) ) ;
#12821 = CARTESIAN_POINT ( 'NONE',  ( -34.50000000000000000, -111.8727710936879589, 2.535339294948415922 ) ) ;
#12822 = AXIS2_PLACEMENT_3D ( 'NONE', #6532, #14449, #25277 ) ;
#12823 = CARTESIAN_POINT ( 'NONE',  ( -1.599999999999990319, 0.000000000000000000, 0.000000000000000000 ) ) ;
#12824 = EDGE_LOOP ( 'NONE', ( #33333, #22681, #20976, #9868 ) ) ;
#12825 = VERTEX_POINT ( 'NONE', #330 ) ;
#12826 = DIRECTION ( 'NONE',  ( -1.000000000000000000, 0.000000000000000000, 0.000000000000000000 ) ) ;
#12827 = CARTESIAN_POINT ( 'NONE',  ( -34.50000000000000000, -113.9929510916432207, 10.50625754673563250 ) ) ;
#12828 =( BOUNDED_SURFACE ( )  B_SPLINE_SURFACE ( 3, 2, ( 
 ( #9025, #11908, #31172, #3821, #12084, #1114, #34426, #25791, #31351, #23060, #14781, #1282, #6501, #20167, #23242, #34057, #9204, #33877, #6861, #19988, #9383, #25427, #23428, #17476, #3644, #14593, #20342, #28474, #30993, #25607, #12268, #6678, #4008, #17659, #6327, #28664, #9743, #22885, #34235, #7034, #20704, #17832, #18009, #17298, #11724, #31704, #28301, #14951, #9564, #25958, #20532, #31538, #28833, #4181, #15121, #26133, #1464, #928, #12445, #29007, #14421, #742, #22697, #33689, #18551, #4552, #21062, #16014, #23970, #4357, #21423, #15483, #26500, #12984, #7926, #29376, #18908, #4722, #32068, #24325, #21250 ),
 ( #1836, #12811, #34965, #15303, #15657, #26316, #23789, #29204, #18193, #34773, #10465, #32245, #4890, #29556, #10289, #7571, #1653, #32419, #23608, #7743, #18375, #12630, #18725, #7403, #10095, #34601, #26679, #9917, #35316, #29727, #15832, #20879, #26853, #2011, #2205, #13174, #24148, #35141, #31880, #5071, #27031, #2375, #13346, #10636, #21594, #32594, #7211, #33975, #5, #11162, #14683, #22971, #10822, #20081, #19080, #21779, #27208, #19249, #174, #32773, #1031, #2551, #5594, #8097, #12006, #3556, #25515, #2903, #8934, #25697, #2730, #28386, #33601, #6247, #6417, #30255, #16555, #27382, #28215, #17385, #3729 ),
 ( #5247, #35489, #30078, #9302, #16188, #31090, #29905, #5419, #13517, #27565, #22132, #24498, #16367, #13694, #33796, #24676, #10990, #21956, #32950, #8273, #13864, #14502, #19898, #17208, #11813, #24849, #30911, #9121, #832, #22793, #6775, #34509, #12541, #1203, #18287, #28747, #17560, #15042, #26587, #9659, #25879, #4453, #34151, #29288, #9473, #4100, #31266, #12354, #9828, #12901, #31794, #7129, #1925, #23514, #4274, #34329, #31443, #26049, #31975, #20428, #34688, #20792, #23331, #28569, #29105, #17747, #4633, #12182, #10011, #23697, #3920, #23154, #14870, #20617, #20256, #1379, #31616, #15212, #6951, #17926, #28923 ),
 ( #15567, #26219, #1559, #18102, #15395, #26404, #1737, #12721, #20971, #7311, #23883, #34871, #6587, #4807, #5163, #21167, #19172, #26952, #35059, #10379, #35229, #4979, #26767, #21337, #32696, #2461, #35400, #27122, #2112, #7836, #30170, #18643, #29999, #13265, #24413, #16463, #5337, #10197, #7655, #32330, #13432, #7485, #8192, #29642, #13088, #10727, #16105, #18824, #21696, #2827, #2294, #8017, #5507, #19000, #27481, #13786, #24074, #16279, #10548, #24238, #24771, #27295, #2639, #15934, #29826, #13602, #32156, #24597, #15750, #32502, #21505, #35588, #18463, #10912, #21877, #32869, #29464, #33048, #24944, #11432, #20041 ),
 ( #8361, #30699, #30353, #33224, #16816, #25117, #33389, #22396, #31046, #8714, #16988, #19682, #446, #22571, #27826, #5853, #8894, #6028, #30522, #19517, #28173, #5686, #27995, #11085, #9079, #3162, #267, #11252, #3346, #14118, #16644, #22223, #33563, #14295, #25296, #617, #27656, #11598, #6377, #8546, #19856, #30869, #6205, #17341, #17167, #95, #3515, #14463, #25474, #19342, #33748, #794, #2994, #11774, #22752, #28344, #3691, #14642, #22054, #13954, #20928, #31581, #31927, #23661, #6547, #6912, #15001, #17708, #9969, #17884, #26179, #20386, #9615, #1514, #986, #28879, #31222, #12313, #28525, #20582, #18243 ),
 ( #31398, #22931, #14834, #1334, #33929, #6732, #7264, #26005, #17522, #9792, #3875, #34647, #25840, #34106, #11965, #28710, #15172, #29248, #12496, #23478, #4593, #4232, #34473, #4058, #1162, #23285, #1698, #12137, #4407, #20754, #34284, #9259, #31752, #23107, #25654, #9429, #15352, #29059, #20211, #7084, #18059, #26364, #12684, #29953, #18953, #21294, #2063, #29780, #7791, #32115, #13560, #24026, #24551, #5120, #15710, #32291, #27254, #35188, #15529, #32649, #26726, #13038, #24194, #19127, #4940, #30125, #35013, #4767, #29421, #10333, #21647, #32464, #16059, #27078, #10504, #21468, #26550, #7973, #34824, #5294, #29601 ),
 ( #7611, #1884, #18602, #21116, #10869, #16233, #2419, #10146, #18777, #15888, #26908, #2251, #13219, #13388, #12859, #24369, #35357, #10686, #2595, #35543, #21830, #32826, #8145, #23837, #7445, #18422, #25434, #33697, #22006, #30822, #30307, #33003, #2784, #30485, #11395, #8315, #11731, #13746, #16773, #19296, #22704, #14255, #575, #14074, #19644, #752, #13912, #3474, #8677, #16942, #17126, #5816, #27785, #2953, #3301, #28130, #14427, #24899, #19994, #3121, #16415, #11041, #5644, #9035, #27435, #6161, #5463, #16604, #24726, #25070, #33350, #54, #27616, #224, #8850, #11208, #22178, #33181, #8509, #19483, #399 ) ),
 .UNSPECIFIED., .T., .F., .F. ) 
 B_SPLINE_SURFACE_WITH_KNOTS ( ( 4, 3, 4 ),
 ( 3, 2, 2, 2, 2, 2, 2, 2, 2, 2, 2, 2, 2, 2, 2, 2, 2, 2, 2, 2, 2, 2, 2, 2, 2, 2, 2, 2, 2, 2, 2, 2, 2, 2, 2, 2, 2, 2, 2, 2, 3 ),
 ( 0.000000000000000000, 0.5000000000000000000, 1.000000000000000000 ),
 ( 0.000000000000000000, 0.02500000000000000139, 0.05000000000000000278, 0.07499999999999999722, 0.1000000000000000056, 0.1250000000000000000, 0.1499999999999999944, 0.1749999999999999889, 0.2000000000000000111, 0.2250000000000000056, 0.2500000000000000000, 0.2750000000000000222, 0.2999999999999999889, 0.3250000000000000111, 0.3499999999999999778, 0.3750000000000000000, 0.4000000000000000222, 0.4249999999999999889, 0.4500000000000000111, 0.4749999999999999778, 0.5000000000000000000, 0.5250000000000000222, 0.5500000000000000444, 0.5749999999999999556, 0.5999999999999999778, 0.6250000000000000000, 0.6500000000000000222, 0.6750000000000000444, 0.6999999999999999556, 0.7249999999999999778, 0.7500000000000000000, 0.7750000000000000222, 0.8000000000000000444, 0.8249999999999999556, 0.8499999999999999778, 0.8750000000000000000, 0.9000000000000000222, 0.9250000000000000444, 0.9499999999999999556, 0.9749999999999999778, 1.000000000000000000 ),
 .UNSPECIFIED. ) 
 GEOMETRIC_REPRESENTATION_ITEM ( )  RATIONAL_B_SPLINE_SURFACE ( (
 ( 1.000000000000000000, 0.9238795325112867385, 1.000000000000000000, 0.9238795325112867385, 1.000000000000000000, 0.9238795325112867385, 1.000000000000000000, 0.9238795325112867385, 1.000000000000000000, 0.9238795325112867385, 1.000000000000000000, 0.9238795325112867385, 1.000000000000000000, 0.9238795325112867385, 1.000000000000000000, 0.9238795325112867385, 1.000000000000000000, 0.9238795325112867385, 1.000000000000000000, 0.9238795325112867385, 1.000000000000000000, 0.9238795325112867385, 1.000000000000000000, 0.9238795325112867385, 1.000000000000000000, 0.9238795325112867385, 1.000000000000000000, 0.9238795325112867385, 1.000000000000000000, 0.9238795325112867385, 1.000000000000000000, 0.9238795325112867385, 1.000000000000000000, 0.9238795325112867385, 1.000000000000000000, 0.9238795325112867385, 1.000000000000000000, 0.9238795325112867385, 1.000000000000000000, 0.9238795325112867385, 1.000000000000000000, 0.9238795325112867385, 1.000000000000000000, 0.9238795325112867385, 1.000000000000000000, 0.9238795325112867385, 1.000000000000000000, 0.9238795325112867385, 1.000000000000000000, 0.9238795325112867385, 1.000000000000000000, 0.9238795325112867385, 1.000000000000000000, 0.9238795325112867385, 1.000000000000000000, 0.9238795325112867385, 1.000000000000000000, 0.9238795325112867385, 1.000000000000000000, 0.9238795325112867385, 1.000000000000000000, 0.9238795325112867385, 1.000000000000000000, 0.9238795325112867385, 1.000000000000000000, 0.9238795325112867385, 1.000000000000000000, 0.9238795325112867385, 1.000000000000000000, 0.9238795325112867385, 1.000000000000000000, 0.9238795325112867385, 1.000000000000000000, 0.9238795325112867385, 1.000000000000000000, 0.9238795325112867385, 1.000000000000000000, 0.9238795325112867385, 1.000000000000000000, 0.9238795325112867385, 1.000000000000000000),
 ( 0.3333333333333333703, 0.3079598441704289313, 0.3333333333333333703, 0.3079598441704289313, 0.3333333333333333703, 0.3079598441704289313, 0.3333333333333333703, 0.3079598441704289313, 0.3333333333333333703, 0.3079598441704289313, 0.3333333333333333703, 0.3079598441704289313, 0.3333333333333333703, 0.3079598441704289313, 0.3333333333333333703, 0.3079598441704289313, 0.3333333333333333703, 0.3079598441704289313, 0.3333333333333333703, 0.3079598441704289313, 0.3333333333333333703, 0.3079598441704289313, 0.3333333333333333703, 0.3079598441704289313, 0.3333333333333333703, 0.3079598441704289313, 0.3333333333333333703, 0.3079598441704289313, 0.3333333333333333703, 0.3079598441704289313, 0.3333333333333333703, 0.3079598441704289313, 0.3333333333333333703, 0.3079598441704289313, 0.3333333333333333703, 0.3079598441704289313, 0.3333333333333333703, 0.3079598441704289313, 0.3333333333333333703, 0.3079598441704289313, 0.3333333333333333703, 0.3079598441704289313, 0.3333333333333333703, 0.3079598441704289313, 0.3333333333333333703, 0.3079598441704289313, 0.3333333333333333703, 0.3079598441704289313, 0.3333333333333333703, 0.3079598441704289313, 0.3333333333333333703, 0.3079598441704289313, 0.3333333333333333703, 0.3079598441704289313, 0.3333333333333333703, 0.3079598441704289313, 0.3333333333333333703, 0.3079598441704289313, 0.3333333333333333703, 0.3079598441704289313, 0.3333333333333333703, 0.3079598441704289313, 0.3333333333333333703, 0.3079598441704289313, 0.3333333333333333703, 0.3079598441704289313, 0.3333333333333333703, 0.3079598441704289313, 0.3333333333333333703, 0.3079598441704289313, 0.3333333333333333703, 0.3079598441704289313, 0.3333333333333333703, 0.3079598441704289313, 0.3333333333333333703, 0.3079598441704289313, 0.3333333333333333703, 0.3079598441704289313, 0.3333333333333333703, 0.3079598441704289313, 0.3333333333333333703),
 ( 0.3333333333333333703, 0.3079598441704289313, 0.3333333333333333703, 0.3079598441704289313, 0.3333333333333333703, 0.3079598441704289313, 0.3333333333333333703, 0.3079598441704289313, 0.3333333333333333703, 0.3079598441704289313, 0.3333333333333333703, 0.3079598441704289313, 0.3333333333333333703, 0.3079598441704289313, 0.3333333333333333703, 0.3079598441704289313, 0.3333333333333333703, 0.3079598441704289313, 0.3333333333333333703, 0.3079598441704289313, 0.3333333333333333703, 0.3079598441704289313, 0.3333333333333333703, 0.3079598441704289313, 0.3333333333333333703, 0.3079598441704289313, 0.3333333333333333703, 0.3079598441704289313, 0.3333333333333333703, 0.3079598441704289313, 0.3333333333333333703, 0.3079598441704289313, 0.3333333333333333703, 0.3079598441704289313, 0.3333333333333333703, 0.3079598441704289313, 0.3333333333333333703, 0.3079598441704289313, 0.3333333333333333703, 0.3079598441704289313, 0.3333333333333333703, 0.3079598441704289313, 0.3333333333333333703, 0.3079598441704289313, 0.3333333333333333703, 0.3079598441704289313, 0.3333333333333333703, 0.3079598441704289313, 0.3333333333333333703, 0.3079598441704289313, 0.3333333333333333703, 0.3079598441704289313, 0.3333333333333333703, 0.3079598441704289313, 0.3333333333333333703, 0.3079598441704289313, 0.3333333333333333703, 0.3079598441704289313, 0.3333333333333333703, 0.3079598441704289313, 0.3333333333333333703, 0.3079598441704289313, 0.3333333333333333703, 0.3079598441704289313, 0.3333333333333333703, 0.3079598441704289313, 0.3333333333333333703, 0.3079598441704289313, 0.3333333333333333703, 0.3079598441704289313, 0.3333333333333333703, 0.3079598441704289313, 0.3333333333333333703, 0.3079598441704289313, 0.3333333333333333703, 0.3079598441704289313, 0.3333333333333333703, 0.3079598441704289313, 0.3333333333333333703, 0.3079598441704289313, 0.3333333333333333703),
 ( 1.000000000000000000, 0.9238795325112867385, 1.000000000000000000, 0.9238795325112867385, 1.000000000000000000, 0.9238795325112867385, 1.000000000000000000, 0.9238795325112867385, 1.000000000000000000, 0.9238795325112867385, 1.000000000000000000, 0.9238795325112867385, 1.000000000000000000, 0.9238795325112867385, 1.000000000000000000, 0.9238795325112867385, 1.000000000000000000, 0.9238795325112867385, 1.000000000000000000, 0.9238795325112867385, 1.000000000000000000, 0.9238795325112867385, 1.000000000000000000, 0.9238795325112867385, 1.000000000000000000, 0.9238795325112867385, 1.000000000000000000, 0.9238795325112867385, 1.000000000000000000, 0.9238795325112867385, 1.000000000000000000, 0.9238795325112867385, 1.000000000000000000, 0.9238795325112867385, 1.000000000000000000, 0.9238795325112867385, 1.000000000000000000, 0.9238795325112867385, 1.000000000000000000, 0.9238795325112867385, 1.000000000000000000, 0.9238795325112867385, 1.000000000000000000, 0.9238795325112867385, 1.000000000000000000, 0.9238795325112867385, 1.000000000000000000, 0.9238795325112867385, 1.000000000000000000, 0.9238795325112867385, 1.000000000000000000, 0.9238795325112867385, 1.000000000000000000, 0.9238795325112867385, 1.000000000000000000, 0.9238795325112867385, 1.000000000000000000, 0.9238795325112867385, 1.000000000000000000, 0.9238795325112867385, 1.000000000000000000, 0.9238795325112867385, 1.000000000000000000, 0.9238795325112867385, 1.000000000000000000, 0.9238795325112867385, 1.000000000000000000, 0.9238795325112867385, 1.000000000000000000, 0.9238795325112867385, 1.000000000000000000, 0.9238795325112867385, 1.000000000000000000, 0.9238795325112867385, 1.000000000000000000, 0.9238795325112867385, 1.000000000000000000, 0.9238795325112867385, 1.000000000000000000, 0.9238795325112867385, 1.000000000000000000),
 ( 0.3333333333333333703, 0.3079598441704289313, 0.3333333333333333703, 0.3079598441704289313, 0.3333333333333333703, 0.3079598441704289313, 0.3333333333333333703, 0.3079598441704289313, 0.3333333333333333703, 0.3079598441704289313, 0.3333333333333333703, 0.3079598441704289313, 0.3333333333333333703, 0.3079598441704289313, 0.3333333333333333703, 0.3079598441704289313, 0.3333333333333333703, 0.3079598441704289313, 0.3333333333333333703, 0.3079598441704289313, 0.3333333333333333703, 0.3079598441704289313, 0.3333333333333333703, 0.3079598441704289313, 0.3333333333333333703, 0.3079598441704289313, 0.3333333333333333703, 0.3079598441704289313, 0.3333333333333333703, 0.3079598441704289313, 0.3333333333333333703, 0.3079598441704289313, 0.3333333333333333703, 0.3079598441704289313, 0.3333333333333333703, 0.3079598441704289313, 0.3333333333333333703, 0.3079598441704289313, 0.3333333333333333703, 0.3079598441704289313, 0.3333333333333333703, 0.3079598441704289313, 0.3333333333333333703, 0.3079598441704289313, 0.3333333333333333703, 0.3079598441704289313, 0.3333333333333333703, 0.3079598441704289313, 0.3333333333333333703, 0.3079598441704289313, 0.3333333333333333703, 0.3079598441704289313, 0.3333333333333333703, 0.3079598441704289313, 0.3333333333333333703, 0.3079598441704289313, 0.3333333333333333703, 0.3079598441704289313, 0.3333333333333333703, 0.3079598441704289313, 0.3333333333333333703, 0.3079598441704289313, 0.3333333333333333703, 0.3079598441704289313, 0.3333333333333333703, 0.3079598441704289313, 0.3333333333333333703, 0.3079598441704289313, 0.3333333333333333703, 0.3079598441704289313, 0.3333333333333333703, 0.3079598441704289313, 0.3333333333333333703, 0.3079598441704289313, 0.3333333333333333703, 0.3079598441704289313, 0.3333333333333333703, 0.3079598441704289313, 0.3333333333333333703, 0.3079598441704289313, 0.3333333333333333703),
 ( 0.3333333333333333703, 0.3079598441704289313, 0.3333333333333333703, 0.3079598441704289313, 0.3333333333333333703, 0.3079598441704289313, 0.3333333333333333703, 0.3079598441704289313, 0.3333333333333333703, 0.3079598441704289313, 0.3333333333333333703, 0.3079598441704289313, 0.3333333333333333703, 0.3079598441704289313, 0.3333333333333333703, 0.3079598441704289313, 0.3333333333333333703, 0.3079598441704289313, 0.3333333333333333703, 0.3079598441704289313, 0.3333333333333333703, 0.3079598441704289313, 0.3333333333333333703, 0.3079598441704289313, 0.3333333333333333703, 0.3079598441704289313, 0.3333333333333333703, 0.3079598441704289313, 0.3333333333333333703, 0.3079598441704289313, 0.3333333333333333703, 0.3079598441704289313, 0.3333333333333333703, 0.3079598441704289313, 0.3333333333333333703, 0.3079598441704289313, 0.3333333333333333703, 0.3079598441704289313, 0.3333333333333333703, 0.3079598441704289313, 0.3333333333333333703, 0.3079598441704289313, 0.3333333333333333703, 0.3079598441704289313, 0.3333333333333333703, 0.3079598441704289313, 0.3333333333333333703, 0.3079598441704289313, 0.3333333333333333703, 0.3079598441704289313, 0.3333333333333333703, 0.3079598441704289313, 0.3333333333333333703, 0.3079598441704289313, 0.3333333333333333703, 0.3079598441704289313, 0.3333333333333333703, 0.3079598441704289313, 0.3333333333333333703, 0.3079598441704289313, 0.3333333333333333703, 0.3079598441704289313, 0.3333333333333333703, 0.3079598441704289313, 0.3333333333333333703, 0.3079598441704289313, 0.3333333333333333703, 0.3079598441704289313, 0.3333333333333333703, 0.3079598441704289313, 0.3333333333333333703, 0.3079598441704289313, 0.3333333333333333703, 0.3079598441704289313, 0.3333333333333333703, 0.3079598441704289313, 0.3333333333333333703, 0.3079598441704289313, 0.3333333333333333703, 0.3079598441704289313, 0.3333333333333333703),
 ( 1.000000000000000000, 0.9238795325112867385, 1.000000000000000000, 0.9238795325112867385, 1.000000000000000000, 0.9238795325112867385, 1.000000000000000000, 0.9238795325112867385, 1.000000000000000000, 0.9238795325112867385, 1.000000000000000000, 0.9238795325112867385, 1.000000000000000000, 0.9238795325112867385, 1.000000000000000000, 0.9238795325112867385, 1.000000000000000000, 0.9238795325112867385, 1.000000000000000000, 0.9238795325112867385, 1.000000000000000000, 0.9238795325112867385, 1.000000000000000000, 0.9238795325112867385, 1.000000000000000000, 0.9238795325112867385, 1.000000000000000000, 0.9238795325112867385, 1.000000000000000000, 0.9238795325112867385, 1.000000000000000000, 0.9238795325112867385, 1.000000000000000000, 0.9238795325112867385, 1.000000000000000000, 0.9238795325112867385, 1.000000000000000000, 0.9238795325112867385, 1.000000000000000000, 0.9238795325112867385, 1.000000000000000000, 0.9238795325112867385, 1.000000000000000000, 0.9238795325112867385, 1.000000000000000000, 0.9238795325112867385, 1.000000000000000000, 0.9238795325112867385, 1.000000000000000000, 0.9238795325112867385, 1.000000000000000000, 0.9238795325112867385, 1.000000000000000000, 0.9238795325112867385, 1.000000000000000000, 0.9238795325112867385, 1.000000000000000000, 0.9238795325112867385, 1.000000000000000000, 0.9238795325112867385, 1.000000000000000000, 0.9238795325112867385, 1.000000000000000000, 0.9238795325112867385, 1.000000000000000000, 0.9238795325112867385, 1.000000000000000000, 0.9238795325112867385, 1.000000000000000000, 0.9238795325112867385, 1.000000000000000000, 0.9238795325112867385, 1.000000000000000000, 0.9238795325112867385, 1.000000000000000000, 0.9238795325112867385, 1.000000000000000000, 0.9238795325112867385, 1.000000000000000000, 0.9238795325112867385, 1.000000000000000000) ) ) 
 REPRESENTATION_ITEM ( '' )  SURFACE ( )  );
#12829 = LINE ( 'NONE', #12288, #10501 ) ;
#12830 = CARTESIAN_POINT ( 'NONE',  ( -37.62959469683911351, -113.9929510916434339, 13.10254527216511633 ) ) ;
#12831 = EDGE_CURVE ( 'NONE', #20345, #13985, #5201, .T. ) ;
#12832 = CARTESIAN_POINT ( 'NONE',  ( -36.06250000000000711, -115.9929510916434481, 13.11852480586264846 ) ) ;
#12833 = FACE_OUTER_BOUND ( 'NONE', #11045, .T. ) ;
#12834 = VECTOR ( 'NONE', #23753, 1000.000000000000000 ) ;
#12835 = CARTESIAN_POINT ( 'NONE',  ( 10.50000000000000178, 0.000000000000000000, -1.200000000000006617 ) ) ;
#12836 = ADVANCED_FACE ( 'NONE', ( #25195, #516 ), #11495, .F. ) ;
#12837 = AXIS2_PLACEMENT_3D ( 'NONE', #18657, #27670, #19362 ) ;
#12838 = ORIENTED_EDGE ( 'NONE', *, *, #20702, .T. ) ;
#12839 = CARTESIAN_POINT ( 'NONE',  ( 4.000000000000003553, 24.47917365149946534, 45.87777302070943364 ) ) ;
#12840 = DIRECTION ( 'NONE',  ( -1.000000000000000000, -0.000000000000000000, 0.000000000000000000 ) ) ;
#12841 = LINE ( 'NONE', #12297, #22580 ) ;
#12842 = VERTEX_POINT ( 'NONE', #11839 ) ;
#12843 = DIRECTION ( 'NONE',  ( 0.000000000000000000, -1.000000000000000000, 0.000000000000000000 ) ) ;
#12844 = AXIS2_PLACEMENT_3D ( 'NONE', #27598, #5629, #3459 ) ;
#12845 = AXIS2_PLACEMENT_3D ( 'NONE', #27712, #5742, #30754 ) ;
#12846 = CARTESIAN_POINT ( 'NONE',  ( -35.50000000000000711, -112.0140978167138712, 0.3752176474015640473 ) ) ;
#12847 = CARTESIAN_POINT ( 'NONE',  ( 0.000000000000000000, 0.000000000000000000, 50.00000000000000000 ) ) ;
#12848 = EDGE_CURVE ( 'NONE', #5782, #14643, #32218, .T. ) ;
#12849 = VECTOR ( 'NONE', #30351, 1000.000000000000000 ) ;
#12850 = EDGE_CURVE ( 'NONE', #23114, #23381, #8608, .T. ) ;
#12851 = CARTESIAN_POINT ( 'NONE',  ( -35.50000000000000711, -114.1091535596544873, 9.513028657562415447 ) ) ;
#12852 = CARTESIAN_POINT ( 'NONE',  ( 55.00000000000000000, 20.00000000000001776, 120.0000000000000000 ) ) ;
#12853 = ORIENTED_EDGE ( 'NONE', *, *, #16521, .F. ) ;
#12854 = CARTESIAN_POINT ( 'NONE',  ( 5.400000000000085620, -1.000000000000049516, 55.00000000000000711 ) ) ;
#12855 = CARTESIAN_POINT ( 'NONE',  ( -34.50000000000000000, -111.0780159515033034, -1.143161139953928762 ) ) ;
#12856 = DIRECTION ( 'NONE',  ( -1.000000000000000000, 0.000000000000000000, 0.000000000000000000 ) ) ;
#12857 = ORIENTED_EDGE ( 'NONE', *, *, #8447, .T. ) ;
#12858 = EDGE_LOOP ( 'NONE', ( #34913, #10051, #8783, #9336 ) ) ;
#12859 = CARTESIAN_POINT ( 'NONE',  ( -35.54388159064475872, -112.6276912846090568, 2.816024454178448710 ) ) ;
#12860 =( LENGTH_UNIT ( ) NAMED_UNIT ( * ) SI_UNIT ( .MILLI., .METRE. ) );
#12861 = FACE_OUTER_BOUND ( 'NONE', #29147, .T. ) ;
#12863 = EDGE_LOOP ( 'NONE', ( #14955, #13094, #5010, #35068 ) ) ;
#12862 = AXIS2_PLACEMENT_3D ( 'NONE', #30050, #16333, #8244 ) ;
#12864 = VERTEX_POINT ( 'NONE', #25904 ) ;
#12865 = CARTESIAN_POINT ( 'NONE',  ( -35.50000000000000000, -115.0140978167138712, -0.6247823525984403936 ) ) ;
#12866 = AXIS2_PLACEMENT_3D ( 'NONE', #21850, #8165, #19145 ) ;
#12867 = DIRECTION ( 'NONE',  ( -1.000000000000000000, 0.000000000000000000, -0.000000000000000000 ) ) ;
#12868 = DIRECTION ( 'NONE',  ( -1.000000000000000000, -1.836970198721030181E-16, 0.000000000000000000 ) ) ;
#12869 = CIRCLE ( 'NONE', #13458, 47.49900000000001654 ) ;
#12870 = CARTESIAN_POINT ( 'NONE',  ( -37.51635661748575501, -114.9929510916434339, 13.11827392651459157 ) ) ;
#12871 = VECTOR ( 'NONE', #17185, 1000.000000000000000 ) ;
#12872 = CARTESIAN_POINT ( 'NONE',  ( 70.00000000000001421, -36.26296008782259861, 84.27446239413865214 ) ) ;
#12873 = EDGE_CURVE ( 'NONE', #24508, #5329, #33821, .T. ) ;
#12874 = CARTESIAN_POINT ( 'NONE',  ( -37.37500000000009237, -114.9929510916434339, 14.11852480586264846 ) ) ;
#12875 = DIRECTION ( 'NONE',  ( -1.000000000000000000, -1.387778780781445922E-16, 0.000000000000000000 ) ) ;
#12876 = EDGE_CURVE ( 'NONE', #26795, #5670, #2329, .T. ) ;
#12877 = CYLINDRICAL_SURFACE ( 'NONE', #1375, 4.000000000000000000 ) ;
#12878 = EDGE_LOOP ( 'NONE', ( #10059, #3516, #13506, #4007 ) ) ;
#12879 = CARTESIAN_POINT ( 'NONE',  ( -36.62499999999902656, -115.9929510916434481, 13.11852480586264846 ) ) ;
#12880 = CARTESIAN_POINT ( 'NONE',  ( -35.50000000000000711, -115.8878449012421754, -1.128496220799388494 ) ) ;
#12881 = CARTESIAN_POINT ( 'NONE',  ( 7.999999999999992895, 44.47301969247469344, -16.68249143361863318 ) ) ;
#12882 = FACE_OUTER_BOUND ( 'NONE', #29692, .T. ) ;
#12883 = DIRECTION ( 'NONE',  ( 0.000000000000000000, 0.000000000000000000, -1.000000000000000000 ) ) ;
#12884 = AXIS2_PLACEMENT_3D ( 'NONE', #16621, #11582, #19498 ) ;
#12885 = VERTEX_POINT ( 'NONE', #3413 ) ;
#12886 = DIRECTION ( 'NONE',  ( 1.000000000000000000, -0.000000000000000000, -0.000000000000000000 ) ) ;
#12887 = DIRECTION ( 'NONE',  ( -1.000000000000000000, -0.000000000000000000, -0.000000000000000000 ) ) ;
#12888 = DIRECTION ( 'NONE',  ( -1.000000000000000000, 0.000000000000000000, 0.000000000000000000 ) ) ;
#12889 = LINE ( 'NONE', #18453, #22437 ) ;
#12890 = VERTEX_POINT ( 'NONE', #14360 ) ;
#12891 = CARTESIAN_POINT ( 'NONE',  ( -37.66520193420439000, -113.2509883718312977, 3.941024454178448710 ) ) ;
#12892 = DIRECTION ( 'NONE',  ( 0.000000000000000000, 0.000000000000000000, -1.000000000000000000 ) ) ;
#12893 = CARTESIAN_POINT ( 'NONE',  ( -39.49999999999999289, -14.17619866229204106, 93.62476896299857287 ) ) ;
#12894 = EDGE_LOOP ( 'NONE', ( #10060, #18854 ) ) ;
#12895 = VERTEX_POINT ( 'NONE', #22634 ) ;
#12896 = CIRCLE ( 'NONE', #26705, 17.49900000000001299 ) ;
#12897 = DIRECTION ( 'NONE',  ( 0.000000000000000000, 0.000000000000000000, 1.000000000000000000 ) ) ;
#12898 = AXIS2_PLACEMENT_3D ( 'NONE', #34953, #26664, #35129 ) ;
#12899 = LINE ( 'NONE', #7834, #10505 ) ;
#12900 = ORIENTED_EDGE ( 'NONE', *, *, #21810, .F. ) ;
#12901 = CARTESIAN_POINT ( 'NONE',  ( -33.97545270896703329, -115.1833782841879810, 7.090225545821551734 ) ) ;
#12902 = ORIENTED_EDGE ( 'NONE', *, *, #2653, .T. ) ;
#12903 = CYLINDRICAL_SURFACE ( 'NONE', #33943, 4.000000000000000000 ) ;
#12904 = ORIENTED_EDGE ( 'NONE', *, *, #7098, .F. ) ;
#12905 = ORIENTED_EDGE ( 'NONE', *, *, #12276, .F. ) ;
#12906 = LINE ( 'NONE', #9834, #9101 ) ;
#12907 = CARTESIAN_POINT ( 'NONE',  ( 8.000000000000000000, -6.860320204751044315, -13.89802171851389900 ) ) ;
#12908 = ORIENTED_EDGE ( 'NONE', *, *, #8672, .F. ) ;
#12909 = ORIENTED_EDGE ( 'NONE', *, *, #15444, .T. ) ;
#12910 = DIRECTION ( 'NONE',  ( 0.000000000000000000, 0.000000000000000000, 1.000000000000000000 ) ) ;
#12911 = DIRECTION ( 'NONE',  ( -1.000000000000000000, 0.000000000000000000, 0.000000000000000000 ) ) ;
#12912 = ORIENTED_EDGE ( 'NONE', *, *, #32883, .F. ) ;
#12913 = DIRECTION ( 'NONE',  ( 0.000000000000000000, 0.000000000000000000, 1.000000000000000000 ) ) ;
#12914 = CYLINDRICAL_SURFACE ( 'NONE', #3904, 2.799122904894268071 ) ;
#12915 = DIRECTION ( 'NONE',  ( -1.000000000000000000, 0.000000000000000000, 0.000000000000000000 ) ) ;
#12916 = ADVANCED_FACE ( 'NONE', ( #19925 ), #25371, .T. ) ;
#12917 = CARTESIAN_POINT ( 'NONE',  ( -34.50000000000000000, -115.9929510916434481, 12.44250253426871033 ) ) ;
#12918 = CIRCLE ( 'NONE', #34769, 4.000000000000000000 ) ;
#12919 = DIRECTION ( 'NONE',  ( -1.783119874454246424E-31, -1.187911941725854497E-31, 1.000000000000000000 ) ) ;
#12920 = CARTESIAN_POINT ( 'NONE',  ( -38.99999999999999289, -113.9407375970686900, 8.253524454178448266 ) ) ;
#12921 = CARTESIAN_POINT ( 'NONE',  ( -34.50000000000000000, -115.3279708130221479, 8.997521329298534098 ) ) ;
#12922 = DIRECTION ( 'NONE',  ( 0.000000000000000000, 0.000000000000000000, 1.000000000000000000 ) ) ;
#12923 = CIRCLE ( 'NONE', #19302, 20.00000000000000711 ) ;
#12924 = CARTESIAN_POINT ( 'NONE',  ( 3.872983346207429900, -1.000000000000003553, -22.00000000000000000 ) ) ;
#12925 = DIRECTION ( 'NONE',  ( 0.000000000000000000, 0.000000000000000000, -1.000000000000000000 ) ) ;
#12926 = CARTESIAN_POINT ( 'NONE',  ( 4.000000000000000000, -13.24207120356955159, -14.98824707027455183 ) ) ;
#12927 = CARTESIAN_POINT ( 'NONE',  ( 8.000000000000000000, 0.000000000000000000, 0.000000000000000000 ) ) ;
#12928 = CARTESIAN_POINT ( 'NONE',  ( 75.00000000000002842, -27.93100416606587899, 81.50764321173589622 ) ) ;
#12929 = ORIENTED_EDGE ( 'NONE', *, *, #16723, .T. ) ;
#12930 = ADVANCED_FACE ( 'NONE', ( #20462 ), #9503, .T. ) ;
#12931 = CARTESIAN_POINT ( 'NONE',  ( -35.00000000000000000, -113.9407375970686900, 5.496475545821551734 ) ) ;
#12932 = CARTESIAN_POINT ( 'NONE',  ( 7.999999999999992895, 0.000000000000000000, 0.000000000000000000 ) ) ;
#12933 = CARTESIAN_POINT ( 'NONE',  ( -35.50000000000000000, -113.0140978167138712, 0.8752176474015934682 ) ) ;
#12934 = ORIENTED_EDGE ( 'NONE', *, *, #21354, .F. ) ;
#12935 = EDGE_LOOP ( 'NONE', ( #8814, #3053, #16993, #16322 ) ) ;
#12936 = DIRECTION ( 'NONE',  ( 1.000000000000000000, 0.000000000000000000, 0.000000000000000000 ) ) ;
#12937 = CARTESIAN_POINT ( 'NONE',  ( 7.999999999999992895, -39.55064067543046491, -25.36340625197400200 ) ) ;
#12938 = ORIENTED_EDGE ( 'NONE', *, *, #7955, .T. ) ;
#12939 = VERTEX_POINT ( 'NONE', #12209 ) ;
#12940 = ORIENTED_EDGE ( 'NONE', *, *, #7090, .T. ) ;
#12941 = AXIS2_PLACEMENT_3D ( 'NONE', #14665, #5747, #1189 ) ;
#12942 = CARTESIAN_POINT ( 'NONE',  ( -1.387778780781445676E-14, 0.4273491293403097746, -0.7999999999999951594 ) ) ;
#12943 = AXIS2_PLACEMENT_3D ( 'NONE', #28601, #12384, #12030 ) ;
#12944 = CARTESIAN_POINT ( 'NONE',  ( -35.02454729103298092, -113.1123104723225055, 9.902725545821553510 ) ) ;
#12945 = CARTESIAN_POINT ( 'NONE',  ( 10.00000000000000888, -25.98076211353320986, 84.99999999999994316 ) ) ;
#12946 = AXIS2_PLACEMENT_3D ( 'NONE', #34723, #21372, #10416 ) ;
#12947 = CARTESIAN_POINT ( 'NONE',  ( 4.000000000000000000, 4.898587196589412829E-16, 65.00000000000000000 ) ) ;
#12948 = ORIENTED_EDGE ( 'NONE', *, *, #19490, .T. ) ;
#12949 = ORIENTED_EDGE ( 'NONE', *, *, #1777, .T. ) ;
#12950 = CARTESIAN_POINT ( 'NONE',  ( -35.50000000000000711, -112.0140978167138712, 0.2502176474015765373 ) ) ;
#12951 = CIRCLE ( 'NONE', #13541, 8.000000000000007105 ) ;
#12952 = DIRECTION ( 'NONE',  ( 0.000000000000000000, 0.9048270524660175784, 0.4257792915650767673 ) ) ;
#12953 = CARTESIAN_POINT ( 'NONE',  ( 0.000000000000000000, 0.000000000000000000, 0.000000000000000000 ) ) ;
#12954 = ORIENTED_EDGE ( 'NONE', *, *, #31496, .T. ) ;
#12955 = CARTESIAN_POINT ( 'NONE',  ( -1.599999999999989875, -3.455569164145799535E-16, -4.980000000000017302 ) ) ;
#12956 = VECTOR ( 'NONE', #374, 1000.000000000000114 ) ;
#12957 = CARTESIAN_POINT ( 'NONE',  ( -34.50000000000000000, -112.6043641208289188, 1.789429170677330649 ) ) ;
#12958 = EDGE_CURVE ( 'NONE', #440, #1656, #14388, .T. ) ;
#12959 = CARTESIAN_POINT ( 'NONE',  ( -34.50000000000000000, -114.9929510916434339, 10.68227981832981044 ) ) ;
#12960 = EDGE_CURVE ( 'NONE', #18157, #18380, #21881, .T. ) ;
#12961 = LINE ( 'NONE', #23946, #18301 ) ;
#12962 = CARTESIAN_POINT ( 'NONE',  ( -37.66108410722335265, -114.9929510916434339, 13.09299768411426790 ) ) ;
#12963 = DIRECTION ( 'NONE',  ( 0.000000000000000000, -6.938893903907203726E-17, -1.000000000000000000 ) ) ;
#12964 = CARTESIAN_POINT ( 'NONE',  ( -34.50000000000000000, -114.1712995509219724, 9.522174004479579068 ) ) ;
#12965 = CYLINDRICAL_SURFACE ( 'NONE', #15378, 3.799999999999999822 ) ;
#12966 = CARTESIAN_POINT ( 'NONE',  ( -37.99994980024369085, -114.9929510916434339, 12.62670525340494621 ) ) ;
#12967 = DIRECTION ( 'NONE',  ( -1.000000000000000000, -0.000000000000000000, -0.000000000000000000 ) ) ;
#12968 = EDGE_LOOP ( 'NONE', ( #8261, #32240, #1558, #27942 ) ) ;
#12969 = CARTESIAN_POINT ( 'NONE',  ( -55.00000000000000000, 10.00000000000000888, 120.0000000000000000 ) ) ;
#12970 = CARTESIAN_POINT ( 'NONE',  ( 4.000000000000003553, 13.42368113696688958, -3.975523202427861058 ) ) ;
#12971 = CIRCLE ( 'NONE', #14659, 4.800000000000006040 ) ;
#12972 = ORIENTED_EDGE ( 'NONE', *, *, #7699, .T. ) ;
#12973 = CARTESIAN_POINT ( 'NONE',  ( -37.50818044754229419, -114.9929510916434339, 13.11847460610629668 ) ) ;
#12974 = ORIENTED_EDGE ( 'NONE', *, *, #28656, .T. ) ;
#12975 = EDGE_CURVE ( 'NONE', #1868, #15669, #3493, .T. ) ;
#12976 = CARTESIAN_POINT ( 'NONE',  ( -38.37230871539094323, -112.5438815906447729, 6.941024454178449155 ) ) ;
#12977 = DIRECTION ( 'NONE',  ( -1.000000000000000000, 0.000000000000000000, 0.000000000000000000 ) ) ;
#12978 = AXIS2_PLACEMENT_3D ( 'NONE', #26212, #26758, #29632 ) ;
#12979 = ORIENTED_EDGE ( 'NONE', *, *, #20850, .T. ) ;
#12980 = ORIENTED_EDGE ( 'NONE', *, *, #31983, .F. ) ;
#12981 = CIRCLE ( 'NONE', #31371, 19.99999999999998579 ) ;
#12982 = DIRECTION ( 'NONE',  ( 0.000000000000000000, 0.000000000000000000, -1.000000000000000000 ) ) ;
#12983 = VERTEX_POINT ( 'NONE', #3581 ) ;
#12984 = CARTESIAN_POINT ( 'NONE',  ( -38.97545270896704039, -113.1123104723225197, 8.347274454178448266 ) ) ;
#12985 = CIRCLE ( 'NONE', #2074, 20.00000000000000355 ) ;
#12986 = DIRECTION ( 'NONE',  ( 1.000000000000000000, -0.000000000000000000, -0.000000000000000000 ) ) ;
#12987 = CARTESIAN_POINT ( 'NONE',  ( -21.15833593587365513, -28.69486372867094559, 81.70096189432321410 ) ) ;
#12988 = ORIENTED_EDGE ( 'NONE', *, *, #6154, .F. ) ;
#12989 = ORIENTED_EDGE ( 'NONE', *, *, #27794, .F. ) ;
#12990 = CARTESIAN_POINT ( 'NONE',  ( 55.00000000000000711, -25.98076211353320986, 84.99999999999994316 ) ) ;
#12991 = EDGE_CURVE ( 'NONE', #6950, #15285, #14529, .T. ) ;
#12992 = PRESENTATION_STYLE_ASSIGNMENT (( #32781 ) ) ;
#12993 = DIRECTION ( 'NONE',  ( 0.000000000000000000, 0.000000000000000000, 1.000000000000000000 ) ) ;
#12994 = ORIENTED_EDGE ( 'NONE', *, *, #21823, .T. ) ;
#12995 = ORIENTED_EDGE ( 'NONE', *, *, #18188, .F. ) ;
#12996 = CARTESIAN_POINT ( 'NONE',  ( -34.50000000000000000, -113.2224311500466030, -2.624782352598442614 ) ) ;
#12997 = AXIS2_PLACEMENT_3D ( 'NONE', #23270, #31205, #22557 ) ;
#12998 = DIRECTION ( 'NONE',  ( -1.000000000000000000, 0.000000000000000000, 0.000000000000000000 ) ) ;
#12999 = ORIENTED_EDGE ( 'NONE', *, *, #6859, .T. ) ;
#13000 = ORIENTED_EDGE ( 'NONE', *, *, #32390, .F. ) ;
#13001 = CARTESIAN_POINT ( 'NONE',  ( -35.50000000000000711, -114.8847986568751907, 10.03799953695244618 ) ) ;
#13002 = VECTOR ( 'NONE', #14620, 1000.000000000000000 ) ;
#13003 = VECTOR ( 'NONE', #28076, 1000.000000000000000 ) ;
#13004 = VECTOR ( 'NONE', #30728, 1000.000000000000000 ) ;
#13005 = AXIS2_PLACEMENT_3D ( 'NONE', #6100, #25015, #8788 ) ;
#13006 = EDGE_CURVE ( 'NONE', #18147, #1452, #25725, .T. ) ;
#13007 = CARTESIAN_POINT ( 'NONE',  ( -34.50000000000000000, -113.9929510916434339, 10.50625754673577994 ) ) ;
#13008 = EDGE_CURVE ( 'NONE', #15971, #26642, #4126, .T. ) ;
#13009 = CARTESIAN_POINT ( 'NONE',  ( 0.000000000000000000, -2.710505431213761085E-17, 55.00000000000000000 ) ) ;
#13010 = LINE ( 'NONE', #32797, #31185 ) ;
#13011 = ADVANCED_FACE ( 'NONE', ( #25545 ), #17834, .T. ) ;
#13012 = CARTESIAN_POINT ( 'NONE',  ( -34.50000000000000000, -113.9813390189866027, 10.50487145766371100 ) ) ;
#13013 = CIRCLE ( 'NONE', #5529, 2.447112362156711018 ) ;
#13014 = CARTESIAN_POINT ( 'NONE',  ( -38.00000000000000711, -115.9929510916434481, 12.59102132592609102 ) ) ;
#13015 = DIRECTION ( 'NONE',  ( -1.000000000000000000, -0.000000000000000000, -0.000000000000000000 ) ) ;
#13016 = CARTESIAN_POINT ( 'NONE',  ( -34.49999999999998579, -13.17619866229195047, 79.33933265213923391 ) ) ;
#13017 = ORIENTED_EDGE ( 'NONE', *, *, #1789, .T. ) ;
#13018 = ADVANCED_FACE ( 'NONE', ( #9327, #28598 ), #31475, .F. ) ;
#13019 = DIRECTION ( 'NONE',  ( 0.000000000000000000, 1.000000000000000000, -1.067522139062650474E-15 ) ) ;
#13020 = CARTESIAN_POINT ( 'NONE',  ( 8.000000000000007105, -5.679790370316031733, 7.613867765417587030 ) ) ;
#13021 = DIRECTION ( 'NONE',  ( 0.000000000000000000, 0.000000000000000000, 1.000000000000000000 ) ) ;
#13022 = EDGE_CURVE ( 'NONE', #574, #28112, #33455, .T. ) ;
#13023 = ORIENTED_EDGE ( 'NONE', *, *, #12053, .F. ) ;
#13024 = FACE_OUTER_BOUND ( 'NONE', #18835, .T. ) ;
#13025 = CIRCLE ( 'NONE', #33142, 4.000000000000000000 ) ;
#13026 = CARTESIAN_POINT ( 'NONE',  ( -35.50000000000000711, -114.5974311500472425, -1.624782352598427959 ) ) ;
#13027 = DIRECTION ( 'NONE',  ( 0.000000000000000000, 0.9510565162951544194, -0.3090169943749448422 ) ) ;
#13028 = CARTESIAN_POINT ( 'NONE',  ( -35.50000000000000711, -114.9492820284331742, 10.20776876943783940 ) ) ;
#13029 = DIRECTION ( 'NONE',  ( -1.000000000000000000, 0.000000000000000000, 0.000000000000000000 ) ) ;
#13030 = ORIENTED_EDGE ( 'NONE', *, *, #5572, .T. ) ;
#13031 = CIRCLE ( 'NONE', #7847, 47.49900000000001654 ) ;
#13032 = CARTESIAN_POINT ( 'NONE',  ( -21.15833593587365513, -22.68172400785658382, 87.71410161513770731 ) ) ;
#13033 = CARTESIAN_POINT ( 'NONE',  ( -35.50000000000000000, -111.0168437565048691, 0.9961850632443862708 ) ) ;
#13034 = CARTESIAN_POINT ( 'NONE',  ( 65.00000000000001421, -25.98076211353320986, 77.99999999999992895 ) ) ;
#13035 = ORIENTED_EDGE ( 'NONE', *, *, #34064, .F. ) ;
#13036 = ORIENTED_EDGE ( 'NONE', *, *, #34637, .F. ) ;
#13037 = CIRCLE ( 'NONE', #972, 0.7500000000000039968 ) ;
#13038 = CARTESIAN_POINT ( 'NONE',  ( -36.52652403469556930, -113.0245472910329880, 7.222274454178449155 ) ) ;
#13039 = EDGE_CURVE ( 'NONE', #3468, #26771, #6092, .T. ) ;
#13040 = FILL_AREA_STYLE ('',( #2066 ) ) ;
#13041 = CIRCLE ( 'NONE', #26848, 52.00000000000000711 ) ;
#13042 = CARTESIAN_POINT ( 'NONE',  ( 7.999999999999992895, -44.47301969247457976, 16.68249143361895293 ) ) ;
#13043 = VERTEX_POINT ( 'NONE', #20640 ) ;
#13044 = ORIENTED_EDGE ( 'NONE', *, *, #32640, .F. ) ;
#13045 = CARTESIAN_POINT ( 'NONE',  ( -34.50000000000000000, -113.0140978167137717, 0.8903425666012282358 ) ) ;
#13046 = ADVANCED_FACE ( 'NONE', ( #15239 ), #26976, .T. ) ;
#13047 = EDGE_CURVE ( 'NONE', #33645, #2204, #28949, .T. ) ;
#13048 = CARTESIAN_POINT ( 'NONE',  ( 0.000000000000000000, 0.000000000000000000, 0.000000000000000000 ) ) ;
#13049 = VECTOR ( 'NONE', #18264, 1000.000000000000000 ) ;
#13050 = LINE ( 'NONE', #13230, #1300 ) ;
#13051 = CIRCLE ( 'NONE', #22228, 8.000000000000007105 ) ;
#13052 = AXIS2_PLACEMENT_3D ( 'NONE', #22878, #561, #6494 ) ;
#13053 = CARTESIAN_POINT ( 'NONE',  ( -37.99994980024369085, -114.9929510916434339, 12.62670525340494621 ) ) ;
#13054 = FACE_OUTER_BOUND ( 'NONE', #2460, .T. ) ;
#13055 = EDGE_CURVE ( 'NONE', #11602, #26957, #4298, .T. ) ;
#13056 = DIRECTION ( 'NONE',  ( 0.000000000000000000, 0.000000000000000000, 1.000000000000000000 ) ) ;
#13057 = EDGE_CURVE ( 'NONE', #23156, #28712, #13837, .T. ) ;
#13058 = CARTESIAN_POINT ( 'NONE',  ( -34.50000000000000000, -112.0140978167138712, -0.3122823525984337878 ) ) ;
#13059 = AXIS2_PLACEMENT_3D ( 'NONE', #34408, #7016, #34039 ) ;
#13060 = VECTOR ( 'NONE', #818, 1000.000000000000114 ) ;
#13061 = CARTESIAN_POINT ( 'NONE',  ( -4.000000000000000000, 0.000000000000000000, 55.00000000000000000 ) ) ;
#13062 = DIRECTION ( 'NONE',  ( -1.000000000000000000, 0.000000000000000000, 0.000000000000000000 ) ) ;
#13063 = CIRCLE ( 'NONE', #33180, 7.199999999999993960 ) ;
#13064 = DIRECTION ( 'NONE',  ( 1.000000000000000000, -1.110223024625156540E-16, 0.000000000000000000 ) ) ;
#13065 = ORIENTED_EDGE ( 'NONE', *, *, #23388, .T. ) ;
#13066 = CARTESIAN_POINT ( 'NONE',  ( -37.34375000000001421, -115.9929510916434481, 13.11852480586264846 ) ) ;
#13067 = CARTESIAN_POINT ( 'NONE',  ( -35.50000000000000711, -116.0060826362711595, -0.7553032835231661135 ) ) ;
#13068 = FACE_OUTER_BOUND ( 'NONE', #33882, .T. ) ;
#13069 = CARTESIAN_POINT ( 'NONE',  ( 4.000000000000003553, 13.42368113696682030, 3.975523202428055125 ) ) ;
#13070 = EDGE_CURVE ( 'NONE', #27693, #14516, #32246, .T. ) ;
#13071 = AXIS2_PLACEMENT_3D ( 'NONE', #10713, #26938, #5491 ) ;
#13072 = VERTEX_POINT ( 'NONE', #26613 ) ;
#13073 = CARTESIAN_POINT ( 'NONE',  ( -39.49999999999999289, -14.17619866229204106, 94.12476896299857287 ) ) ;
#13074 = DIRECTION ( 'NONE',  ( 0.000000000000000000, 0.000000000000000000, 1.000000000000000000 ) ) ;
#13075 = DIRECTION ( 'NONE',  ( 1.000000000000000000, 0.000000000000000000, 0.000000000000000000 ) ) ;
#13076 = DIRECTION ( 'NONE',  ( 1.000000000000000000, 1.734723475976807094E-16, 0.000000000000000000 ) ) ;
#13077 = CARTESIAN_POINT ( 'NONE',  ( -36.64504884055823908, -115.0245472910329880, 3.284774454178449155 ) ) ;
#13078 = CARTESIAN_POINT ( 'NONE',  ( -39.49999999999999289, 0.4463568765849662556, 113.0433323525902125 ) ) ;
#13079 = CARTESIAN_POINT ( 'NONE',  ( 0.000000000000000000, 0.000000000000000000, 0.000000000000000000 ) ) ;
#13080 = ORIENTED_EDGE ( 'NONE', *, *, #21096, .T. ) ;
#13081 = CIRCLE ( 'NONE', #26883, 4.800000000000006040 ) ;
#13082 = ORIENTED_EDGE ( 'NONE', *, *, #24880, .T. ) ;
#13083 = DIRECTION ( 'NONE',  ( -1.000000000000000000, 0.000000000000000000, 0.000000000000000000 ) ) ;
#13084 = AXIS2_PLACEMENT_3D ( 'NONE', #16248, #13401, #11055 ) ;
#13085 = CARTESIAN_POINT ( 'NONE',  ( -1.519999999999992912, -4.846123502488801633E-16, -6.984000000000015085 ) ) ;
#13086 = LINE ( 'NONE', #26585, #15646 ) ;
#13087 = ORIENTED_EDGE ( 'NONE', *, *, #29115, .T. ) ;
#13088 = CARTESIAN_POINT ( 'NONE',  ( -37.05926240293131713, -112.0000000000000142, 6.621475545821550845 ) ) ;
#13089 = ORIENTED_EDGE ( 'NONE', *, *, #21096, .F. ) ;
#13090 = VECTOR ( 'NONE', #33810, 1000.000000000000000 ) ;
#13091 = CIRCLE ( 'NONE', #22820, 9.499000000000012989 ) ;
#13092 = EDGE_CURVE ( 'NONE', #21954, #9760, #31639, .T. ) ;
#13093 = ORIENTED_EDGE ( 'NONE', *, *, #31775, .F. ) ;
#13094 = ORIENTED_EDGE ( 'NONE', *, *, #20227, .F. ) ;
#13095 = CIRCLE ( 'NONE', #9059, 8.000000000000007105 ) ;
#13096 = DIRECTION ( 'NONE',  ( 1.000000000000000000, -0.000000000000000000, -0.000000000000000000 ) ) ;
#13097 = ADVANCED_FACE ( 'NONE', ( #1948 ), #26789, .T. ) ;
#13098 = VECTOR ( 'NONE', #27328, 1000.000000000000000 ) ;
#13099 = AXIS2_PLACEMENT_3D ( 'NONE', #5068, #34636, #8454 ) ;
#13100 = DIRECTION ( 'NONE',  ( 0.000000000000000000, 0.000000000000000000, 1.000000000000000000 ) ) ;
#13101 = VERTEX_POINT ( 'NONE', #12924 ) ;
#13102 = VERTEX_POINT ( 'NONE', #31818 ) ;
#13103 = CARTESIAN_POINT ( 'NONE',  ( 0.000000000000000000, 0.000000000000000000, -33.50000000000000711 ) ) ;
#13104 = DIRECTION ( 'NONE',  ( -1.000000000000000000, -1.836970198721029934E-16, -0.000000000000000000 ) ) ;
#13105 = EDGE_CURVE ( 'NONE', #21428, #8016, #23908, .T. ) ;
#13106 = CARTESIAN_POINT ( 'NONE',  ( -44.00000000000000000, 10.99999999999999289, 1.347111479062087616E-15 ) ) ;
#13107 = EDGE_CURVE ( 'NONE', #23058, #16691, #26502, .T. ) ;
#13108 = AXIS2_PLACEMENT_3D ( 'NONE', #26889, #24175, #10851 ) ;
#13109 = CYLINDRICAL_SURFACE ( 'NONE', #35517, 20.00000000000000355 ) ;
#13110 = LINE ( 'NONE', #4655, #1821 ) ;
#13111 = CIRCLE ( 'NONE', #32624, 47.49900000000000944 ) ;
#13112 = CARTESIAN_POINT ( 'NONE',  ( 8.000000000000000000, 0.000000000000000000, 0.000000000000000000 ) ) ;
#13113 = CARTESIAN_POINT ( 'NONE',  ( -34.97545270896703329, -113.2308352781851397, 5.909774454178449155 ) ) ;
#13114 = CARTESIAN_POINT ( 'NONE',  ( -34.50300906734826611, -115.9929510916434481, 12.71660600561482468 ) ) ;
#13115 = CARTESIAN_POINT ( 'NONE',  ( 0.000000000000000000, -9.508666619816507293, -19.83898331853700370 ) ) ;
#13116 = CIRCLE ( 'NONE', #1612, 20.00000000000000711 ) ;
#13117 = DIRECTION ( 'NONE',  ( 0.000000000000000000, 0.000000000000000000, 1.000000000000000000 ) ) ;
#13118 = AXIS2_PLACEMENT_3D ( 'NONE', #23565, #10427, #1791 ) ;
#13119 = LINE ( 'NONE', #26791, #18155 ) ;
#13120 = FACE_OUTER_BOUND ( 'NONE', #22525, .T. ) ;
#13121 = CYLINDRICAL_SURFACE ( 'NONE', #22764, 19.99999999999998579 ) ;
#13122 = CYLINDRICAL_SURFACE ( 'NONE', #25308, 52.00000000000000711 ) ;
#13123 = VERTEX_POINT ( 'NONE', #15423 ) ;
#13124 = CARTESIAN_POINT ( 'NONE',  ( -38.37230871539094323, -115.4561184093552413, 6.058975545821551734 ) ) ;
#13125 =( GEOMETRIC_REPRESENTATION_CONTEXT ( 3 ) GLOBAL_UNCERTAINTY_ASSIGNED_CONTEXT ( ( #25139 ) ) GLOBAL_UNIT_ASSIGNED_CONTEXT ( ( #7166, #20654, #4136 ) ) REPRESENTATION_CONTEXT ( 'NONE', 'WORKASPACE' ) );
#13126 = DIRECTION ( 'NONE',  ( 0.000000000000000000, 0.000000000000000000, 1.000000000000000000 ) ) ;
#13127 = CARTESIAN_POINT ( 'NONE',  ( 0.000000000000000000, -8.128228055638974325, 16.94522934049209795 ) ) ;
#13128 = ORIENTED_EDGE ( 'NONE', *, *, #12817, .F. ) ;
#13129 = VERTEX_POINT ( 'NONE', #18315 ) ;
#13130 = DIRECTION ( 'NONE',  ( -1.000000000000000000, 0.000000000000000000, -0.000000000000000000 ) ) ;
#13131 = CYLINDRICAL_SURFACE ( 'NONE', #8862, 20.00000000000000711 ) ;
#13132 = ORIENTED_EDGE ( 'NONE', *, *, #31733, .F. ) ;
#13133 = ORIENTED_EDGE ( 'NONE', *, *, #29426, .F. ) ;
#13134 = EDGE_CURVE ( 'NONE', #5612, #18458, #7511, .T. ) ;
#13135 = DIRECTION ( 'NONE',  ( 0.000000000000000000, 0.000000000000000000, 1.000000000000000000 ) ) ;
#13136 = DIRECTION ( 'NONE',  ( 1.000000000000000000, 1.734723475976807094E-16, 0.000000000000000000 ) ) ;
#13137 = AXIS2_PLACEMENT_3D ( 'NONE', #34034, #34212, #17806 ) ;
#13138 = DIRECTION ( 'NONE',  ( -0.000000000000000000, -0.000000000000000000, -1.000000000000000000 ) ) ;
#13139 = DIRECTION ( 'NONE',  ( 0.000000000000000000, -1.000000000000000000, 0.000000000000000000 ) ) ;
#13140 = ORIENTED_EDGE ( 'NONE', *, *, #27073, .F. ) ;
#13141 = ORIENTED_EDGE ( 'NONE', *, *, #29590, .F. ) ;
#13142 = CARTESIAN_POINT ( 'NONE',  ( -35.50000000000000711, -113.2637153405686519, 1.912112492696748989 ) ) ;
#13143 = AXIS2_PLACEMENT_3D ( 'NONE', #7136, #31801, #5128 ) ;
#13144 =( REPRESENTATION_RELATIONSHIP ('NONE','NONE', #26607, #22901 ) REPRESENTATION_RELATIONSHIP_WITH_TRANSFORMATION ( #256 )SHAPE_REPRESENTATION_RELATIONSHIP( ) );
#13145 = CARTESIAN_POINT ( 'NONE',  ( 54.99999999999999289, -64.99999999999997158, 120.0000000000000000 ) ) ;
#13146 = CARTESIAN_POINT ( 'NONE',  ( -54.99999999999998579, -64.99999999999997158, -25.00000000000000000 ) ) ;
#13147 = VERTEX_POINT ( 'NONE', #34713 ) ;
#13148 = AXIS2_PLACEMENT_3D ( 'NONE', #22433, #3386, #24980 ) ;
#13149 = CARTESIAN_POINT ( 'NONE',  ( 55.00000000000000000, -25.98076211353320275, 90.99999999999994316 ) ) ;
#13150 = CARTESIAN_POINT ( 'NONE',  ( 0.000000000000000000, 15.49408907645234734, -44.90087086784577508 ) ) ;
#13151 = CARTESIAN_POINT ( 'NONE',  ( -35.07817881376918479, -114.9929510916434339, 13.81802396319203297 ) ) ;
#13152 = DIRECTION ( 'NONE',  ( 0.000000000000000000, -6.938893903907203726E-17, -1.000000000000000000 ) ) ;
#13153 = CARTESIAN_POINT ( 'NONE',  ( -37.99959864031215773, -114.9929510916434339, 12.63896776382213538 ) ) ;
#13154 = CARTESIAN_POINT ( 'NONE',  ( 8.000000000000007105, 9.919332006307387317, -5.363026430117004750 ) ) ;
#13155 = CARTESIAN_POINT ( 'NONE',  ( -34.50000000000000000, -114.1489256397697289, 9.518467544735724317 ) ) ;
#13156 = LINE ( 'NONE', #20858, #14234 ) ;
#13157 = CARTESIAN_POINT ( 'NONE',  ( 1.398397006337009918, -6.091550361990587525, 0.000000000000000000 ) ) ;
#13158 = CARTESIAN_POINT ( 'NONE',  ( 7.999999999999992895, 11.46872990052444408, -45.56340405422432127 ) ) ;
#13159 = EDGE_LOOP ( 'NONE', ( #15273, #2919, #13386, #2782 ) ) ;
#13160 = CARTESIAN_POINT ( 'NONE',  ( 8.000000000000000000, -16.71027810728550733, -2.620268201066114688 ) ) ;
#13161 = CARTESIAN_POINT ( 'NONE',  ( 7.999999999999992895, 0.000000000000000000, 0.000000000000000000 ) ) ;
#13162 = ORIENTED_EDGE ( 'NONE', *, *, #11535, .T. ) ;
#13163 = CARTESIAN_POINT ( 'NONE',  ( -38.00000000000000711, -114.9929510916434339, 12.60752341388803721 ) ) ;
#13164 = EDGE_LOOP ( 'NONE', ( #21377, #25919, #18083, #15221 ) ) ;
#13165 = CIRCLE ( 'NONE', #26365, 4.000000000000000000 ) ;
#13166 = CARTESIAN_POINT ( 'NONE',  ( -38.45611840935523418, -115.3723087153909432, 5.066024454178449155 ) ) ;
#13167 = AXIS2_PLACEMENT_3D ( 'NONE', #2224, #18925, #27585 ) ;
#13168 = CARTESIAN_POINT ( 'NONE',  ( 4.000000000000003553, -39.64889472655756464, 33.64468972902493960 ) ) ;
#13169 = ORIENTED_EDGE ( 'NONE', *, *, #9901, .F. ) ;
#13170 = AXIS2_PLACEMENT_3D ( 'NONE', #31758, #23668, #34654 ) ;
#13171 = VERTEX_POINT ( 'NONE', #21000 ) ;
#13172 = CARTESIAN_POINT ( 'NONE',  ( 0.000000000000000000, 0.000000000000000000, 0.000000000000000000 ) ) ;
#13173 = ORIENTED_EDGE ( 'NONE', *, *, #35575, .F. ) ;
#13174 = CARTESIAN_POINT ( 'NONE',  ( -35.81662171581204746, -117.0245472910329738, 4.784774454178448266 ) ) ;
#13175 = DIRECTION ( 'NONE',  ( 1.000000000000000000, -0.000000000000000000, -0.000000000000000000 ) ) ;
#13176 = ADVANCED_FACE ( 'NONE', ( #34901 ), #17948, .T. ) ;
#13177 = CARTESIAN_POINT ( 'NONE',  ( -35.50000000000000711, -116.0140978167138712, 0.3752176474015736507 ) ) ;
#13178 = ORIENTED_EDGE ( 'NONE', *, *, #4919, .T. ) ;
#13179 = ORIENTED_EDGE ( 'NONE', *, *, #29883, .F. ) ;
#13180 = CARTESIAN_POINT ( 'NONE',  ( 70.00001200000002655, -25.45716333793490094, 80.99999999999991473 ) ) ;
#13181 =( LENGTH_UNIT ( ) NAMED_UNIT ( * ) SI_UNIT ( .MILLI., .METRE. ) );
#13182 = DIRECTION ( 'NONE',  ( -1.000000000000000000, 0.000000000000000000, 0.000000000000000000 ) ) ;
#13183 = ORIENTED_EDGE ( 'NONE', *, *, #1981, .F. ) ;
#13184 = ORIENTED_EDGE ( 'NONE', *, *, #5799, .T. ) ;
#13185 = CARTESIAN_POINT ( 'NONE',  ( -34.50000000000000000, -112.6882700046066645, -2.599147725882136939 ) ) ;
#13186 = AXIS2_PLACEMENT_3D ( 'NONE', #31051, #20045, #22401 ) ;
#13187 = ADVANCED_FACE ( 'NONE', ( #9685 ), #10037, .T. ) ;
#13188 = CARTESIAN_POINT ( 'NONE',  ( -4.000000000000000000, -2.710505431213761085E-17, -46.00000000000000000 ) ) ;
#13189 = VERTEX_POINT ( 'NONE', #7510 ) ;
#13190 = CARTESIAN_POINT ( 'NONE',  ( -35.50000000000000711, -114.1068310684433129, 9.512752019463897923 ) ) ;
#13191 = CIRCLE ( 'NONE', #3425, 52.00000000000000711 ) ;
#13192 = CARTESIAN_POINT ( 'NONE',  ( -38.00000000000000711, -113.9929510916434339, 10.50625754673587053 ) ) ;
#13193 = DIRECTION ( 'NONE',  ( -1.000000000000000000, 0.000000000000000000, 0.000000000000000000 ) ) ;
#13194 = CARTESIAN_POINT ( 'NONE',  ( -46.00000000000000000, 9.797174393178825657E-16, -8.000000000000000000 ) ) ;
#13195 = CARTESIAN_POINT ( 'NONE',  ( -37.93687354226506869, -113.9929510916434339, 12.87038173996323565 ) ) ;
#13196 = CARTESIAN_POINT ( 'NONE',  ( -36.31249999999994316, -115.9929510916434481, 13.11852480586264846 ) ) ;
#13197 = CARTESIAN_POINT ( 'NONE',  ( 0.000000000000000000, 21.63912866391140710, 3.968388925834887893 ) ) ;
#13198 = DIRECTION ( 'NONE',  ( -1.000000000000000000, 0.000000000000000000, 0.000000000000000000 ) ) ;
#13199 = ORIENTED_EDGE ( 'NONE', *, *, #63, .F. ) ;
#13200 = DIRECTION ( 'NONE',  ( -1.000000000000000000, 0.000000000000000000, 0.000000000000000000 ) ) ;
#13201 = DIRECTION ( 'NONE',  ( -1.000000000000000000, 0.000000000000000000, 0.000000000000000000 ) ) ;
#13202 = CARTESIAN_POINT ( 'NONE',  ( 8.000000000000000000, 16.31134495048485178, 6.336799421339877725 ) ) ;
#13203 = ADVANCED_FACE ( 'NONE', ( #4663 ), #10226, .T. ) ;
#13204 = EDGE_LOOP ( 'NONE', ( #32507, #17025, #8298, #32924, #3519, #17491, #940, #26468, #32033, #20159, #1554, #15945, #32700, #5989, #4629, #21832, #29940, #28483, #15743, #10468, #13708, #26327, #12007, #9654, #25052, #20721, #33590, #4727, #22453, #11470, #5206, #25517, #21744, #30163, #2104, #17503, #6259, #10591, #13547, #23638, #18816, #29289, #24398, #17619, #18951, #27134, #30553, #2348, #19973, #4313, #35069, #23152, #28873, #2995, #12733, #7022, #8540, #24118, #23422, #26866, #18783, #26308, #6209, #7654, #18105, #10284, #4753, #32411, #8494, #16941, #33930, #3126, #32331, #6147, #3974, #1507, #30957, #33532, #3564, #13596, #20804, #33600, #26236, #2912, #20531 ) ) ;
#13205 = CARTESIAN_POINT ( 'NONE',  ( 0.000000000000000000, 0.000000000000000000, 0.000000000000000000 ) ) ;
#13206 = CARTESIAN_POINT ( 'NONE',  ( -35.50000000000000000, -113.0140978167140702, 0.8752176474015603835 ) ) ;
#13207 = DIRECTION ( 'NONE',  ( 0.000000000000000000, 0.000000000000000000, 1.000000000000000000 ) ) ;
#13208 = CIRCLE ( 'NONE', #17180, 15.49899999999998812 ) ;
#13209 = CARTESIAN_POINT ( 'NONE',  ( -35.50400759022159036, -114.9929510916434339, 12.68378527132497524 ) ) ;
#13210 = LINE ( 'NONE', #2055, #33175 ) ;
#13211 = EDGE_LOOP ( 'NONE', ( #13369, #4555, #15620, #3914 ) ) ;
#13212 = AXIS2_PLACEMENT_3D ( 'NONE', #13836, #505, #32925 ) ;
#13213 = DIRECTION ( 'NONE',  ( -1.000000000000000000, -0.000000000000000000, -0.000000000000000000 ) ) ;
#13214 = ADVANCED_FACE ( 'NONE', ( #6976 ), #18492, .T. ) ;
#13215 = CARTESIAN_POINT ( 'NONE',  ( -35.50000000000000000, -112.7319952733504635, 2.855726801009121463 ) ) ;
#13216 = VERTEX_POINT ( 'NONE', #30377 ) ;
#13217 = ORIENTED_EDGE ( 'NONE', *, *, #22705, .F. ) ;
#13218 = EDGE_CURVE ( 'NONE', #2874, #19260, #25337, .T. ) ;
#13219 = CARTESIAN_POINT ( 'NONE',  ( -36.94073759706868287, -112.0000000000000142, 2.628524454178448710 ) ) ;
#13220 = EDGE_CURVE ( 'NONE', #21073, #24111, #9799, .T. ) ;
#13221 = AXIS2_PLACEMENT_3D ( 'NONE', #25417, #30467, #9194 ) ;
#13222 = SURFACE_STYLE_USAGE ( .BOTH. , #13563 ) ;
#13223 = DIRECTION ( 'NONE',  ( 0.02857142857143298714, -0.9995917534020514195, -4.555780455966493806E-16 ) ) ;
#13224 = ORIENTED_EDGE ( 'NONE', *, *, #24076, .T. ) ;
#13225 = ORIENTED_EDGE ( 'NONE', *, *, #16234, .T. ) ;
#13226 = CARTESIAN_POINT ( 'NONE',  ( -34.50000000000000000, -113.0140978167138712, 0.5627176474015715968 ) ) ;
#13227 = EDGE_CURVE ( 'NONE', #33344, #18371, #18430, .T. ) ;
#13228 = DIRECTION ( 'NONE',  ( 0.000000000000000000, 0.000000000000000000, 1.000000000000000000 ) ) ;
#13229 = ADVANCED_FACE ( 'NONE', ( #32894 ), #8042, .F. ) ;
#13230 = CARTESIAN_POINT ( 'NONE',  ( 4.000000000000003553, 3.975523202428290936, -13.42368113696666754 ) ) ;
#13231 = CARTESIAN_POINT ( 'NONE',  ( -37.52044295795950291, -114.9929510916434339, 13.11812344617477244 ) ) ;
#13232 = DIRECTION ( 'NONE',  ( 0.000000000000000000, -1.000000000000000000, 0.000000000000000000 ) ) ;
#13233 = LINE ( 'NONE', #16430, #13630 ) ;
#13234 = CARTESIAN_POINT ( 'NONE',  ( -34.50000000000000000, -112.0140978167138712, 0.3752176474015640473 ) ) ;
#13235 = FACE_OUTER_BOUND ( 'NONE', #24770, .T. ) ;
#13236 = CIRCLE ( 'NONE', #20676, 52.00000000000000711 ) ;
#13237 = LINE ( 'NONE', #18259, #16874 ) ;
#13238 = VERTEX_POINT ( 'NONE', #19194 ) ;
#13239 = PRESENTATION_LAYER_ASSIGNMENT (  '', '', ( #24727 ) ) ;
#13240 =( GEOMETRIC_REPRESENTATION_CONTEXT ( 3 ) GLOBAL_UNCERTAINTY_ASSIGNED_CONTEXT ( ( #9534 ) ) GLOBAL_UNIT_ASSIGNED_CONTEXT ( ( #32736, #11130, #33095 ) ) REPRESENTATION_CONTEXT ( 'NONE', 'WORKASPACE' ) );
#13241 = CARTESIAN_POINT ( 'NONE',  ( -37.99899697755054717, -115.9929510916434481, 12.65121853911336913 ) ) ;
#13242 = DIRECTION ( 'NONE',  ( -1.000000000000000000, 0.000000000000000000, 0.000000000000000000 ) ) ;
#13243 = CARTESIAN_POINT ( 'NONE',  ( 75.00000000000001421, -27.93100416606583991, 81.50764321173598148 ) ) ;
#13244 = VECTOR ( 'NONE', #8944, 1000.000000000000000 ) ;
#13245 = LINE ( 'NONE', #27640, #32938 ) ;
#13246 = EDGE_CURVE ( 'NONE', #31873, #12235, #34536, .T. ) ;
#13247 = DIRECTION ( 'NONE',  ( 1.000000000000000000, -0.000000000000000000, -0.000000000000000000 ) ) ;
#13248 = VERTEX_POINT ( 'NONE', #30193 ) ;
#13249 = CARTESIAN_POINT ( 'NONE',  ( 0.000000000000000000, -15.92965478239629817, 15.17386234660378008 ) ) ;
#13250 = CARTESIAN_POINT ( 'NONE',  ( 0.000000000000000000, -13.85708833600000744, 45.43276465116660745 ) ) ;
#13251 = PRODUCT_RELATED_PRODUCT_CATEGORY ( 'part', '', ( #29075 ) ) ;
#13252 = DIRECTION ( 'NONE',  ( 0.000000000000000000, 0.000000000000000000, 1.000000000000000000 ) ) ;
#13253 = LINE ( 'NONE', #2099, #15519 ) ;
#13254 = CARTESIAN_POINT ( 'NONE',  ( -1.000000000000014655, -4.808326913196006913, 0.000000000000000000 ) ) ;
#13255 = DIRECTION ( 'NONE',  ( 0.000000000000000000, 0.000000000000000000, 1.000000000000000000 ) ) ;
#13256 = ORIENTED_EDGE ( 'NONE', *, *, #10829, .T. ) ;
#13257 = ORIENTED_EDGE ( 'NONE', *, *, #23440, .F. ) ;
#13258 = CARTESIAN_POINT ( 'NONE',  ( 0.000000000000000000, 0.000000000000000000, 0.000000000000000000 ) ) ;
#13259 = ADVANCED_FACE ( 'NONE', ( #10574 ), #3016, .T. ) ;
#13260 = CARTESIAN_POINT ( 'NONE',  ( 7.999999999999992895, 39.78933988720114456, 24.98727647985016276 ) ) ;
#13261 = DIRECTION ( 'NONE',  ( -1.226634733346697831E-16, -0.7071067811865507924, 0.7071067811865441310 ) ) ;
#13262 = ORIENTED_EDGE ( 'NONE', *, *, #22014, .T. ) ;
#13263 = EDGE_CURVE ( 'NONE', #23156, #12650, #26841, .T. ) ;
#13264 = AXIS2_PLACEMENT_3D ( 'NONE', #13573, #34837, #26737 ) ;
#13265 = CARTESIAN_POINT ( 'NONE',  ( -34.97545270896703329, -114.7691647218148745, 5.590225545821552622 ) ) ;
#13266 = ADVANCED_FACE ( 'NONE', ( #24966 ), #290, .T. ) ;
#13267 = ORIENTED_EDGE ( 'NONE', *, *, #15244, .F. ) ;
#13268 = ORIENTED_EDGE ( 'NONE', *, *, #17822, .T. ) ;
#13269 = AXIS2_PLACEMENT_3D ( 'NONE', #18849, #2485, #24793 ) ;
#13270 = EDGE_LOOP ( 'NONE', ( #4844, #9947, #34951, #27783 ) ) ;
#13271 = CYLINDRICAL_SURFACE ( 'NONE', #9698, 6.000000000000005329 ) ;
#13272 = VECTOR ( 'NONE', #27471, 1000.000000000000000 ) ;
#13273 = ADVANCED_FACE ( 'NONE', ( #35604, #16128 ), #22076, .F. ) ;
#13274 = DIRECTION ( 'NONE',  ( 0.000000000000000000, 2.423959199780483078E-15, -1.000000000000000000 ) ) ;
#13275 = EDGE_LOOP ( 'NONE', ( #10189, #8134 ) ) ;
#13276 = VERTEX_POINT ( 'NONE', #10933 ) ;
#13277 = DIRECTION ( 'NONE',  ( 0.1305261922200512403, -0.9914448613738104932, 6.326001338775677127E-32 ) ) ;
#13278 = CARTESIAN_POINT ( 'NONE',  ( 8.000000000000000000, 0.000000000000000000, 0.000000000000000000 ) ) ;
#13279 = DIRECTION ( 'NONE',  ( 0.000000000000000000, 0.000000000000000000, -1.000000000000000000 ) ) ;
#13280 = DIRECTION ( 'NONE',  ( 0.000000000000000000, 0.000000000000000000, -1.000000000000000000 ) ) ;
#13281 = DIRECTION ( 'NONE',  ( 1.000000000000000000, -0.000000000000000000, 0.000000000000000000 ) ) ;
#13282 = AXIS2_PLACEMENT_3D ( 'NONE', #20010, #17313, #24913 ) ;
#13283 = CARTESIAN_POINT ( 'NONE',  ( -38.37230871539094323, -112.5438815906447729, 5.441024454178449155 ) ) ;
#13284 = CARTESIAN_POINT ( 'NONE',  ( -34.50000000000000000, -115.9056129652226872, 9.909279992139808257 ) ) ;
#13285 = CARTESIAN_POINT ( 'NONE',  ( -39.49999999999999289, -5.633167542791597704, 143.9590043477703887 ) ) ;
#13286 = EDGE_CURVE ( 'NONE', #26760, #21695, #28544, .T. ) ;
#13287 = DIRECTION ( 'NONE',  ( 1.000000000000000000, 0.000000000000000000, 0.000000000000000000 ) ) ;
#13288 = CARTESIAN_POINT ( 'NONE',  ( 0.000000000000000000, -2.710505431213761085E-17, 55.00000000000000000 ) ) ;
#13289 = DIRECTION ( 'NONE',  ( 0.000000000000000000, 0.000000000000000000, 1.000000000000000000 ) ) ;
#13290 = EDGE_CURVE ( 'NONE', #10684, #11623, #23986, .T. ) ;
#13291 = CARTESIAN_POINT ( 'NONE',  ( 38.00000000000000000, -10.49999999999999112, 0.000000000000000000 ) ) ;
#13292 = CARTESIAN_POINT ( 'NONE',  ( 8.000000000000000000, 12.49559743815794199, -9.169462670380459812 ) ) ;
#13293 = ORIENTED_EDGE ( 'NONE', *, *, #20765, .T. ) ;
#13294 = CIRCLE ( 'NONE', #4102, 20.00000000000001421 ) ;
#13295 =( GEOMETRIC_REPRESENTATION_CONTEXT ( 3 ) GLOBAL_UNCERTAINTY_ASSIGNED_CONTEXT ( ( #11750 ) ) GLOBAL_UNIT_ASSIGNED_CONTEXT ( ( #27484, #33052, #15936 ) ) REPRESENTATION_CONTEXT ( 'NONE', 'WORKASPACE' ) );
#13296 = CARTESIAN_POINT ( 'NONE',  ( -38.99999999999999289, -114.0592624029313242, 3.246475545821551734 ) ) ;
#13297 = CARTESIAN_POINT ( 'NONE',  ( 8.000000000000000000, -15.17386234660395417, 15.92965478239613830 ) ) ;
#13298 = DIRECTION ( 'NONE',  ( -1.000000000000000000, 0.000000000000000000, -0.000000000000000000 ) ) ;
#13299 = AXIS2_PLACEMENT_3D ( 'NONE', #27529, #10955, #21921 ) ;
#13300 = ORIENTED_EDGE ( 'NONE', *, *, #21511, .F. ) ;
#13301 = VERTEX_POINT ( 'NONE', #5359 ) ;
#13302 = CARTESIAN_POINT ( 'NONE',  ( -39.49999999999999289, -5.633167542791597704, 121.0048025873810218 ) ) ;
#13303 = DIRECTION ( 'NONE',  ( 0.000000000000000000, 0.000000000000000000, 1.000000000000000000 ) ) ;
#13304 = ORIENTED_EDGE ( 'NONE', *, *, #14514, .T. ) ;
#13305 = ADVANCED_FACE ( 'NONE', ( #21527 ), #5873, .T. ) ;
#13306 = ORIENTED_EDGE ( 'NONE', *, *, #19602, .T. ) ;
#13307 = EDGE_CURVE ( 'NONE', #21774, #26100, #16303, .T. ) ;
#13308 = CARTESIAN_POINT ( 'NONE',  ( -9.999999999999994671, 0.000000000000000000, 0.000000000000000000 ) ) ;
#13309 = DIRECTION ( 'NONE',  ( 0.000000000000000000, 0.000000000000000000, 1.000000000000000000 ) ) ;
#13310 = CARTESIAN_POINT ( 'NONE',  ( -6.938893903907228378E-15, 8.673617379884035472E-16, 70.00000000000000000 ) ) ;
#13311 = FACE_OUTER_BOUND ( 'NONE', #33437, .T. ) ;
#13312 = VERTEX_POINT ( 'NONE', #19369 ) ;
#13313 = EDGE_LOOP ( 'NONE', ( #4733, #7448, #34111, #8761 ) ) ;
#13314 = CARTESIAN_POINT ( 'NONE',  ( -35.50000000000000711, -112.2144317118258527, -1.239329810084414341 ) ) ;
#13315 = DIRECTION ( 'NONE',  ( 1.000000000000000000, -5.339440136655842133E-16, -1.047965281155519420E-16 ) ) ;
#13316 = CARTESIAN_POINT ( 'NONE',  ( 8.000000000000000000, 8.128228055638880178, 16.94522934049213347 ) ) ;
#13317 = VECTOR ( 'NONE', #22520, 1000.000000000000000 ) ;
#13318 = ORIENTED_EDGE ( 'NONE', *, *, #32639, .F. ) ;
#13319 = DIRECTION ( 'NONE',  ( -1.000000000000000000, -0.000000000000000000, -0.000000000000000000 ) ) ;
#13320 = CARTESIAN_POINT ( 'NONE',  ( -34.50000000000000000, -116.0124910254613297, -0.6902086197697608894 ) ) ;
#13321 = CARTESIAN_POINT ( 'NONE',  ( -35.93867112612154813, -114.9929510916434339, 14.11732072679899197 ) ) ;
#13322 = CARTESIAN_POINT ( 'NONE',  ( -49.99999999999999289, -25.98076211353320275, 84.99999999999994316 ) ) ;
#13323 = CARTESIAN_POINT ( 'NONE',  ( -35.50000000000000000, -113.9929510916434339, 10.55026311463432087 ) ) ;
#13324 = CARTESIAN_POINT ( 'NONE',  ( 0.000000000000000000, 8.128228055639098670, -16.94522934049206242 ) ) ;
#13325 = CARTESIAN_POINT ( 'NONE',  ( -34.50000000000000000, -114.1021862393805577, 9.512197583835053649 ) ) ;
#13326 = FACE_OUTER_BOUND ( 'NONE', #18286, .T. ) ;
#13327 = EDGE_CURVE ( 'NONE', #9081, #21954, #8998, .T. ) ;
#13328 = CARTESIAN_POINT ( 'NONE',  ( -38.00000000000000711, -114.9929510916434339, 12.57451923796417503 ) ) ;
#13329 = CARTESIAN_POINT ( 'NONE',  ( 0.000000000000000000, 0.000000000000000000, 0.000000000000000000 ) ) ;
#13330 = ORIENTED_EDGE ( 'NONE', *, *, #383, .T. ) ;
#13331 = DIRECTION ( 'NONE',  ( 0.000000000000000000, 0.000000000000000000, 1.000000000000000000 ) ) ;
#13332 = DIRECTION ( 'NONE',  ( 1.000000000000000000, -0.000000000000000000, -0.000000000000000000 ) ) ;
#13333 = ADVANCED_FACE ( 'NONE', ( #10752 ), #2664, .T. ) ;
#13334 = ORIENTED_EDGE ( 'NONE', *, *, #13609, .F. ) ;
#13335 = CARTESIAN_POINT ( 'NONE',  ( -38.00000000000000711, -114.9929510916434339, 12.26648026267477043 ) ) ;
#13336 = VERTEX_POINT ( 'NONE', #14667 ) ;
#13337 = CARTESIAN_POINT ( 'NONE',  ( -35.02454729103298803, -114.8876895276775087, 4.597274454178448266 ) ) ;
#13338 = CYLINDRICAL_SURFACE ( 'NONE', #14059, 20.00000000000000355 ) ;
#13339 = ORIENTED_EDGE ( 'NONE', *, *, #1421, .T. ) ;
#13340 = ORIENTED_EDGE ( 'NONE', *, *, #18487, .T. ) ;
#13341 = CARTESIAN_POINT ( 'NONE',  ( 0.000000000000000000, 0.000000000000000000, 0.000000000000000000 ) ) ;
#13342 = FACE_OUTER_BOUND ( 'NONE', #2023, .T. ) ;
#13343 = AXIS2_PLACEMENT_3D ( 'NONE', #23447, #23987, #34980 ) ;
#13344 = ORIENTED_EDGE ( 'NONE', *, *, #34549, .T. ) ;
#13345 = CIRCLE ( 'NONE', #33444, 7.000000000000035527 ) ;
#13346 = CARTESIAN_POINT ( 'NONE',  ( -39.07941549657748936, -111.8367748094582055, 5.441024454178449155 ) ) ;
#13347 = CARTESIAN_POINT ( 'NONE',  ( -26.99999999999998579, -45.00000000000000000, 0.000000000000000000 ) ) ;
#13348 = DIRECTION ( 'NONE',  ( -0.000000000000000000, 0.000000000000000000, -1.000000000000000000 ) ) ;
#13349 = VERTEX_POINT ( 'NONE', #25866 ) ;
#13350 = VERTEX_POINT ( 'NONE', #22591 ) ;
#13351 = CARTESIAN_POINT ( 'NONE',  ( 0.000000000000000000, -2.710505431213761085E-17, 55.00000000000000000 ) ) ;
#13352 = DIRECTION ( 'NONE',  ( 1.000000000000000000, -0.000000000000000000, -0.000000000000000000 ) ) ;
#13353 = ORIENTED_EDGE ( 'NONE', *, *, #12376, .F. ) ;
#13354 = VERTEX_POINT ( 'NONE', #14316 ) ;
#13355 = AXIS2_PLACEMENT_3D ( 'NONE', #4083, #1906, #1718 ) ;
#13356 = CARTESIAN_POINT ( 'NONE',  ( -34.50000000000000000, -112.1946304249441795, 2.703640693953100804 ) ) ;
#13357 = CARTESIAN_POINT ( 'NONE',  ( -39.49999999999999289, -5.633167542791597704, 143.9590043477703887 ) ) ;
#13358 = ORIENTED_EDGE ( 'NONE', *, *, #17655, .T. ) ;
#13359 = CARTESIAN_POINT ( 'NONE',  ( -35.50000000000000711, -114.0000000000003411, 9.500000000000035527 ) ) ;
#13360 = CARTESIAN_POINT ( 'NONE',  ( -38.00000000000000711, -113.9929510916434339, 12.59652202191340820 ) ) ;
#13361 = CARTESIAN_POINT ( 'NONE',  ( 8.000000000000007105, 10.15474465512060398, 9.637487275701170475 ) ) ;
#13362 = DIRECTION ( 'NONE',  ( 0.000000000000000000, -0.3681245526846654292, -0.9297764858882563432 ) ) ;
#13363 = AXIS2_PLACEMENT_3D ( 'NONE', #30707, #27834, #14304 ) ;
#13364 = CARTESIAN_POINT ( 'NONE',  ( -37.66108410722335265, -113.9929510916434339, 13.09299768411426612 ) ) ;
#13365 = CARTESIAN_POINT ( 'NONE',  ( -37.51635661748575501, -115.9929510916434481, 13.11827392651459512 ) ) ;
#13366 = DIRECTION ( 'NONE',  ( 1.000000000000000000, 0.000000000000000000, 0.000000000000000000 ) ) ;
#13367 = CARTESIAN_POINT ( 'NONE',  ( -55.00000000000000000, 0.000000000000000000, 70.00000000000000000 ) ) ;
#13368 = EDGE_CURVE ( 'NONE', #21074, #10214, #6755, .T. ) ;
#13369 = ORIENTED_EDGE ( 'NONE', *, *, #28860, .F. ) ;
#13370 = DIRECTION ( 'NONE',  ( 1.000000000000000000, -5.339440136655842133E-16, -1.047965281155519420E-16 ) ) ;
#13371 = DIRECTION ( 'NONE',  ( -1.000000000000000000, 0.000000000000000000, 0.000000000000000000 ) ) ;
#13372 = CARTESIAN_POINT ( 'NONE',  ( 4.000000000000003553, -24.47917365149914914, -45.87777302070961127 ) ) ;
#13373 = ORIENTED_EDGE ( 'NONE', *, *, #15157, .F. ) ;
#13374 = PRESENTATION_LAYER_ASSIGNMENT (  '', '', ( #34058 ) ) ;
#13375 = ADVANCED_BREP_SHAPE_REPRESENTATION ( '', ( #34226, #21307 ), #26556 ) ;
#13376 = DIRECTION ( 'NONE',  ( 1.000000000000000000, 0.000000000000000000, 0.000000000000000000 ) ) ;
#13377 = CARTESIAN_POINT ( 'NONE',  ( -35.50000000000000000, -113.0140978167138712, -0.3122823525984338988 ) ) ;
#13378 = DIRECTION ( 'NONE',  ( 0.000000000000000000, 0.4817536741017163782, -0.8763066800438630288 ) ) ;
#13379 = ADVANCED_FACE ( 'NONE', ( #3370 ), #22776, .T. ) ;
#13380 = CARTESIAN_POINT ( 'NONE',  ( -35.50000000000000711, -114.9929510916434339, 10.52826033068511435 ) ) ;
#13381 = DIRECTION ( 'NONE',  ( -1.000000000000000000, 0.000000000000000000, 0.000000000000000000 ) ) ;
#13382 = ORIENTED_EDGE ( 'NONE', *, *, #18756, .T. ) ;
#13383 = LINE ( 'NONE', #4935, #23963 ) ;
#13384 = CARTESIAN_POINT ( 'NONE',  ( -35.50000000000000000, -111.1014359431343905, 1.472195201997948510 ) ) ;
#13385 = AXIS2_PLACEMENT_3D ( 'NONE', #21443, #8118, #32440 ) ;
#13386 = ORIENTED_EDGE ( 'NONE', *, *, #27591, .T. ) ;
#13387 = VERTEX_POINT ( 'NONE', #470 ) ;
#13388 = CARTESIAN_POINT ( 'NONE',  ( -36.11231047232249125, -112.0245472910329880, 2.722274454178448266 ) ) ;
#13389 =( NAMED_UNIT ( * ) PLANE_ANGLE_UNIT ( ) SI_UNIT ( $, .RADIAN. ) );
#13390 = CYLINDRICAL_SURFACE ( 'NONE', #34230, 52.00000000000000711 ) ;
#13391 = ORIENTED_EDGE ( 'NONE', *, *, #17830, .T. ) ;
#13392 = ORIENTED_EDGE ( 'NONE', *, *, #34832, .F. ) ;
#13393 = CARTESIAN_POINT ( 'NONE',  ( -34.50000000000000000, -113.0140978167138712, 0.7189676474015717078 ) ) ;
#13394 = CARTESIAN_POINT ( 'NONE',  ( 7.999999999999992895, 0.000000000000000000, 0.000000000000000000 ) ) ;
#13395 = FACE_OUTER_BOUND ( 'NONE', #28516, .T. ) ;
#13396 = DIRECTION ( 'NONE',  ( -1.000000000000000000, 0.000000000000000000, 0.000000000000000000 ) ) ;
#13397 = CIRCLE ( 'NONE', #734, 47.49900000000001654 ) ;
#13398 = CARTESIAN_POINT ( 'NONE',  ( -37.46093750000000711, -114.9929510916434339, 13.11852480586264669 ) ) ;
#13399 = VECTOR ( 'NONE', #33911, 1000.000000000000000 ) ;
#13400 = CARTESIAN_POINT ( 'NONE',  ( 0.000000000000000000, -3.840921266750157326, 47.34345070675169609 ) ) ;
#13401 = DIRECTION ( 'NONE',  ( -1.000000000000000000, 0.000000000000000000, 0.000000000000000000 ) ) ;
#13402 = CARTESIAN_POINT ( 'NONE',  ( -34.50000000000000000, -115.1770117227680998, -1.611965039240062181 ) ) ;
#13403 = CARTESIAN_POINT ( 'NONE',  ( 0.000000000000000000, 10.46102064772367868, -19.35373470438974053 ) ) ;
#13404 = VECTOR ( 'NONE', #1146, 1000.000000000000000 ) ;
#13405 = ADVANCED_FACE ( 'NONE', ( #30717 ), #6051, .F. ) ;
#13406 = AXIS2_PLACEMENT_3D ( 'NONE', #1629, #22859, #20856 ) ;
#13407 = EDGE_CURVE ( 'NONE', #21242, #14544, #11796, .T. ) ;
#13408 = FACE_BOUND ( 'NONE', #10430, .T. ) ;
#13409 = ORIENTED_EDGE ( 'NONE', *, *, #10734, .T. ) ;
#13410 = CARTESIAN_POINT ( 'NONE',  ( -38.00000000000000711, -115.9929510916434481, 10.85830208992306822 ) ) ;
#13411 = CARTESIAN_POINT ( 'NONE',  ( -34.49999999999998579, -31.64142946139395107, 72.19543654875866423 ) ) ;
#13412 = CARTESIAN_POINT ( 'NONE',  ( -29.99999999999999645, 11.00000000000000000, 0.000000000000000000 ) ) ;
#13413 = CARTESIAN_POINT ( 'NONE',  ( 4.000000000000003553, 9.637487275701349887, -10.15474465512039615 ) ) ;
#13414 = CONTEXT_DEPENDENT_SHAPE_REPRESENTATION ( #20934, #27690 ) ;
#13415 = CARTESIAN_POINT ( 'NONE',  ( -42.49999999999999289, -38.78532556477446036, 90.66066734786068082 ) ) ;
#13416 = EDGE_LOOP ( 'NONE', ( #27002, #16952, #2298, #18204 ) ) ;
#13417 = CARTESIAN_POINT ( 'NONE',  ( 4.000000000000003553, -10.46102064772354723, 19.35373470438981869 ) ) ;
#13418 = DIRECTION ( 'NONE',  ( -1.000000000000000000, -0.000000000000000000, -0.000000000000000000 ) ) ;
#13419 = CARTESIAN_POINT ( 'NONE',  ( 3.999999999999996447, 2.912696353506125657, -21.80633394113447210 ) ) ;
#13420 = FACE_OUTER_BOUND ( 'NONE', #142, .T. ) ;
#13421 = EDGE_CURVE ( 'NONE', #29017, #23042, #1532, .T. ) ;
#13422 = DIRECTION ( 'NONE',  ( -1.000000000000000000, 0.000000000000000000, 0.000000000000000000 ) ) ;
#13423 = CARTESIAN_POINT ( 'NONE',  ( 0.000000000000000000, 16.94522934049224361, -8.128228055638670568 ) ) ;
#13424 = VERTEX_POINT ( 'NONE', #22419 ) ;
#13425 = AXIS2_PLACEMENT_3D ( 'NONE', #16522, #8067, #2872 ) ;
#13426 = VERTEX_POINT ( 'NONE', #9106 ) ;
#13427 = EDGE_CURVE ( 'NONE', #17487, #28349, #33777, .T. ) ;
#13428 = DIRECTION ( 'NONE',  ( 0.000000000000000000, -6.983129352544636959E-15, 1.000000000000000000 ) ) ;
#13429 = CYLINDRICAL_SURFACE ( 'NONE', #29771, 17.49900000000000233 ) ;
#13430 = LINE ( 'NONE', #32500, #12227 ) ;
#13431 = ORIENTED_EDGE ( 'NONE', *, *, #23483, .F. ) ;
#13432 = CARTESIAN_POINT ( 'NONE',  ( -38.99999999999999289, -114.0592624029313242, 6.246475545821550845 ) ) ;
#13433 = ORIENTED_EDGE ( 'NONE', *, *, #34467, .F. ) ;
#13434 = VERTEX_POINT ( 'NONE', #23136 ) ;
#13435 = ORIENTED_EDGE ( 'NONE', *, *, #21723, .F. ) ;
#13436 = CARTESIAN_POINT ( 'NONE',  ( -36.49999999999999289, -11.52052244843579309, 118.1848168619253556 ) ) ;
#13437 = CIRCLE ( 'NONE', #5373, 4.980000000000017302 ) ;
#13438 = AXIS2_PLACEMENT_3D ( 'NONE', #11660, #30414, #25190 ) ;
#13439 = EDGE_CURVE ( 'NONE', #11158, #28784, #11880, .T. ) ;
#13440 = DIRECTION ( 'NONE',  ( -1.000000000000000000, 0.000000000000000000, 0.000000000000000000 ) ) ;
#13441 = ORIENTED_EDGE ( 'NONE', *, *, #973, .T. ) ;
#13442 = EDGE_LOOP ( 'NONE', ( #16057, #14556, #30729, #13939 ) ) ;
#13443 = CYLINDRICAL_SURFACE ( 'NONE', #20214, 52.00000000000000711 ) ;
#13444 = DIRECTION ( 'NONE',  ( 8.645950338799857827E-17, -6.938893903907203726E-17, -1.000000000000000000 ) ) ;
#13445 = CARTESIAN_POINT ( 'NONE',  ( 8.000000000000000000, 0.000000000000000000, 0.000000000000000000 ) ) ;
#13446 = AXIS2_PLACEMENT_3D ( 'NONE', #29309, #12563, #34709 ) ;
#13447 = DIRECTION ( 'NONE',  ( -1.000000000000000000, 0.000000000000000000, 0.000000000000000000 ) ) ;
#13448 = DIRECTION ( 'NONE',  ( -1.000000000000000000, 0.000000000000000000, 0.000000000000000000 ) ) ;
#13449 = EDGE_CURVE ( 'NONE', #3021, #21428, #13037, .T. ) ;
#13450 = EDGE_CURVE ( 'NONE', #6425, #29329, #14169, .T. ) ;
#13451 = CARTESIAN_POINT ( 'NONE',  ( -35.62769128460905677, -115.4561184093552413, 6.191024454178448266 ) ) ;
#13452 = EDGE_CURVE ( 'NONE', #20326, #10473, #17605, .T. ) ;
#13453 = CARTESIAN_POINT ( 'NONE',  ( -37.74437085908086686, -115.9929510916434481, 14.09929883582536903 ) ) ;
#13454 = PLANE ( 'NONE',  #9047 ) ;
#13455 = CARTESIAN_POINT ( 'NONE',  ( 0.000000000000000000, 0.000000000000000000, 65.00000000000000000 ) ) ;
#13456 = CARTESIAN_POINT ( 'NONE',  ( 8.000000000000000000, -10.62435788049434038, -13.16139124467930444 ) ) ;
#13457 = CYLINDRICAL_SURFACE ( 'NONE', #30742, 47.49900000000001654 ) ;
#13458 = AXIS2_PLACEMENT_3D ( 'NONE', #4173, #3810, #25779 ) ;
#13459 = DIRECTION ( 'NONE',  ( -1.000000000000000000, -1.734723475976807094E-16, 0.000000000000000000 ) ) ;
#13460 = CYLINDRICAL_SURFACE ( 'NONE', #1714, 7.199999999999993960 ) ;
#13461 = ORIENTED_EDGE ( 'NONE', *, *, #34428, .T. ) ;
#13462 = EDGE_CURVE ( 'NONE', #29830, #26423, #8734, .T. ) ;
#13463 = CARTESIAN_POINT ( 'NONE',  ( -34.00000000000000000, -113.9407375970686758, 8.496475545821549957 ) ) ;
#13464 = CYLINDRICAL_SURFACE ( 'NONE', #27318, 7.199999999999993960 ) ;
#13465 = LINE ( 'NONE', #34590, #25091 ) ;
#13466 = DIRECTION ( 'NONE',  ( -1.000000000000000000, 0.000000000000000000, 0.000000000000000000 ) ) ;
#13467 = EDGE_CURVE ( 'NONE', #22983, #3168, #19357, .T. ) ;
#13468 = ORIENTED_EDGE ( 'NONE', *, *, #7341, .F. ) ;
#13469 = ORIENTED_EDGE ( 'NONE', *, *, #2260, .T. ) ;
#13470 = SURFACE_STYLE_USAGE ( .BOTH. , #2501 ) ;
#13471 = DIRECTION ( 'NONE',  ( -1.000000000000000000, 0.000000000000000000, 0.000000000000000000 ) ) ;
#13472 = ORIENTED_EDGE ( 'NONE', *, *, #11481, .T. ) ;
#13473 = EDGE_LOOP ( 'NONE', ( #12428, #1063, #33228, #16154 ) ) ;
#13474 = LINE ( 'NONE', #2864, #16557 ) ;
#13475 = LINE ( 'NONE', #5383, #32664 ) ;
#13476 = DIRECTION ( 'NONE',  ( 1.000000000000000000, 0.000000000000000000, 0.000000000000000000 ) ) ;
#13477 = EDGE_CURVE ( 'NONE', #31888, #35006, #1013, .T. ) ;
#13478 = FACE_OUTER_BOUND ( 'NONE', #32425, .T. ) ;
#13479 = ORIENTED_EDGE ( 'NONE', *, *, #13134, .F. ) ;
#13480 = ORIENTED_EDGE ( 'NONE', *, *, #546, .F. ) ;
#13481 = CARTESIAN_POINT ( 'NONE',  ( -35.50000000000000711, -112.0140978167138712, -0.4997823525984337878 ) ) ;
#13482 = AXIS2_PLACEMENT_3D ( 'NONE', #4312, #12582, #1604 ) ;
#13483 = AXIS2_PLACEMENT_3D ( 'NONE', #23227, #12254, #34220 ) ;
#13484 = EDGE_CURVE ( 'NONE', #33840, #7659, #3865, .T. ) ;
#13485 = DIRECTION ( 'NONE',  ( 0.000000000000000000, 0.000000000000000000, -1.000000000000000000 ) ) ;
#13486 = CARTESIAN_POINT ( 'NONE',  ( 7.999999999999992895, 0.000000000000000000, 0.000000000000000000 ) ) ;
#13487 = EDGE_CURVE ( 'NONE', #30439, #11413, #3539, .T. ) ;
#13488 = VERTEX_POINT ( 'NONE', #25497 ) ;
#13489 = CARTESIAN_POINT ( 'NONE',  ( -0.1085714285714300953, -3.798448662927791819, 0.000000000000000000 ) ) ;
#13490 = CARTESIAN_POINT ( 'NONE',  ( -34.50000000000000000, -112.8511839106603247, -1.611965039240275122 ) ) ;
#13491 = CARTESIAN_POINT ( 'NONE',  ( -38.92341863475394348, -114.9929510916434339, 13.10177712753322155 ) ) ;
#13492 = CARTESIAN_POINT ( 'NONE',  ( 0.000000000000000000, 0.000000000000000000, 0.000000000000000000 ) ) ;
#13493 = EDGE_CURVE ( 'NONE', #8147, #26137, #6569, .T. ) ;
#13494 = CARTESIAN_POINT ( 'NONE',  ( -35.50000000000000000, -113.9697269463297431, 10.50348536859153370 ) ) ;
#13495 = DIRECTION ( 'NONE',  ( -1.000000000000000000, 0.000000000000000000, 0.000000000000000000 ) ) ;
#13496 = ADVANCED_FACE ( 'NONE', ( #3899 ), #14855, .T. ) ;
#13497 = CARTESIAN_POINT ( 'NONE',  ( -34.50000000000000000, -114.9929510916434339, 12.50851088611648088 ) ) ;
#13498 = DIRECTION ( 'NONE',  ( 0.000000000000000000, -0.9510565162951565288, 0.3090169943749382919 ) ) ;
#13499 = CARTESIAN_POINT ( 'NONE',  ( 5.639656061357297467, -10.48075544252193048, -1.200000000000006617 ) ) ;
#13500 = DIRECTION ( 'NONE',  ( 1.000000000000000000, -0.000000000000000000, 0.000000000000000000 ) ) ;
#13501 = ORIENTED_EDGE ( 'NONE', *, *, #6564, .T. ) ;
#13502 = DIRECTION ( 'NONE',  ( 1.000000000000000000, -0.000000000000000000, 0.000000000000000000 ) ) ;
#13503 = CARTESIAN_POINT ( 'NONE',  ( 50.00005079999999680, 5.399999999999999467, -1.000000000000003109 ) ) ;
#13504 = EDGE_LOOP ( 'NONE', ( #27020, #23191 ) ) ;
#13505 = CARTESIAN_POINT ( 'NONE',  ( -36.62499999999902656, -114.9929510916434339, 13.11852480586264669 ) ) ;
#13506 = ORIENTED_EDGE ( 'NONE', *, *, #27117, .F. ) ;
#13507 = CARTESIAN_POINT ( 'NONE',  ( -39.02454729103295961, -114.7691647218148745, 6.659774454178450043 ) ) ;
#13508 = FACE_BOUND ( 'NONE', #20448, .T. ) ;
#13509 = EDGE_CURVE ( 'NONE', #7270, #29218, #15887, .T. ) ;
#13510 = ORIENTED_EDGE ( 'NONE', *, *, #11859, .F. ) ;
#13511 = VERTEX_POINT ( 'NONE', #34313 ) ;
#13512 = CIRCLE ( 'NONE', #22678, 4.000000000000000000 ) ;
#13513 = CARTESIAN_POINT ( 'NONE',  ( 5.400000000000015454, -1.000000000000002220, -30.00000000000000000 ) ) ;
#13514 = VECTOR ( 'NONE', #31641, 1000.000000000000000 ) ;
#13515 = DIRECTION ( 'NONE',  ( -1.000000000000000000, -1.836970198721029934E-16, -0.000000000000000000 ) ) ;
#13516 = ORIENTED_EDGE ( 'NONE', *, *, #4009, .F. ) ;
#13517 = CARTESIAN_POINT ( 'NONE',  ( -39.99999999999999289, -114.0592624029313242, 3.246475545821551734 ) ) ;
#13518 = VECTOR ( 'NONE', #7162, 1000.000000000000000 ) ;
#13519 = CARTESIAN_POINT ( 'NONE',  ( 3.799999999999999822, 4.653657836759942730E-16, -39.50000000000000711 ) ) ;
#13520 = CARTESIAN_POINT ( 'NONE',  ( 0.000000000000000000, 10.00000000000000888, -25.00000000000000000 ) ) ;
#13521 = ORIENTED_EDGE ( 'NONE', *, *, #18595, .F. ) ;
#13522 = EDGE_LOOP ( 'NONE', ( #18379, #27421, #12641, #28216 ) ) ;
#13523 = CARTESIAN_POINT ( 'NONE',  ( 70.00001200000001234, -23.96628619204960486, 81.50485444658289680 ) ) ;
#13524 = ADVANCED_FACE ( 'NONE', ( #12522 ), #24054, .T. ) ;
#13525 = DIRECTION ( 'NONE',  ( -1.000000000000000000, 0.000000000000000000, 0.000000000000000000 ) ) ;
#13527 = VERTEX_POINT ( 'NONE', #32138 ) ;
#13526 = CIRCLE ( 'NONE', #34209, 3.799999999999999822 ) ;
#13528 = EDGE_LOOP ( 'NONE', ( #26678, #1161, #5920, #21177, #35548, #28268 ) ) ;
#13529 = CARTESIAN_POINT ( 'NONE',  ( -34.50000000000000000, -114.1807644833817648, -2.624782352598442614 ) ) ;
#13530 = ADVANCED_FACE ( 'NONE', ( #28906, #15027 ), #18082, .F. ) ;
#13531 = DIRECTION ( 'NONE',  ( 0.000000000000000000, 0.000000000000000000, 1.000000000000000000 ) ) ;
#13532 = ORIENTED_EDGE ( 'NONE', *, *, #12831, .T. ) ;
#13533 = CARTESIAN_POINT ( 'NONE',  ( -35.50000000000000711, -114.1264797827112574, 9.515205387299289441 ) ) ;
#13534 = CARTESIAN_POINT ( 'NONE',  ( -35.80421860361284558, -113.9929510916434339, 14.10650203519841916 ) ) ;
#13535 = DIRECTION ( 'NONE',  ( -1.000000000000000000, 0.000000000000000000, 0.000000000000000000 ) ) ;
#13536 = EDGE_CURVE ( 'NONE', #26957, #9355, #6131, .T. ) ;
#13537 = CYLINDRICAL_SURFACE ( 'NONE', #32343, 47.49900000000001654 ) ;
#13538 = CARTESIAN_POINT ( 'NONE',  ( -37.37500000000009237, -113.9929510916434339, 13.11852480586264846 ) ) ;
#13539 = CARTESIAN_POINT ( 'NONE',  ( -35.50000000000000711, -114.9929510916434339, 10.59426868253284226 ) ) ;
#13540 = DIRECTION ( 'NONE',  ( 0.000000000000000000, 0.000000000000000000, -1.000000000000000000 ) ) ;
#13541 = AXIS2_PLACEMENT_3D ( 'NONE', #27439, #5296, #11043 ) ;
#13542 = FACE_OUTER_BOUND ( 'NONE', #23420, .T. ) ;
#13543 = EDGE_LOOP ( 'NONE', ( #3324, #12529, #24691, #7639 ) ) ;
#13544 = CARTESIAN_POINT ( 'NONE',  ( 23.00000000000000711, 1.230770033143090132E-14, 0.000000000000000000 ) ) ;
#13545 = DIRECTION ( 'NONE',  ( 0.000000000000000000, 0.000000000000000000, 1.000000000000000000 ) ) ;
#13546 = DIRECTION ( 'NONE',  ( 1.000000000000000000, -0.000000000000000000, -0.000000000000000000 ) ) ;
#13547 = ORIENTED_EDGE ( 'NONE', *, *, #12850, .F. ) ;
#13548 = CARTESIAN_POINT ( 'NONE',  ( 7.999999999999992895, -39.64889472655708857, -33.64468972902551513 ) ) ;
#13549 = ORIENTED_EDGE ( 'NONE', *, *, #30883, .F. ) ;
#13550 = CARTESIAN_POINT ( 'NONE',  ( -35.50000000000000000, -113.1291422947505936, 0.8889500704178361357 ) ) ;
#13551 = DIRECTION ( 'NONE',  ( 0.000000000000000000, 0.000000000000000000, -1.000000000000000000 ) ) ;
#13552 = CARTESIAN_POINT ( 'NONE',  ( -35.50000000000000711, -114.9929510916434339, 10.53376102667243508 ) ) ;
#13553 = DIRECTION ( 'NONE',  ( -1.000000000000000000, 0.000000000000000000, 0.000000000000000000 ) ) ;
#13554 = ORIENTED_EDGE ( 'NONE', *, *, #26376, .T. ) ;
#13555 = DIRECTION ( 'NONE',  ( -1.000000000000000000, -1.836970198721029934E-16, 0.000000000000000000 ) ) ;
#13556 = AXIS2_PLACEMENT_3D ( 'NONE', #8703, #19507, #14104 ) ;
#13557 = CARTESIAN_POINT ( 'NONE',  ( -35.50000000000000000, -111.0140978167138570, -0.3747823525984258497 ) ) ;
#13558 = ORIENTED_EDGE ( 'NONE', *, *, #9162, .F. ) ;
#13559 = VERTEX_POINT ( 'NONE', #26031 ) ;
#13560 = CARTESIAN_POINT ( 'NONE',  ( -36.33479806579561000, -114.7490116281687165, 6.191024454178448266 ) ) ;
#13561 = AXIS2_PLACEMENT_3D ( 'NONE', #6352, #19659, #30672 ) ;
#13562 = CIRCLE ( 'NONE', #2656, 3.799999999999999822 ) ;
#13563 = SURFACE_SIDE_STYLE ('',( #21295 ) ) ;
#13564 = DIRECTION ( 'NONE',  ( 0.000000000000000000, 0.000000000000000000, 1.000000000000000000 ) ) ;
#13565 = ORIENTED_EDGE ( 'NONE', *, *, #5046, .T. ) ;
#13566 = ORIENTED_EDGE ( 'NONE', *, *, #22127, .F. ) ;
#13567 = CARTESIAN_POINT ( 'NONE',  ( -34.50000000000000000, -114.9932644833805426, -0.6247823525982824089 ) ) ;
#13568 = CARTESIAN_POINT ( 'NONE',  ( 7.999999999999992895, -32.00046193115124282, -34.40241257139719977 ) ) ;
#13569 = EDGE_CURVE ( 'NONE', #33265, #13312, #15193, .T. ) ;
#13570 = DIRECTION ( 'NONE',  ( -1.000000000000000000, 0.000000000000000000, 0.000000000000000000 ) ) ;
#13571 = CARTESIAN_POINT ( 'NONE',  ( 0.000000000000000000, 16.59870953437680896, 3.253005020243904255 ) ) ;
#13572 = CARTESIAN_POINT ( 'NONE',  ( -35.50000000000000000, -113.9929510916434339, 12.53051367006571581 ) ) ;
#13573 = CARTESIAN_POINT ( 'NONE',  ( 8.000000000000000000, 0.000000000000000000, 0.000000000000000000 ) ) ;
#13574 = CARTESIAN_POINT ( 'NONE',  ( 0.000000000000000000, 0.000000000000000000, -34.40000000000000568 ) ) ;
#13575 = CARTESIAN_POINT ( 'NONE',  ( -34.50000000000000000, -112.1859307030124739, 1.448610958621386224 ) ) ;
#13576 = CARTESIAN_POINT ( 'NONE',  ( -37.24999999999992184, -115.9929510916434481, 14.11852480586265024 ) ) ;
#13577 = CARTESIAN_POINT ( 'NONE',  ( 8.000000000000000000, -2.494040418455211849, -18.62763138773853200 ) ) ;
#13578 = CIRCLE ( 'NONE', #11843, 47.49900000000001654 ) ;
#13579 = CARTESIAN_POINT ( 'NONE',  ( 7.999999999999992895, -15.49408907645140943, -44.90087086784610904 ) ) ;
#13580 = ORIENTED_EDGE ( 'NONE', *, *, #30877, .F. ) ;
#13581 = CARTESIAN_POINT ( 'NONE',  ( -38.00000000000000711, -115.9929510916434481, 12.39849696637031151 ) ) ;
#13582 = FACE_OUTER_BOUND ( 'NONE', #2123, .T. ) ;
#13583 = SURFACE_SIDE_STYLE ('',( #35568 ) ) ;
#13584 = CYLINDRICAL_SURFACE ( 'NONE', #3058, 0.5000000000000004441 ) ;
#13585 = AXIS2_PLACEMENT_3D ( 'NONE', #16583, #27593, #24876 ) ;
#13586 = CARTESIAN_POINT ( 'NONE',  ( 8.000000000000000000, 3.678165988948591814, 15.05623113391068379 ) ) ;
#13587 = ORIENTED_EDGE ( 'NONE', *, *, #2777, .T. ) ;
#13588 = AXIS2_PLACEMENT_3D ( 'NONE', #17920, #4264, #1198 ) ;
#13589 = CARTESIAN_POINT ( 'NONE',  ( 0.000000000000000000, -9.604183132802312173, -1.108880290975637228 ) ) ;
#13590 = CARTESIAN_POINT ( 'NONE',  ( 0.000000000000000000, 3.753907720749127819, 8.725776631572756514 ) ) ;
#13591 = CARTESIAN_POINT ( 'NONE',  ( 7.999999999999992895, -19.44205635905572649, 43.33776004284603545 ) ) ;
#13592 = DIRECTION ( 'NONE',  ( 0.000000000000000000, -6.938893903907226800E-15, 1.000000000000000000 ) ) ;
#13593 = PRESENTATION_LAYER_ASSIGNMENT (  '', '', ( #6670 ) ) ;
#13594 = CARTESIAN_POINT ( 'NONE',  ( -55.00000000000000000, 0.000000000000000000, -5.000000000000011546 ) ) ;
#13595 = DIRECTION ( 'NONE',  ( -1.000000000000000000, 0.000000000000000000, 0.000000000000000000 ) ) ;
#13596 = ORIENTED_EDGE ( 'NONE', *, *, #6207, .F. ) ;
#13597 = ORIENTED_EDGE ( 'NONE', *, *, #15368, .F. ) ;
#13598 = CARTESIAN_POINT ( 'NONE',  ( 7.999999999999992895, 0.000000000000000000, 0.000000000000000000 ) ) ;
#13599 = DIRECTION ( 'NONE',  ( -1.000000000000000000, -0.000000000000000000, -0.000000000000000000 ) ) ;
#13600 = LINE ( 'NONE', #13784, #12849 ) ;
#13601 = ORIENTED_EDGE ( 'NONE', *, *, #20357, .F. ) ;
#13602 = CARTESIAN_POINT ( 'NONE',  ( -34.97545270896703329, -114.7691647218148745, 8.590225545821551734 ) ) ;
#13603 = ORIENTED_EDGE ( 'NONE', *, *, #16808, .T. ) ;
#13604 = EDGE_LOOP ( 'NONE', ( #29671, #26588, #29152, #13501 ) ) ;
#13605 = EDGE_LOOP ( 'NONE', ( #29645, #20097, #34772, #20753, #18818, #19520 ) ) ;
#13606 = CARTESIAN_POINT ( 'NONE',  ( 0.000000000000000000, 16.53603053422211389, 8.931325931664652273 ) ) ;
#13607 = EDGE_CURVE ( 'NONE', #8021, #7666, #9812, .T. ) ;
#13608 = AXIS2_PLACEMENT_3D ( 'NONE', #11715, #31345, #11549 ) ;
#13609 = EDGE_CURVE ( 'NONE', #793, #27859, #7292, .T. ) ;
#13610 = VECTOR ( 'NONE', #18853, 1000.000000000000000 ) ;
#13611 = CARTESIAN_POINT ( 'NONE',  ( 0.000000000000000000, 0.000000000000000000, 0.000000000000000000 ) ) ;
#13612 = ORIENTED_EDGE ( 'NONE', *, *, #24656, .F. ) ;
#13613 = AXIS2_PLACEMENT_3D ( 'NONE', #13423, #24404, #35391 ) ;
#13614 = DIRECTION ( 'NONE',  ( -1.000000000000000000, 0.000000000000000000, 0.000000000000000000 ) ) ;
#13615 = DIRECTION ( 'NONE',  ( -1.000000000000000000, 0.000000000000000000, 0.000000000000000000 ) ) ;
#13616 = VECTOR ( 'NONE', #20414, 1000.000000000000000 ) ;
#13617 = ADVANCED_FACE ( 'NONE', ( #12335, #6936 ), #29086, .F. ) ;
#13618 = FACE_OUTER_BOUND ( 'NONE', #10277, .T. ) ;
#13619 = AXIS2_PLACEMENT_3D ( 'NONE', #7969, #13213, #23832 ) ;
#13620 = AXIS2_PLACEMENT_3D ( 'NONE', #23865, #9643, #23681 ) ;
#13621 = DIRECTION ( 'NONE',  ( 0.000000000000000000, -0.5877852522924799095, 0.8090169943749424553 ) ) ;
#13622 = CARTESIAN_POINT ( 'NONE',  ( -21.15833593587365513, -24.48076211353301801, 67.99999999999991473 ) ) ;
#13623 = DIRECTION ( 'NONE',  ( -1.000000000000000000, 0.000000000000000000, 0.000000000000000000 ) ) ;
#13624 = CARTESIAN_POINT ( 'NONE',  ( -38.99518666717493431, -115.9929510916434481, 12.74107470552714894 ) ) ;
#13625 = LINE ( 'NONE', #16486, #24589 ) ;
#13626 = CARTESIAN_POINT ( 'NONE',  ( -44.00000000000000000, 0.000000000000000000, 0.000000000000000000 ) ) ;
#13627 = AXIS2_PLACEMENT_3D ( 'NONE', #15422, #12746, #20999 ) ;
#13628 = DIRECTION ( 'NONE',  ( 0.000000000000000000, 0.8660254037844428154, -0.4999999999999929501 ) ) ;
#13629 = PLANE ( 'NONE',  #22129 ) ;
#13630 = VECTOR ( 'NONE', #24042, 1000.000000000000000 ) ;
#13631 = CARTESIAN_POINT ( 'NONE',  ( -3.799999999999999822, -2.710505431213761085E-17, -46.00000000000000000 ) ) ;
#13632 = FACE_OUTER_BOUND ( 'NONE', #34319, .T. ) ;
#13633 = ORIENTED_EDGE ( 'NONE', *, *, #29094, .T. ) ;
#13634 = CARTESIAN_POINT ( 'NONE',  ( -36.94073759706868287, -115.0000000000000000, 4.371475545821550845 ) ) ;
#13635 = CIRCLE ( 'NONE', #16497, 4.800000000000000711 ) ;
#13636 = DIRECTION ( 'NONE',  ( -1.000000000000000000, -0.000000000000000000, 0.000000000000000000 ) ) ;
#13637 = DIRECTION ( 'NONE',  ( -1.734723475976807094E-16, 1.000000000000000000, 0.000000000000000000 ) ) ;
#13638 = ADVANCED_FACE ( 'NONE', ( #20602 ), #1540, .T. ) ;
#13639 = CIRCLE ( 'NONE', #33173, 20.00000000000000000 ) ;
#13640 = DIRECTION ( 'NONE',  ( -0.000000000000000000, 0.000000000000000000, -1.000000000000000000 ) ) ;
#13641 = ORIENTED_EDGE ( 'NONE', *, *, #11605, .T. ) ;
#13642 = ORIENTED_EDGE ( 'NONE', *, *, #20482, .T. ) ;
#13643 = AXIS2_PLACEMENT_3D ( 'NONE', #21637, #16226, #18415 ) ;
#13644 = UNCERTAINTY_MEASURE_WITH_UNIT (LENGTH_MEASURE( 1.000000000000000082E-05 ), #23439, 'distance_accuracy_value', 'NONE');
#13645 = LINE ( 'NONE', #13819, #3947 ) ;
#13646 = LINE ( 'NONE', #5205, #27290 ) ;
#13647 = VERTEX_POINT ( 'NONE', #4433 ) ;
#13648 = CIRCLE ( 'NONE', #18800, 0.04100000000000673939 ) ;
#13649 = VECTOR ( 'NONE', #17923, 1000.000000000000000 ) ;
#13650 = ORIENTED_EDGE ( 'NONE', *, *, #5305, .F. ) ;
#13651 = CIRCLE ( 'NONE', #19359, 0.7500000000000006661 ) ;
#13652 = EDGE_CURVE ( 'NONE', #10099, #31717, #30882, .T. ) ;
#13653 = DIRECTION ( 'NONE',  ( -1.000000000000000000, -0.000000000000000000, 0.000000000000000000 ) ) ;
#13654 = ADVANCED_FACE ( 'NONE', ( #34672 ), #1361, .T. ) ;
#13655 = DIRECTION ( 'NONE',  ( 1.000000000000000000, -0.000000000000000000, -0.000000000000000000 ) ) ;
#13656 = EDGE_CURVE ( 'NONE', #10641, #6851, #23863, .T. ) ;
#13657 = APPLICATION_PROTOCOL_DEFINITION ( 'draft international standard', 'automotive_design', 1998, #3200 ) ;
#13658 = CARTESIAN_POINT ( 'NONE',  ( 8.000000000000000000, 0.000000000000000000, 0.000000000000000000 ) ) ;
#13659 = CIRCLE ( 'NONE', #32621, 0.5000000000000004441 ) ;
#13660 = ORIENTED_EDGE ( 'NONE', *, *, #34825, .T. ) ;
#13661 = VERTEX_POINT ( 'NONE', #4618 ) ;
#13662 = AXIS2_PLACEMENT_3D ( 'NONE', #10396, #12559, #23714 ) ;
#13663 = FACE_OUTER_BOUND ( 'NONE', #27743, .T. ) ;
#13664 = EDGE_CURVE ( 'NONE', #7329, #23201, #6160, .T. ) ;
#13665 = CARTESIAN_POINT ( 'NONE',  ( 0.000000000000000000, -36.05989434073592292, -30.12041790338657066 ) ) ;
#13666 = ORIENTED_EDGE ( 'NONE', *, *, #29434, .T. ) ;
#13667 = DIRECTION ( 'NONE',  ( 0.000000000000000000, 0.000000000000000000, -1.000000000000000000 ) ) ;
#13668 = AXIS2_PLACEMENT_3D ( 'NONE', #10291, #13348, #15837 ) ;
#13669 = ADVANCED_FACE ( 'NONE', ( #21145 ), #18448, .T. ) ;
#13670 = CARTESIAN_POINT ( 'NONE',  ( -34.50000000000000000, -116.0060826362711595, -0.7553032835231661135 ) ) ;
#13671 = CARTESIAN_POINT ( 'NONE',  ( -38.99699093265173389, -114.9929510916434339, 12.71660600561481402 ) ) ;
#13672 = CARTESIAN_POINT ( 'NONE',  ( -35.50000000000000000, -113.9929510916436470, 10.50625754673586876 ) ) ;
#13673 = CARTESIAN_POINT ( 'NONE',  ( 65.00000000000001421, -25.98076211353320986, 84.99999999999994316 ) ) ;
#13674 = CARTESIAN_POINT ( 'NONE',  ( -34.50075263804418313, -114.9929510916434339, 12.66759465831979981 ) ) ;
#13675 = DIRECTION ( 'NONE',  ( -1.000000000000000000, 0.000000000000000000, 0.000000000000000000 ) ) ;
#13676 = CIRCLE ( 'NONE', #19394, 3.799999999999999822 ) ;
#13677 = DIRECTION ( 'NONE',  ( 0.000000000000000000, 0.000000000000000000, 1.000000000000000000 ) ) ;
#13678 = PRESENTATION_STYLE_ASSIGNMENT (( #2713 ) ) ;
#13679 = DIRECTION ( 'NONE',  ( -1.000000000000000000, 0.000000000000000000, 0.000000000000000000 ) ) ;
#13680 = DIRECTION ( 'NONE',  ( -1.000000000000000000, 0.000000000000000000, 0.000000000000000000 ) ) ;
#13681 = CYLINDRICAL_SURFACE ( 'NONE', #11167, 52.00000000000000711 ) ;
#13682 = VERTEX_POINT ( 'NONE', #18985 ) ;
#13683 = CYLINDRICAL_SURFACE ( 'NONE', #12425, 20.00000000000000711 ) ;
#13684 = EDGE_LOOP ( 'NONE', ( #29759, #7269, #22534, #34604 ) ) ;
#13685 = CARTESIAN_POINT ( 'NONE',  ( -38.18337828418795965, -110.9754527089670546, 7.034774454178450043 ) ) ;
#13686 = CARTESIAN_POINT ( 'NONE',  ( -3.239593890920919428, -13.56862304811759579, 0.000000000000000000 ) ) ;
#13687 = EDGE_CURVE ( 'NONE', #10783, #10620, #10205, .T. ) ;
#13688 = CIRCLE ( 'NONE', #9642, 3.999999999999993339 ) ;
#13689 = ORIENTED_EDGE ( 'NONE', *, *, #34428, .F. ) ;
#13690 = ORIENTED_EDGE ( 'NONE', *, *, #33770, .T. ) ;
#13691 = FACE_OUTER_BOUND ( 'NONE', #20883, .T. ) ;
#13692 = DIRECTION ( 'NONE',  ( 0.000000000000000000, 0.000000000000000000, -1.000000000000000000 ) ) ;
#13693 = ORIENTED_EDGE ( 'NONE', *, *, #4611, .F. ) ;
#13694 = CARTESIAN_POINT ( 'NONE',  ( -35.81662171581203324, -110.9754527089670546, 3.715225545821552178 ) ) ;
#13695 = CIRCLE ( 'NONE', #30374, 11.00000000000000000 ) ;
#13696 = CIRCLE ( 'NONE', #22283, 4.000000000000000000 ) ;
#13697 = CIRCLE ( 'NONE', #22286, 20.00000000000000355 ) ;
#13698 = CYLINDRICAL_SURFACE ( 'NONE', #8059, 8.000000000000001776 ) ;
#13699 = DIRECTION ( 'NONE',  ( 0.000000000000000000, 0.000000000000000000, 1.000000000000000000 ) ) ;
#13700 = VERTEX_POINT ( 'NONE', #8173 ) ;
#13701 = ORIENTED_EDGE ( 'NONE', *, *, #11285, .T. ) ;
#13702 = ADVANCED_FACE ( 'NONE', ( #30152 ), #19155, .T. ) ;
#13703 = DIRECTION ( 'NONE',  ( 1.032573497605238773E-16, -6.938893903907203726E-17, -1.000000000000000000 ) ) ;
#13704 = EDGE_CURVE ( 'NONE', #11984, #21331, #29809, .T. ) ;
#13705 = VECTOR ( 'NONE', #14906, 1000.000000000000000 ) ;
#13706 =( LENGTH_UNIT ( ) NAMED_UNIT ( * ) SI_UNIT ( .MILLI., .METRE. ) );
#13707 = FACE_OUTER_BOUND ( 'NONE', #15752, .T. ) ;
#13708 = ORIENTED_EDGE ( 'NONE', *, *, #4605, .F. ) ;
#13709 = ORIENTED_EDGE ( 'NONE', *, *, #28615, .T. ) ;
#13710 = CARTESIAN_POINT ( 'NONE',  ( -34.50000000000000000, -115.5324766040685631, -2.560864217809699195 ) ) ;
#13711 = CARTESIAN_POINT ( 'NONE',  ( 0.000000000000000000, 0.000000000000000000, 45.00000000000000711 ) ) ;
#13712 = ORIENTED_EDGE ( 'NONE', *, *, #33283, .T. ) ;
#13713 = CARTESIAN_POINT ( 'NONE',  ( -35.50000000000000711, -114.9929510916434339, 11.21034663311131929 ) ) ;
#13714 = EDGE_CURVE ( 'NONE', #7443, #23156, #5147, .T. ) ;
#13715 = CARTESIAN_POINT ( 'NONE',  ( -34.51922597003733273, -113.9929510916434339, 12.86289566494349224 ) ) ;
#13716 = DIRECTION ( 'NONE',  ( -1.174092375852890260E-15, 4.222049128630259891E-16, 1.000000000000000000 ) ) ;
#13717 = CIRCLE ( 'NONE', #33835, 8.000000000000001776 ) ;
#13718 = DIRECTION ( 'NONE',  ( -1.000000000000000000, -0.000000000000000000, 0.000000000000000000 ) ) ;
#13719 = CARTESIAN_POINT ( 'NONE',  ( -34.50000000000000000, -113.9929510916434339, 12.39849696637031684 ) ) ;
#13720 = CARTESIAN_POINT ( 'NONE',  ( -39.00000000000000711, -114.9929510916434339, 12.50851088611646311 ) ) ;
#13721 = CIRCLE ( 'NONE', #27528, 3.799999999999999822 ) ;
#13722 = CARTESIAN_POINT ( 'NONE',  ( -38.00000000000000711, -115.9929510916434481, 10.50625754673587053 ) ) ;
#13723 = DIRECTION ( 'NONE',  ( 1.000000000000000000, -5.339440136655842133E-16, 1.047965281155515476E-16 ) ) ;
#13724 = AXIS2_PLACEMENT_3D ( 'NONE', #28139, #22361, #33357 ) ;
#13725 = DIRECTION ( 'NONE',  ( 0.000000000000000000, 1.000000000000000000, 3.469446951953614189E-15 ) ) ;
#13726 = VERTEX_POINT ( 'NONE', #82 ) ;
#13727 = EDGE_LOOP ( 'NONE', ( #11667, #23553, #1840, #22306 ) ) ;
#13728 = CARTESIAN_POINT ( 'NONE',  ( 70.00000000000001421, -27.28312344603513040, 77.61394185240837373 ) ) ;
#13729 = CARTESIAN_POINT ( 'NONE',  ( 1.110223024625156540E-13, -1.000000000000042633, -32.00000000000000000 ) ) ;
#13730 = ADVANCED_FACE ( 'NONE', ( #18808 ), #21490, .T. ) ;
#13731 = ORIENTED_EDGE ( 'NONE', *, *, #27965, .T. ) ;
#13732 = CARTESIAN_POINT ( 'NONE',  ( -42.49999999999999289, -16.18172400785637777, 71.02756813566458050 ) ) ;
#13733 = EDGE_LOOP ( 'NONE', ( #23730, #9619, #18774, #33351 ) ) ;
#13734 = EDGE_CURVE ( 'NONE', #14470, #10711, #2811, .T. ) ;
#13735 = CARTESIAN_POINT ( 'NONE',  ( -35.50000000000000000, -113.0140978167139991, 0.8595926474015699315 ) ) ;
#13736 = CARTESIAN_POINT ( 'NONE',  ( -55.00000000000000000, 0.000000000000000000, 64.00000000000000000 ) ) ;
#13737 = EDGE_CURVE ( 'NONE', #20033, #7746, #28602, .T. ) ;
#13738 = CARTESIAN_POINT ( 'NONE',  ( -37.35495115944176092, -112.9754527089670688, 2.534774454178448710 ) ) ;
#13739 = CARTESIAN_POINT ( 'NONE',  ( 8.000000000000007105, -5.908880290975582206, 9.604183132802395662 ) ) ;
#13740 = ORIENTED_EDGE ( 'NONE', *, *, #32968, .T. ) ;
#13741 = SURFACE_SIDE_STYLE ('',( #27431 ) ) ;
#13742 = CARTESIAN_POINT ( 'NONE',  ( -35.50000000000000000, -112.6572589393539516, 2.844055607295835397 ) ) ;
#13743 = ORIENTED_EDGE ( 'NONE', *, *, #11299, .F. ) ;
#13744 = ORIENTED_EDGE ( 'NONE', *, *, #24516, .F. ) ;
#13745 = EDGE_CURVE ( 'NONE', #21122, #6172, #11068, .T. ) ;
#13746 = CARTESIAN_POINT ( 'NONE',  ( -37.88768952767750164, -115.9754527089670262, 4.972274454178448266 ) ) ;
#13747 = VECTOR ( 'NONE', #24418, 1000.000000000000000 ) ;
#13748 = ADVANCED_FACE ( 'NONE', ( #27105 ), #22038, .T. ) ;
#13749 = DIRECTION ( 'NONE',  ( -1.000000000000000000, 0.000000000000000000, 0.000000000000000000 ) ) ;
#13750 = ORIENTED_EDGE ( 'NONE', *, *, #24635, .F. ) ;
#13751 = ORIENTED_EDGE ( 'NONE', *, *, #30713, .F. ) ;
#13752 = CARTESIAN_POINT ( 'NONE',  ( -34.50000000000000000, -115.0140978167138428, -0.6247823525979866455 ) ) ;
#13753 = LINE ( 'NONE', #20798, #17714 ) ;
#13754 = CARTESIAN_POINT ( 'NONE',  ( 8.000000000000000000, 0.000000000000000000, 0.000000000000000000 ) ) ;
#13755 = LINE ( 'NONE', #16425, #138 ) ;
#13756 = CARTESIAN_POINT ( 'NONE',  ( -35.50000000000000000, -113.9929510916434339, 10.50625754673588474 ) ) ;
#13757 = FACE_OUTER_BOUND ( 'NONE', #33279, .T. ) ;
#13758 = DIRECTION ( 'NONE',  ( 0.000000000000000000, 0.000000000000000000, -1.000000000000000000 ) ) ;
#13759 = CARTESIAN_POINT ( 'NONE',  ( -34.50000000000000000, -116.0140978167138712, -0.4997823525984418369 ) ) ;
#13760 = CARTESIAN_POINT ( 'NONE',  ( -38.99518666717493431, -115.9929510916434481, 12.74107470552714894 ) ) ;
#13761 = CARTESIAN_POINT ( 'NONE',  ( 1.799999999999996492, -4.728754675408722838E-14, 4.000000000000000000 ) ) ;
#13762 = FACE_OUTER_BOUND ( 'NONE', #20821, .T. ) ;
#13763 = DIRECTION ( 'NONE',  ( 1.000000000000000000, 0.000000000000000000, -1.691777834109591064E-31 ) ) ;
#13764 = ORIENTED_EDGE ( 'NONE', *, *, #22660, .T. ) ;
#13765 = AXIS2_PLACEMENT_3D ( 'NONE', #5351, #22067, #16292 ) ;
#13766 = CARTESIAN_POINT ( 'NONE',  ( -38.00000000000000711, -115.9929510916434481, 12.44250253426875119 ) ) ;
#13767 = DIRECTION ( 'NONE',  ( -1.000000000000000000, 8.673617379883896189E-17, 1.502314598737167413E-16 ) ) ;
#13768 = FACE_OUTER_BOUND ( 'NONE', #10524, .T. ) ;
#13769 = CARTESIAN_POINT ( 'NONE',  ( -55.00000000000000000, 0.000000000000000000, -5.000000000000011546 ) ) ;
#13770 = EDGE_CURVE ( 'NONE', #28824, #14767, #24396, .T. ) ;
#13771 = ORIENTED_EDGE ( 'NONE', *, *, #29600, .T. ) ;
#13772 = VECTOR ( 'NONE', #26148, 1000.000000000000114 ) ;
#13773 = CARTESIAN_POINT ( 'NONE',  ( -23.00000000000000000, 11.00000000000000000, 0.000000000000000000 ) ) ;
#13774 = DIRECTION ( 'NONE',  ( -1.000000000000000000, -0.000000000000000000, -0.000000000000000000 ) ) ;
#13775 = EDGE_CURVE ( 'NONE', #29301, #10171, #7638, .T. ) ;
#13776 = CARTESIAN_POINT ( 'NONE',  ( -4.000000000000000000, -2.710505431213761085E-17, 55.00000000000000000 ) ) ;
#13777 = CARTESIAN_POINT ( 'NONE',  ( 8.000000000000000000, -16.71027810728551799, 2.620268201065888203 ) ) ;
#13778 = AXIS2_PLACEMENT_3D ( 'NONE', #4667, #23729, #32187 ) ;
#13779 = CARTESIAN_POINT ( 'NONE',  ( 4.000000000000003553, 19.74581912682842244, 48.10512059033400334 ) ) ;
#13780 = LINE ( 'NONE', #22046, #364 ) ;
#13781 = ORIENTED_EDGE ( 'NONE', *, *, #11207, .T. ) ;
#13782 = CARTESIAN_POINT ( 'NONE',  ( 4.000000000000003553, 3.968388925835109049, -21.63912866391136447 ) ) ;
#13783 = CYLINDRICAL_SURFACE ( 'NONE', #34369, 3.799999999999999822 ) ;
#13784 = CARTESIAN_POINT ( 'NONE',  ( 4.000000000000000000, 4.627536653468036720E-16, 55.00000000000000000 ) ) ;
#13785 = EDGE_LOOP ( 'NONE', ( #16563, #20119, #9613, #12494 ) ) ;
#13786 = CARTESIAN_POINT ( 'NONE',  ( -38.97545270896704039, -114.8876895276775087, 7.652725545821552622 ) ) ;
#13787 = VERTEX_POINT ( 'NONE', #18626 ) ;
#13788 = ORIENTED_EDGE ( 'NONE', *, *, #25774, .T. ) ;
#13789 = ORIENTED_EDGE ( 'NONE', *, *, #450, .T. ) ;
#13790 = CARTESIAN_POINT ( 'NONE',  ( 8.000000000000000000, -2.494040418455483188, 18.62763138773849292 ) ) ;
#13791 = FACE_OUTER_BOUND ( 'NONE', #10332, .T. ) ;
#13792 = ORIENTED_EDGE ( 'NONE', *, *, #16484, .T. ) ;
#13793 = CIRCLE ( 'NONE', #18385, 17.49900000000001299 ) ;
#13794 = CARTESIAN_POINT ( 'NONE',  ( -35.50000000000000711, -114.1414532730574507, 9.517316564499758158 ) ) ;
#13795 = CYLINDRICAL_SURFACE ( 'NONE', #16049, 20.00000000000000355 ) ;
#13796 = AXIS2_PLACEMENT_3D ( 'NONE', #27679, #5878, #16494 ) ;
#13797 = CARTESIAN_POINT ( 'NONE',  ( 65.00000000000001421, -25.98076211353320986, 84.99999999999994316 ) ) ;
#13798 = DIRECTION ( 'NONE',  ( 1.000000000000000000, 0.000000000000000000, 0.000000000000000000 ) ) ;
#13799 = CIRCLE ( 'NONE', #18956, 14.00000000000000000 ) ;
#13800 = CARTESIAN_POINT ( 'NONE',  ( 7.999999999999992895, -7.162210897276087174, 51.50439529848826936 ) ) ;
#13801 = LINE ( 'NONE', #30185, #34086 ) ;
#13802 = CARTESIAN_POINT ( 'NONE',  ( 65.00000000000001421, 45.53424681125909501, 59.69714175238111409 ) ) ;
#13803 = CARTESIAN_POINT ( 'NONE',  ( -37.46093750000000711, -115.9929510916434481, 14.11852480586265024 ) ) ;
#13804 = DIRECTION ( 'NONE',  ( 0.000000000000000000, 0.9929510916431029122, -0.1185248058626136303 ) ) ;
#13805 = DIRECTION ( 'NONE',  ( 0.000000000000000000, 0.000000000000000000, 1.000000000000000000 ) ) ;
#13806 = DIRECTION ( 'NONE',  ( 1.000000000000000000, -0.000000000000000000, -0.000000000000000000 ) ) ;
#13807 = DIRECTION ( 'NONE',  ( 0.000000000000000000, 0.000000000000000000, 1.000000000000000000 ) ) ;
#13808 = EDGE_CURVE ( 'NONE', #16768, #11237, #13648, .T. ) ;
#13809 = CARTESIAN_POINT ( 'NONE',  ( -21.15833593587365513, -25.27980021920979326, 80.78589838486217900 ) ) ;
#13810 = FILL_AREA_STYLE ('',( #122 ) ) ;
#13811 = ORIENTED_EDGE ( 'NONE', *, *, #2482, .F. ) ;
#13812 = CARTESIAN_POINT ( 'NONE',  ( -37.66520193420439711, -114.7490116281687023, 4.558975545821549957 ) ) ;
#13813 = CARTESIAN_POINT ( 'NONE',  ( 22.99999999999999289, 1.230770033143089817E-14, 0.000000000000000000 ) ) ;
#13814 = DIRECTION ( 'NONE',  ( -1.000000000000000000, 0.000000000000000000, 0.000000000000000000 ) ) ;
#13815 = CARTESIAN_POINT ( 'NONE',  ( 1.110223024625156540E-13, -1.000000000000042633, 53.00000000000000711 ) ) ;
#13816 = ORIENTED_EDGE ( 'NONE', *, *, #34093, .T. ) ;
#13817 = AXIS2_PLACEMENT_3D ( 'NONE', #13846, #33113, #13677 ) ;
#13818 = VERTEX_POINT ( 'NONE', #13415 ) ;
#13819 = CARTESIAN_POINT ( 'NONE',  ( 0.000000000000000000, 0.000000000000000000, -1.000000000000000000 ) ) ;
#13820 = CYLINDRICAL_SURFACE ( 'NONE', #28432, 8.000000000000001776 ) ;
#13821 = ORIENTED_EDGE ( 'NONE', *, *, #28864, .T. ) ;
#13822 = EDGE_CURVE ( 'NONE', #7838, #27467, #5023, .T. ) ;
#13823 = EDGE_LOOP ( 'NONE', ( #28479, #4134, #8143, #22307 ) ) ;
#13824 = AXIS2_PLACEMENT_3D ( 'NONE', #33554, #31386, #11421 ) ;
#13825 = CIRCLE ( 'NONE', #16134, 20.00000000000000355 ) ;
#13826 = DIRECTION ( 'NONE',  ( -1.000000000000000000, 0.000000000000000000, 0.000000000000000000 ) ) ;
#13827 = DIRECTION ( 'NONE',  ( 0.000000000000000000, 0.000000000000000000, -1.000000000000000000 ) ) ;
#13828 = CARTESIAN_POINT ( 'NONE',  ( 37.99999999999999289, 8.902167771358703713E-16, 70.00000000000000000 ) ) ;
#13829 = DIRECTION ( 'NONE',  ( 1.000000000000000000, -0.000000000000000000, -0.000000000000000000 ) ) ;
#13830 = ORIENTED_EDGE ( 'NONE', *, *, #31329, .F. ) ;
#13831 = EDGE_LOOP ( 'NONE', ( #8107, #13991, #2957, #1107 ) ) ;
#13832 = CARTESIAN_POINT ( 'NONE',  ( -0.1717365941144438635, -6.008326913195953800, -0.7999999999999951594 ) ) ;
#13833 = CIRCLE ( 'NONE', #15536, 2.799122904894268071 ) ;
#13834 = DIRECTION ( 'NONE',  ( -1.836970198721029934E-16, 1.000000000000000000, 0.000000000000000000 ) ) ;
#13835 = ORIENTED_EDGE ( 'NONE', *, *, #30246, .T. ) ;
#13836 = CARTESIAN_POINT ( 'NONE',  ( -50.00000000000000000, 0.000000000000000000, 0.000000000000000000 ) ) ;
#13837 = CIRCLE ( 'NONE', #23026, 7.199999999999994849 ) ;
#13838 = CARTESIAN_POINT ( 'NONE',  ( -34.50000000000000000, -112.6919296022648638, -1.573728109100751116 ) ) ;
#13839 = CARTESIAN_POINT ( 'NONE',  ( -39.00000206272865455, -114.9929510916434339, 12.61164896875035701 ) ) ;
#13840 = CARTESIAN_POINT ( 'NONE',  ( -35.50000000000000000, -113.9929510916430075, 10.50625754673586876 ) ) ;
#13841 = CARTESIAN_POINT ( 'NONE',  ( -34.49999999999998579, -27.48076211353304998, 70.99999999999988631 ) ) ;
#13842 = VECTOR ( 'NONE', #35178, 1000.000000000000000 ) ;
#13843 = COLOUR_RGB ( '', 0.40784314, 0.44705882, 0.49803922) ;
#13844 = CARTESIAN_POINT ( 'NONE',  ( -34.50000000000000000, -114.9929510916434339, 12.60752341388803544 ) ) ;
#13845 = DIRECTION ( 'NONE',  ( 0.000000000000000000, 0.000000000000000000, 1.000000000000000000 ) ) ;
#13846 = CARTESIAN_POINT ( 'NONE',  ( 0.000000000000000000, 0.000000000000000000, 0.000000000000000000 ) ) ;
#13847 = AXIS2_PLACEMENT_3D ( 'NONE', #18686, #7884, #18153 ) ;
#13848 = ORIENTED_EDGE ( 'NONE', *, *, #20809, .F. ) ;
#13849 = CARTESIAN_POINT ( 'NONE',  ( 0.000000000000000000, -12.96676809804139197, -13.60411018104332292 ) ) ;
#13850 = CARTESIAN_POINT ( 'NONE',  ( 0.000000000000000000, -27.43636312076347394, 38.14186064215141414 ) ) ;
#13851 = ADVANCED_FACE ( 'NONE', ( #10895, #4963 ), #21861, .T. ) ;
#13852 = ORIENTED_EDGE ( 'NONE', *, *, #954, .F. ) ;
#13853 = ADVANCED_FACE ( 'NONE', ( #27157 ), #5199, .T. ) ;
#13854 = CARTESIAN_POINT ( 'NONE',  ( -38.00000000000000711, -114.9929510916434339, 10.50625754673587231 ) ) ;
#13855 = VERTEX_POINT ( 'NONE', #21730 ) ;
#13856 = CARTESIAN_POINT ( 'NONE',  ( -36.94073759706866156, -111.0000000000000284, 7.128524454178450043 ) ) ;
#13857 = FACE_OUTER_BOUND ( 'NONE', #20801, .T. ) ;
#13858 = EDGE_LOOP ( 'NONE', ( #31665, #6964, #33204, #13816 ) ) ;
#13859 = EDGE_LOOP ( 'NONE', ( #22435, #3643, #184, #33805 ) ) ;
#13860 = CARTESIAN_POINT ( 'NONE',  ( 8.000000000000000000, 0.3212489022567689423, -16.91141623315866482 ) ) ;
#13861 = CARTESIAN_POINT ( 'NONE',  ( -50.00000000000000000, 7.347880794884119736E-16, 76.00000000000001421 ) ) ;
#13862 = EDGE_CURVE ( 'NONE', #8656, #31607, #7321, .T. ) ;
#13863 = ORIENTED_EDGE ( 'NONE', *, *, #1002, .T. ) ;
#13864 = CARTESIAN_POINT ( 'NONE',  ( -36.94073759706868287, -116.9999999999999858, 4.371475545821550845 ) ) ;
#13865 = ADVANCED_FACE ( 'NONE', ( #34912 ), #16139, .F. ) ;
#13866 = CARTESIAN_POINT ( 'NONE',  ( 7.999999999999992895, 39.55064067543098361, -25.36340625197317067 ) ) ;
#13867 = FACE_OUTER_BOUND ( 'NONE', #22395, .T. ) ;
#13868 = EDGE_LOOP ( 'NONE', ( #19600, #7088, #14634, #33647 ) ) ;
#13869 = VERTEX_POINT ( 'NONE', #35614 ) ;
#13870 = DIRECTION ( 'NONE',  ( -1.000000000000000000, 0.000000000000000000, -0.000000000000000000 ) ) ;
#13871 = PRESENTATION_LAYER_ASSIGNMENT (  '', '', ( #23666 ) ) ;
#13872 = CYLINDRICAL_SURFACE ( 'NONE', #11555, 4.000000000000000000 ) ;
#13873 = ORIENTED_EDGE ( 'NONE', *, *, #20534, .T. ) ;
#13874 = ORIENTED_EDGE ( 'NONE', *, *, #30112, .T. ) ;
#13875 = CARTESIAN_POINT ( 'NONE',  ( -34.50000000000000000, -117.0141134414687514, -0.5779076015960331603 ) ) ;
#13876 = DIRECTION ( 'NONE',  ( 0.000000000000000000, -0.2486898871648622333, 0.9685831611286292997 ) ) ;
#13877 = ORIENTED_EDGE ( 'NONE', *, *, #10637, .T. ) ;
#13878 = CARTESIAN_POINT ( 'NONE',  ( -37.50818044754229419, -114.9929510916434339, 13.11847460610629668 ) ) ;
#13879 = EDGE_CURVE ( 'NONE', #25036, #26182, #34941, .T. ) ;
#13880 = CARTESIAN_POINT ( 'NONE',  ( -35.93867112612154102, -113.9929510916434339, 14.11732072679899197 ) ) ;
#13881 = CARTESIAN_POINT ( 'NONE',  ( -55.00000000000000000, 0.000000000000000000, 64.00000000000000000 ) ) ;
#13882 = DIRECTION ( 'NONE',  ( -1.000000000000000000, 0.000000000000000000, -0.000000000000000000 ) ) ;
#13883 = CARTESIAN_POINT ( 'NONE',  ( -34.50000000000000000, -113.9929510916434339, 10.50625754673588474 ) ) ;
#13884 = CARTESIAN_POINT ( 'NONE',  ( -37.88878409051687868, -114.9929510916434339, 14.07058620477052102 ) ) ;
#13885 = CARTESIAN_POINT ( 'NONE',  ( -35.50000000000000711, -114.4026847875275337, 9.592046023459676718 ) ) ;
#13886 = DIRECTION ( 'NONE',  ( 0.000000000000000000, 0.000000000000000000, -1.000000000000000000 ) ) ;
#13887 = DIRECTION ( 'NONE',  ( 0.000000000000000000, 0.000000000000000000, 1.000000000000000000 ) ) ;
#13888 = EDGE_CURVE ( 'NONE', #28224, #13661, #6719, .T. ) ;
#13889 = EDGE_LOOP ( 'NONE', ( #35272, #2113, #27929, #7229 ) ) ;
#13890 = EDGE_CURVE ( 'NONE', #21924, #10834, #23402, .T. ) ;
#13891 = ORIENTED_EDGE ( 'NONE', *, *, #18479, .F. ) ;
#13892 = EDGE_CURVE ( 'NONE', #28214, #13682, #18671, .T. ) ;
#13893 = CIRCLE ( 'NONE', #13343, 8.000000000000003553 ) ;
#13894 = DIRECTION ( 'NONE',  ( -1.000000000000000000, -0.000000000000000000, 0.000000000000000000 ) ) ;
#13895 = AXIS2_PLACEMENT_3D ( 'NONE', #27344, #33436, #28052 ) ;
#13896 = DIRECTION ( 'NONE',  ( -1.000000000000000000, 0.000000000000000000, 0.000000000000000000 ) ) ;
#13897 = EDGE_LOOP ( 'NONE', ( #3059, #19067, #26691, #11435 ) ) ;
#13898 = CARTESIAN_POINT ( 'NONE',  ( -90.00000000000002842, 0.000000000000000000, 6.938893903907228378E-15 ) ) ;
#13899 = ORIENTED_EDGE ( 'NONE', *, *, #20482, .F. ) ;
#13900 = CARTESIAN_POINT ( 'NONE',  ( -35.50000000000000000, -113.0140978167136581, 0.8752176474015604946 ) ) ;
#13901 = DIRECTION ( 'NONE',  ( 0.000000000000000000, 0.000000000000000000, -1.000000000000000000 ) ) ;
#13902 = CARTESIAN_POINT ( 'NONE',  ( -35.97545270896702618, -113.6450488405582604, 2.909774454178449155 ) ) ;
#13903 = EDGE_CURVE ( 'NONE', #29830, #20425, #8471, .T. ) ;
#13904 = LINE ( 'NONE', #24891, #16473 ) ;
#13905 = EDGE_CURVE ( 'NONE', #5721, #8621, #11916, .T. ) ;
#13906 = ORIENTED_EDGE ( 'NONE', *, *, #2737, .T. ) ;
#13907 = CIRCLE ( 'NONE', #24834, 3.800000000000018918 ) ;
#13908 = CARTESIAN_POINT ( 'NONE',  ( -50.00000000000000000, 9.797174393178839462E-16, 61.99999999999999289 ) ) ;
#13909 = CARTESIAN_POINT ( 'NONE',  ( -35.50000000000000711, -112.9876085932806262, 1.879154677457530065 ) ) ;
#13910 = ORIENTED_EDGE ( 'NONE', *, *, #29917, .T. ) ;
#13911 = ORIENTED_EDGE ( 'NONE', *, *, #8806, .T. ) ;
#13912 = CARTESIAN_POINT ( 'NONE',  ( -35.54388159064475872, -112.6276912846090568, 5.816024454178449155 ) ) ;
#13913 = FACE_BOUND ( 'NONE', #34994, .T. ) ;
#13914 = ORIENTED_EDGE ( 'NONE', *, *, #29353, .F. ) ;
#13915 = ORIENTED_EDGE ( 'NONE', *, *, #11570, .T. ) ;
#13916 = CARTESIAN_POINT ( 'NONE',  ( -34.50000000000000000, -112.0140978167138712, -0.4685323525984295134 ) ) ;
#13917 = LINE ( 'NONE', #2959, #2821 ) ;
#13918 = AXIS2_PLACEMENT_3D ( 'NONE', #6426, #17574, #9313 ) ;
#13919 = COLOUR_RGB ( '', 0.40784314, 0.44705882, 0.49803922) ;
#13920 = AXIS2_PLACEMENT_3D ( 'NONE', #6036, #19353, #11440 ) ;
#13921 = DIRECTION ( 'NONE',  ( -1.000000000000000000, 0.000000000000000000, 0.000000000000000000 ) ) ;
#13922 = EDGE_CURVE ( 'NONE', #18458, #11984, #9605, .T. ) ;
#13923 = CARTESIAN_POINT ( 'NONE',  ( -35.50000000000000000, -113.9929510916435049, 10.50625754673586876 ) ) ;
#13924 = EDGE_CURVE ( 'NONE', #11089, #28349, #7878, .T. ) ;
#13925 = CARTESIAN_POINT ( 'NONE',  ( 8.000000000000000000, 16.94522934049215124, 8.128228055638924587 ) ) ;
#13926 = CARTESIAN_POINT ( 'NONE',  ( 50.00000000000000000, 10.00000000000000888, 110.0000000000000000 ) ) ;
#13927 = CARTESIAN_POINT ( 'NONE',  ( -34.50000000000000000, -112.6572589393539516, 2.844055607295835397 ) ) ;
#13928 = CARTESIAN_POINT ( 'NONE',  ( -39.00000000000000000, -115.9929510916434481, 11.21034663311206181 ) ) ;
#13929 = UNCERTAINTY_MEASURE_WITH_UNIT (LENGTH_MEASURE( 1.000000000000000082E-05 ), #15783, 'distance_accuracy_value', 'NONE');
#13930 = CYLINDRICAL_SURFACE ( 'NONE', #5520, 13.99999999999999822 ) ;
#13931 = AXIS2_PLACEMENT_3D ( 'NONE', #11945, #601, #11584 ) ;
#13932 = CARTESIAN_POINT ( 'NONE',  ( 8.000000000000000000, -3.968388925834962500, 21.63912866391138934 ) ) ;
#13933 = ADVANCED_FACE ( 'NONE', ( #4838, #35433 ), #27516, .F. ) ;
#13934 = ORIENTED_EDGE ( 'NONE', *, *, #13006, .T. ) ;
#13935 = CARTESIAN_POINT ( 'NONE',  ( -38.00000068757622529, -115.9929510916434481, 12.61439929482944855 ) ) ;
#13936 = CYLINDRICAL_SURFACE ( 'NONE', #2760, 20.00000000000000355 ) ;
#13937 = EDGE_CURVE ( 'NONE', #31771, #16680, #13063, .T. ) ;
#13938 = LINE ( 'NONE', #1315, #9357 ) ;
#13939 = ORIENTED_EDGE ( 'NONE', *, *, #23028, .T. ) ;
#13940 = CARTESIAN_POINT ( 'NONE',  ( 4.000000000000003553, -40.47821179127737423, 32.64221760512746329 ) ) ;
#13941 = DIRECTION ( 'NONE',  ( 0.000000000000000000, 0.000000000000000000, 1.000000000000000000 ) ) ;
#13942 = CIRCLE ( 'NONE', #15076, 47.49900000000001654 ) ;
#13943 = DIRECTION ( 'NONE',  ( -1.000000000000000000, 0.000000000000000000, 0.000000000000000000 ) ) ;
#13944 = CYLINDRICAL_SURFACE ( 'NONE', #9802, 19.99999999999998579 ) ;
#13945 = CONTEXT_DEPENDENT_SHAPE_REPRESENTATION ( #33361, #17249 ) ;
#13946 = CIRCLE ( 'NONE', #3035, 22.00000000000000000 ) ;
#13947 = FACE_OUTER_BOUND ( 'NONE', #31979, .T. ) ;
#13948 = DIRECTION ( 'NONE',  ( 0.000000000000000000, 0.1736481776669211718, 0.9848077530122096857 ) ) ;
#13949 = ORIENTED_EDGE ( 'NONE', *, *, #33158, .F. ) ;
#13950 = CARTESIAN_POINT ( 'NONE',  ( -4.747884751462066788, -5.143694235356003119, -0.7999999999999951594 ) ) ;
#13951 = CARTESIAN_POINT ( 'NONE',  ( 8.000000000000000000, 14.87816164169121080, -4.342730381189718436 ) ) ;
#13952 = DIRECTION ( 'NONE',  ( -1.000000000000000000, -0.000000000000000000, 0.000000000000000000 ) ) ;
#13953 = ORIENTED_EDGE ( 'NONE', *, *, #3789, .T. ) ;
#13954 = CARTESIAN_POINT ( 'NONE',  ( -37.47347596530441649, -113.0245472910329880, 8.027725545821551734 ) ) ;
#13955 = ORIENTED_EDGE ( 'NONE', *, *, #2897, .F. ) ;
#13957 = VERTEX_POINT ( 'NONE', #5540 ) ;
#13956 = AXIS2_PLACEMENT_3D ( 'NONE', #7243, #14984, #34806 ) ;
#13958 = ORIENTED_EDGE ( 'NONE', *, *, #33503, .F. ) ;
#13959 = CARTESIAN_POINT ( 'NONE',  ( 7.999999999999992895, -46.21320724403641833, -10.97699764142004497 ) ) ;
#13960 = EDGE_CURVE ( 'NONE', #656, #6464, #7521, .T. ) ;
#13961 = DIRECTION ( 'NONE',  ( -1.174092375852890260E-15, 4.222049128630259891E-16, 1.000000000000000000 ) ) ;
#13962 = EDGE_CURVE ( 'NONE', #10094, #33676, #17632, .T. ) ;
#13963 = VECTOR ( 'NONE', #26934, 1000.000000000000000 ) ;
#13964 = CARTESIAN_POINT ( 'NONE',  ( -35.50000000000000711, -114.9492820284331742, 10.20776876943783940 ) ) ;
#13965 = CIRCLE ( 'NONE', #30649, 20.00000000000000711 ) ;
#13966 = FACE_OUTER_BOUND ( 'NONE', #1030, .T. ) ;
#13967 = CIRCLE ( 'NONE', #30653, 20.00000000000000711 ) ;
#13968 = CARTESIAN_POINT ( 'NONE',  ( -46.00000000000000000, -25.98076211353320275, 84.99999999999992895 ) ) ;
#13969 = CARTESIAN_POINT ( 'NONE',  ( 7.999999999999992895, -20.99948489194393275, -42.60488980472803888 ) ) ;
#13970 = DIRECTION ( 'NONE',  ( 0.000000000000000000, -0.5877852522924624790, -0.8090169943749551118 ) ) ;
#13971 = SHAPE_REPRESENTATION ( 'Mounting Base Plate Frame', ( #21307 ), #13295 ) ;
#13972 = FACE_BOUND ( 'NONE', #19629, .T. ) ;
#13973 = CARTESIAN_POINT ( 'NONE',  ( -39.00000000000000000, -115.9929510916434481, 12.56351784598954779 ) ) ;
#13974 = CARTESIAN_POINT ( 'NONE',  ( -35.00000000000000000, -114.0000000000003411, 9.500000000000035527 ) ) ;
#13975 = DIRECTION ( 'NONE',  ( 1.000000000000000000, 0.000000000000000000, 0.000000000000000000 ) ) ;
#13976 = DIRECTION ( 'NONE',  ( 1.000000000000000000, -0.000000000000000000, 0.000000000000000000 ) ) ;
#13977 = CARTESIAN_POINT ( 'NONE',  ( -21.15833593587365513, -20.27980021920970799, 72.12564434701783966 ) ) ;
#13978 = DIRECTION ( 'NONE',  ( 1.000000000000000000, -5.339440136655842133E-16, -1.047965281155519420E-16 ) ) ;
#13979 = CYLINDRICAL_SURFACE ( 'NONE', #19528, 8.000000000000000000 ) ;
#13980 = ORIENTED_EDGE ( 'NONE', *, *, #27077, .T. ) ;
#13981 = CARTESIAN_POINT ( 'NONE',  ( -35.00000000000000000, -113.9407375970686900, 8.496475545821551734 ) ) ;
#13982 = LINE ( 'NONE', #32722, #23876 ) ;
#13983 = DIRECTION ( 'NONE',  ( -1.000000000000000000, 0.000000000000000000, 0.000000000000000000 ) ) ;
#13984 = CARTESIAN_POINT ( 'NONE',  ( 7.999999999999992895, 0.000000000000000000, 0.000000000000000000 ) ) ;
#13985 = VERTEX_POINT ( 'NONE', #5370 ) ;
#13986 = ORIENTED_EDGE ( 'NONE', *, *, #6825, .F. ) ;
#13987 = AXIS2_PLACEMENT_3D ( 'NONE', #2237, #35521, #5107 ) ;
#13988 = CARTESIAN_POINT ( 'NONE',  ( 0.000000000000000000, 46.19362259308833529, 8.585149169758651055 ) ) ;
#13989 = AXIS2_PLACEMENT_3D ( 'NONE', #22290, #16345, #24829 ) ;
#13990 = FACE_OUTER_BOUND ( 'NONE', #13727, .T. ) ;
#13991 = ORIENTED_EDGE ( 'NONE', *, *, #6869, .T. ) ;
#13992 = EDGE_LOOP ( 'NONE', ( #34190, #24416, #20586, #26632 ) ) ;
#13993 = DIRECTION ( 'NONE',  ( -1.047965281155519667E-16, -6.938893903907193865E-17, -1.000000000000000000 ) ) ;
#13994 = CARTESIAN_POINT ( 'NONE',  ( 3.799999999999999822, 4.653657836759942730E-16, -33.50000000000000711 ) ) ;
#13995 = DIRECTION ( 'NONE',  ( 1.000000000000000000, 0.000000000000000000, 0.000000000000000000 ) ) ;
#13996 = CARTESIAN_POINT ( 'NONE',  ( 7.999999999999992895, 0.000000000000000000, 0.000000000000000000 ) ) ;
#13997 = ORIENTED_EDGE ( 'NONE', *, *, #4931, .F. ) ;
#13998 = EDGE_LOOP ( 'NONE', ( #6730, #34726, #989, #30920, #20650, #2855, #22424, #23796, #12732, #25039, #27715, #1237, #22643, #7170, #31957, #31795, #19279, #26684, #7370, #21346, #3352, #26805, #15785, #32988, #20195, #29098, #14793, #17577, #6514, #22268, #295, #2931, #14503, #14581, #5511, #28841, #29284, #19548, #33083, #24119, #1915, #26836, #23612, #32325, #12280, #22972, #604, #24173, #25181, #27213, #24356, #24367, #21697, #23804, #17826, #28743, #19407, #1921, #4261, #20568, #16155, #23269, #28965, #3214, #3878, #18635, #23622, #24232, #34161, #27991, #22657, #13391, #3390, #25932, #35063, #4427, #28667, #10608, #2806, #5679, #556, #19243, #16590, #15760, #19771, #17206, #19174, #23935, #5583, #15757, #30658, #34961, #20583, #34816, #20329, #3608, #3457, #24245, #1463, #32909, #18425, #12456, #34829, #6318, #28286, #28998, #29375, #14833, #9736, #15566, #6516, #10381, #6206, #34224, #10986, #14770, #25550, #28435, #26277, #33865, #16561, #3473, #585, #29415, #22883, #22930, #20866, #28060, #34376, #26224, #10145, #30833, #26403, #10391, #13382, #8197, #16366, #29198, #34290, #10911, #30810, #3083, #19635, #15487, #33295, #7411, #6096, #868, #4139, #8790, #12394, #744, #10648, #15676, #25730, #24137, #615, #3930, #15069, #11562, #23742, #5557, #3233, #1078, #10272, #5777, #1294, #29509, #6446, #15885, #14469, #26087, #8941, #25401, #17964, #11530, #5760, #27387, #25328, #8435, #33139, #15187, #31402, #23225, #34908, #18690, #8718, #7609, #26116, #16413, #3961, #22088, #9864, #24449, #28934, #25975, #12449, #12934, #32958, #13293, #24847, #29252, #26367 ) ) ;
#13999 = AXIS2_PLACEMENT_3D ( 'NONE', #17407, #14187, #19572 ) ;
#14000 = EDGE_CURVE ( 'NONE', #11309, #32739, #2674, .T. ) ;
#14001 = DIRECTION ( 'NONE',  ( 1.000000000000000000, -5.339440136655842133E-16, 1.047965281155515476E-16 ) ) ;
#14002 = CARTESIAN_POINT ( 'NONE',  ( 70.00000000000001421, 75.33903961282864259, 25.84872029956371975 ) ) ;
#14003 = ORIENTED_EDGE ( 'NONE', *, *, #2033, .F. ) ;
#14004 = DIRECTION ( 'NONE',  ( -1.000000000000000000, -1.502314598737158292E-16, -8.673617379884052728E-17 ) ) ;
#14005 = CARTESIAN_POINT ( 'NONE',  ( -34.50000000000000000, -114.3474311500471430, -1.624782352598427959 ) ) ;
#14006 = AXIS2_PLACEMENT_3D ( 'NONE', #4550, #6676, #15481 ) ;
#14007 = CARTESIAN_POINT ( 'NONE',  ( -37.62254989966454133, -114.9929510916434339, 14.11371147303758278 ) ) ;
#14008 = CARTESIAN_POINT ( 'NONE',  ( -35.50000000000000000, -113.9917898843777522, 10.50611893782865813 ) ) ;
#14009 = CARTESIAN_POINT ( 'NONE',  ( 4.000000000000000000, -19.60123832284022782, 3.973846525876368219 ) ) ;
#14010 = EDGE_CURVE ( 'NONE', #7515, #31797, #24628, .T. ) ;
#14011 = CARTESIAN_POINT ( 'NONE',  ( -36.15625000000007816, -114.9929510916434339, 14.11852480586264846 ) ) ;
#14012 = CARTESIAN_POINT ( 'NONE',  ( 4.000000000000003553, 3.268936481846368203, -13.61301047812914256 ) ) ;
#14013 = EDGE_LOOP ( 'NONE', ( #9932, #24406, #6118, #3296 ) ) ;
#14014 = DIRECTION ( 'NONE',  ( -1.000000000000000000, 0.000000000000000000, 0.000000000000000000 ) ) ;
#14015 = DIRECTION ( 'NONE',  ( 0.000000000000000000, 0.000000000000000000, 1.000000000000000000 ) ) ;
#14016 = DIRECTION ( 'NONE',  ( 1.000000000000000000, 0.000000000000000000, 0.000000000000000000 ) ) ;
#14017 = CARTESIAN_POINT ( 'NONE',  ( -34.49999999999998579, -25.98076211353322051, 84.99999999999992895 ) ) ;
#14018 = EDGE_LOOP ( 'NONE', ( #32162, #9771, #7246, #76 ) ) ;
#14019 = CARTESIAN_POINT ( 'NONE',  ( 0.000000000000000000, -44.25018368420724357, -27.31155879685229237 ) ) ;
#14020 = ORIENTED_EDGE ( 'NONE', *, *, #4659, .T. ) ;
#14021 = CARTESIAN_POINT ( 'NONE',  ( -37.05926240293133134, -116.9999999999999858, 4.878524454178448266 ) ) ;
#14022 = DIRECTION ( 'NONE',  ( 1.000000000000000000, -5.339440136655842133E-16, -1.047965281155519420E-16 ) ) ;
#14023 = CARTESIAN_POINT ( 'NONE',  ( -35.50000000000000711, -112.8835768857893527, -1.616767172155725740 ) ) ;
#14024 = ORIENTED_EDGE ( 'NONE', *, *, #4352, .F. ) ;
#14025 = VERTEX_POINT ( 'NONE', #8400 ) ;
#14026 = DIRECTION ( 'NONE',  ( -0.000000000000000000, 0.000000000000000000, -1.000000000000000000 ) ) ;
#14027 = DIRECTION ( 'NONE',  ( 0.000000000000000000, 0.000000000000000000, -1.000000000000000000 ) ) ;
#14028 = ORIENTED_EDGE ( 'NONE', *, *, #24706, .F. ) ;
#14029 = CARTESIAN_POINT ( 'NONE',  ( 8.000000000000000000, 3.384281271888069487, -18.48663108841355296 ) ) ;
#14030 = CIRCLE ( 'NONE', #2576, 4.000000000000000000 ) ;
#14031 = DIRECTION ( 'NONE',  ( 0.000000000000000000, 0.000000000000000000, -1.000000000000000000 ) ) ;
#14032 = VERTEX_POINT ( 'NONE', #28034 ) ;
#14033 = ORIENTED_EDGE ( 'NONE', *, *, #29013, .F. ) ;
#14034 = CARTESIAN_POINT ( 'NONE',  ( 46.00000000000000000, 0.000000000000000000, 70.00000000000000000 ) ) ;
#14035 = FACE_OUTER_BOUND ( 'NONE', #13528, .T. ) ;
#14036 = ORIENTED_EDGE ( 'NONE', *, *, #637, .T. ) ;
#14037 = ORIENTED_EDGE ( 'NONE', *, *, #32838, .T. ) ;
#14038 = CARTESIAN_POINT ( 'NONE',  ( -35.50000000000000000, -113.6974040292745656, 2.970979214817929481 ) ) ;
#14039 = ADVANCED_FACE ( 'NONE', ( #30552 ), #3196, .F. ) ;
#14040 = ADVANCED_FACE ( 'NONE', ( #33789 ), #30387, .F. ) ;
#14041 = DIRECTION ( 'NONE',  ( 9.266685234918781277E-17, 8.187894806610533430E-16, -1.000000000000000000 ) ) ;
#14042 = VERTEX_POINT ( 'NONE', #11806 ) ;
#14043 = CARTESIAN_POINT ( 'NONE',  ( -36.15625000000007816, -114.9929510916434339, 13.11852480586264669 ) ) ;
#14044 = CARTESIAN_POINT ( 'NONE',  ( -36.31249999999994316, -113.9929510916434339, 14.11852480586265024 ) ) ;
#14045 = FACE_OUTER_BOUND ( 'NONE', #14204, .T. ) ;
#14046 = CARTESIAN_POINT ( 'NONE',  ( 46.00000000000000000, -25.98076211353320275, 84.99999999999992895 ) ) ;
#14047 = EDGE_CURVE ( 'NONE', #29687, #31732, #14139, .T. ) ;
#14048 = CARTESIAN_POINT ( 'NONE',  ( -34.50000000000000000, -113.9929510916434339, 12.26648026267477398 ) ) ;
#14049 = CARTESIAN_POINT ( 'NONE',  ( -38.99699093265173389, -114.9929510916434339, 12.71660600561481402 ) ) ;
#14050 = CARTESIAN_POINT ( 'NONE',  ( -35.50000000000000711, -114.9929510916434339, 10.85830208992344303 ) ) ;
#14051 =( LENGTH_UNIT ( ) NAMED_UNIT ( * ) SI_UNIT ( .MILLI., .METRE. ) );
#14053 = AXIS2_PLACEMENT_3D ( 'NONE', #16679, #306, #19551 ) ;
#14052 = CARTESIAN_POINT ( 'NONE',  ( 8.000000000000007105, 5.363026430117337817, -9.919332006307165273 ) ) ;
#14054 = CIRCLE ( 'NONE', #5470, 15.49899999999998457 ) ;
#14055 = VERTEX_POINT ( 'NONE', #8743 ) ;
#14056 = ORIENTED_EDGE ( 'NONE', *, *, #33047, .F. ) ;
#14057 = FACE_OUTER_BOUND ( 'NONE', #16420, .T. ) ;
#14058 = CARTESIAN_POINT ( 'NONE',  ( 0.000000000000000000, 0.000000000000000000, -40.40000000000000568 ) ) ;
#14059 = AXIS2_PLACEMENT_3D ( 'NONE', #2002, #12977, #34765 ) ;
#14060 = VERTEX_POINT ( 'NONE', #22785 ) ;
#14061 = CARTESIAN_POINT ( 'NONE',  ( -21.15833593587365513, -13.10640646055107084, 90.70096189432331357 ) ) ;
#14062 = ORIENTED_EDGE ( 'NONE', *, *, #9258, .T. ) ;
#14063 = CARTESIAN_POINT ( 'NONE',  ( -35.50000000000000000, -112.9977353549762000, -0.6247823525983134951 ) ) ;
#14064 = CARTESIAN_POINT ( 'NONE',  ( 8.000000000000000000, -16.92083251265328769, 4.460989585140905156 ) ) ;
#14065 = CARTESIAN_POINT ( 'NONE',  ( -36.11231047232249125, -112.0245472910329880, 4.222274454178449155 ) ) ;
#14066 = DIRECTION ( 'NONE',  ( 0.000000000000000000, -1.000000000000000000, 0.000000000000000000 ) ) ;
#14067 = EDGE_CURVE ( 'NONE', #1452, #31709, #29770, .T. ) ;
#14068 = CIRCLE ( 'NONE', #10068, 13.99999999999999645 ) ;
#14069 = VERTEX_POINT ( 'NONE', #484 ) ;
#14070 = DIRECTION ( 'NONE',  ( 0.000000000000000000, 0.000000000000000000, -1.000000000000000000 ) ) ;
#14071 = CARTESIAN_POINT ( 'NONE',  ( -35.50000000000000000, -117.0140814545088688, -0.6738694770610542673 ) ) ;
#14072 = VERTEX_POINT ( 'NONE', #11462 ) ;
#14073 = ORIENTED_EDGE ( 'NONE', *, *, #15260, .T. ) ;
#14074 = CARTESIAN_POINT ( 'NONE',  ( -37.76916472181487450, -111.9754527089670404, 5.534774454178449155 ) ) ;
#14075 =( NAMED_UNIT ( * ) PLANE_ANGLE_UNIT ( ) SI_UNIT ( $, .RADIAN. ) );
#14076 = CARTESIAN_POINT ( 'NONE',  ( 7.999999999999992895, 9.744342220504046637, -46.48873837489789196 ) ) ;
#14077 = VERTEX_POINT ( 'NONE', #17023 ) ;
#14078 = VERTEX_POINT ( 'NONE', #19382 ) ;
#14079 = CARTESIAN_POINT ( 'NONE',  ( -34.50000000000000000, -112.1222502514821144, 1.343475657184566296 ) ) ;
#14080 = DIRECTION ( 'NONE',  ( 1.000000000000000000, 1.836970198721029934E-16, 0.000000000000000000 ) ) ;
#14081 = EDGE_CURVE ( 'NONE', #27829, #5217, #10712, .T. ) ;
#14082 = AXIS2_PLACEMENT_3D ( 'NONE', #6572, #20240, #3541 ) ;
#14083 = EDGE_CURVE ( 'NONE', #5216, #2854, #16849, .T. ) ;
#14084 = EDGE_CURVE ( 'NONE', #4520, #13350, #2686, .T. ) ;
#14085 = EDGE_LOOP ( 'NONE', ( #31718, #24320, #31171, #29042 ) ) ;
#14086 = CARTESIAN_POINT ( 'NONE',  ( 3.872983346207517386, -1.000000000000028644, -44.50000000000000000 ) ) ;
#14087 = AXIS2_PLACEMENT_3D ( 'NONE', #27326, #6237, #25688 ) ;
#14088 = CARTESIAN_POINT ( 'NONE',  ( -35.50000000000000000, -113.9929510916434339, 10.94631322572069365 ) ) ;
#14089 = LINE ( 'NONE', #22191, #26465 ) ;
#14090 = CARTESIAN_POINT ( 'NONE',  ( 46.00000000000000000, 0.000000000000000000, 70.00000000000000000 ) ) ;
#14091 = ADVANCED_FACE ( 'NONE', ( #11289 ), #33423, .T. ) ;
#14092 = CARTESIAN_POINT ( 'NONE',  ( -34.50000000000000000, -116.0140978167138712, 0.6252176474015648244 ) ) ;
#14093 = EDGE_CURVE ( 'NONE', #864, #33645, #344, .T. ) ;
#14094 = CARTESIAN_POINT ( 'NONE',  ( -39.00000000000000000, -115.9929510916434481, 12.59102132592609102 ) ) ;
#14095 = AXIS2_PLACEMENT_3D ( 'NONE', #26300, #18176, #23770 ) ;
#14096 = DIRECTION ( 'NONE',  ( 0.000000000000000000, 0.000000000000000000, -1.000000000000000000 ) ) ;
#14097 = DIRECTION ( 'NONE',  ( 1.000000000000000000, -5.339440136655842133E-16, -1.047965281155519420E-16 ) ) ;
#14098 = ORIENTED_EDGE ( 'NONE', *, *, #22855, .F. ) ;
#14099 = DIRECTION ( 'NONE',  ( 0.000000000000000000, 0.000000000000000000, -1.000000000000000000 ) ) ;
#14100 = LINE ( 'NONE', #11415, #8166 ) ;
#14101 = DIRECTION ( 'NONE',  ( 0.000000000000000000, 0.000000000000000000, -1.000000000000000000 ) ) ;
#14102 = ORIENTED_EDGE ( 'NONE', *, *, #11537, .T. ) ;
#14103 = CARTESIAN_POINT ( 'NONE',  ( 4.000000000000000000, -19.60123832284014611, -3.973846525876633340 ) ) ;
#14104 = DIRECTION ( 'NONE',  ( -1.000000000000000000, 0.000000000000000000, 0.000000000000000000 ) ) ;
#14105 = AXIS2_PLACEMENT_3D ( 'NONE', #27814, #19331, #25101 ) ;
#14106 = DIRECTION ( 'NONE',  ( 0.000000000000000000, 0.000000000000000000, -1.000000000000000000 ) ) ;
#14107 = DIRECTION ( 'NONE',  ( 0.000000000000000000, 0.000000000000000000, 1.000000000000000000 ) ) ;
#14108 = ITEM_DEFINED_TRANSFORMATION ( 'NONE', 'NONE', #29896,  #21307 ) ;
#14109 = DIRECTION ( 'NONE',  ( 0.000000000000000000, -1.000000000000000000, 0.000000000000000000 ) ) ;
#14110 = CARTESIAN_POINT ( 'NONE',  ( 0.000000000000000000, -1.693188892523841194, 15.40623615209871389 ) ) ;
#14111 = EDGE_CURVE ( 'NONE', #1026, #28288, #17573, .T. ) ;
#14112 = EDGE_LOOP ( 'NONE', ( #30300, #24662, #693, #24806 ) ) ;
#14113 = CYLINDRICAL_SURFACE ( 'NONE', #349, 52.00000000000000711 ) ;
#14114 = CARTESIAN_POINT ( 'NONE',  ( -1.398397006337051440, -6.091550361990532458, -0.7999999999999951594 ) ) ;
#14115 = EDGE_CURVE ( 'NONE', #1605, #18539, #6105, .T. ) ;
#14116 = DIRECTION ( 'NONE',  ( -1.000000000000000000, 0.000000000000000000, 0.000000000000000000 ) ) ;
#14117 = VERTEX_POINT ( 'NONE', #22263 ) ;
#14118 = CARTESIAN_POINT ( 'NONE',  ( -36.64504884055821776, -112.9754527089670688, 5.215225545821552622 ) ) ;
#14119 = EDGE_LOOP ( 'NONE', ( #19946, #4452, #2414, #30942 ) ) ;
#14120 = EDGE_CURVE ( 'NONE', #6500, #5335, #19874, .T. ) ;
#14121 =( NAMED_UNIT ( * ) SI_UNIT ( $, .STERADIAN. ) SOLID_ANGLE_UNIT ( ) );
#14122 = CIRCLE ( 'NONE', #34259, 20.00000000000000355 ) ;
#14123 = ORIENTED_EDGE ( 'NONE', *, *, #10593, .T. ) ;
#14124 = ORIENTED_EDGE ( 'NONE', *, *, #16571, .T. ) ;
#14125 = LINE ( 'NONE', #3000, #5142 ) ;
#14126 = EDGE_CURVE ( 'NONE', #11644, #485, #27687, .T. ) ;
#14127 = EDGE_CURVE ( 'NONE', #14555, #33603, #2095, .T. ) ;
#14128 = CARTESIAN_POINT ( 'NONE',  ( -35.50000000000000711, -113.2224311500466030, -1.624782352598427959 ) ) ;
#14129 = DIRECTION ( 'NONE',  ( 1.000000000000000000, -0.000000000000000000, 0.000000000000000000 ) ) ;
#14130 = CIRCLE ( 'NONE', #29674, 52.00000000000000711 ) ;
#14131 = CARTESIAN_POINT ( 'NONE',  ( 7.999999999999992895, 15.49408907645171851, 44.90087086784599535 ) ) ;
#14132 = DIRECTION ( 'NONE',  ( 0.000000000000000000, 0.000000000000000000, 1.000000000000000000 ) ) ;
#14133 = DIRECTION ( 'NONE',  ( 0.000000000000000000, -0.9980267284282722251, 0.06279051952930256308 ) ) ;
#14134 = CIRCLE ( 'NONE', #338, 20.00000000000000711 ) ;
#14135 = CIRCLE ( 'NONE', #29085, 5.016000000000010672 ) ;
#14136 = EDGE_CURVE ( 'NONE', #26858, #14835, #19547, .T. ) ;
#14137 = CARTESIAN_POINT ( 'NONE',  ( -34.50000000000000000, -114.8847986568751907, 10.03799953695244618 ) ) ;
#14138 = CARTESIAN_POINT ( 'NONE',  ( 38.00000000000000000, 6.980486755139912911E-15, 0.000000000000000000 ) ) ;
#14139 = CIRCLE ( 'NONE', #33127, 47.49900000000001654 ) ;
#14140 = DIRECTION ( 'NONE',  ( -0.000000000000000000, 0.000000000000000000, -1.000000000000000000 ) ) ;
#14141 = CARTESIAN_POINT ( 'NONE',  ( -37.34375000000001421, -115.9929510916434481, 14.11852480586265024 ) ) ;
#14142 = CARTESIAN_POINT ( 'NONE',  ( -35.50000000000000711, -112.0140978167138712, 0.7189676474015718188 ) ) ;
#14143 = CIRCLE ( 'NONE', #19304, 7.999999999999992895 ) ;
#14144 = DIRECTION ( 'NONE',  ( -1.000000000000000000, 0.000000000000000000, 0.000000000000000000 ) ) ;
#14145 = CIRCLE ( 'NONE', #34288, 4.980000000000017302 ) ;
#14146 = CARTESIAN_POINT ( 'NONE',  ( -34.49999999999998579, -3.734562119078923992, 144.3977620171895637 ) ) ;
#14147 = DIRECTION ( 'NONE',  ( 0.000000000000000000, 0.8090169943749488946, -0.5877852522924709167 ) ) ;
#14148 = DIRECTION ( 'NONE',  ( 0.000000000000000000, 0.000000000000000000, -1.000000000000000000 ) ) ;
#14149 = EDGE_LOOP ( 'NONE', ( #3826, #35191, #32996, #21412 ) ) ;
#14150 = CARTESIAN_POINT ( 'NONE',  ( -35.02454729103298803, -113.1123104723225197, 9.902725545821557063 ) ) ;
#14151 = CARTESIAN_POINT ( 'NONE',  ( 0.000000000000000000, 19.83898331853701080, -9.508666619816445120 ) ) ;
#14152 = CARTESIAN_POINT ( 'NONE',  ( 0.000000000000000000, -18.48663108841356717, 4.615718728111985136 ) ) ;
#14153 = CARTESIAN_POINT ( 'NONE',  ( 0.000000000000000000, -2.710505431213761085E-17, 29.09999999999999787 ) ) ;
#14154 = ADVANCED_FACE ( 'NONE', ( #31083, #17377 ), #28378, .T. ) ;
#14155 = VERTEX_POINT ( 'NONE', #17741 ) ;
#14156 = CIRCLE ( 'NONE', #24533, 7.499999999999992895 ) ;
#14157 = VERTEX_POINT ( 'NONE', #28742 ) ;
#14158 = EDGE_CURVE ( 'NONE', #16904, #32383, #20610, .T. ) ;
#14159 = CARTESIAN_POINT ( 'NONE',  ( 0.000000000000000000, -44.47301969247433817, -16.68249143361957820 ) ) ;
#14160 = CIRCLE ( 'NONE', #3852, 4.000000000000000000 ) ;
#14161 = EDGE_CURVE ( 'NONE', #21217, #34510, #14222, .T. ) ;
#14162 = DIRECTION ( 'NONE',  ( 1.000000000000000000, 0.000000000000000000, 0.000000000000000000 ) ) ;
#14163 = ORIENTED_EDGE ( 'NONE', *, *, #25405, .T. ) ;
#14164 = VERTEX_POINT ( 'NONE', #23146 ) ;
#14165 = CIRCLE ( 'NONE', #362, 4.800000000000002487 ) ;
#14166 = VECTOR ( 'NONE', #24622, 1000.000000000000000 ) ;
#14167 = AXIS2_PLACEMENT_3D ( 'NONE', #33557, #8886, #22216 ) ;
#14168 = CARTESIAN_POINT ( 'NONE',  ( 0.000000000000000000, -12.30077720129132679, 50.52416135122078344 ) ) ;
#14169 = CIRCLE ( 'NONE', #20478, 14.00000000000000000 ) ;
#14170 = DIRECTION ( 'NONE',  ( 0.000000000000000000, 0.000000000000000000, 1.000000000000000000 ) ) ;
#14171 = ADVANCED_FACE ( 'NONE', ( #18093 ), #17667, .T. ) ;
#14172 = EDGE_CURVE ( 'NONE', #13818, #13511, #4446, .T. ) ;
#14173 = APPLICATION_PROTOCOL_DEFINITION ( 'draft international standard', 'automotive_design', 1998, #14221 ) ;
#14174 = FACE_OUTER_BOUND ( 'NONE', #31907, .T. ) ;
#14176 = ORIENTED_EDGE ( 'NONE', *, *, #23119, .T. ) ;
#14175 = AXIS2_PLACEMENT_3D ( 'NONE', #8735, #14488, #12163 ) ;
#14177 = ORIENTED_EDGE ( 'NONE', *, *, #15082, .F. ) ;
#14178 = LINE ( 'NONE', #22986, #16272 ) ;
#14179 = DIRECTION ( 'NONE',  ( -1.000000000000000000, -0.000000000000000000, -0.000000000000000000 ) ) ;
#14180 = ORIENTED_EDGE ( 'NONE', *, *, #15009, .F. ) ;
#14181 = DIRECTION ( 'NONE',  ( 0.000000000000000000, 0.000000000000000000, 1.000000000000000000 ) ) ;
#14182 = CIRCLE ( 'NONE', #19370, 15.49900000000000233 ) ;
#14183 = DIRECTION ( 'NONE',  ( -1.000000000000000000, 0.000000000000000000, 0.000000000000000000 ) ) ;
#14184 = DIRECTION ( 'NONE',  ( -1.000000000000000000, -1.734723475976807094E-16, -0.000000000000000000 ) ) ;
#14185 = CARTESIAN_POINT ( 'NONE',  ( -34.50000000000000000, -114.2600084737790809, 8.524153227862690585 ) ) ;
#14186 = CIRCLE ( 'NONE', #18790, 19.99999999999998579 ) ;
#14187 = DIRECTION ( 'NONE',  ( -1.000000000000000000, 0.000000000000000000, 0.000000000000000000 ) ) ;
#14188 = PLANE ( 'NONE',  #6504 ) ;
#14189 = CARTESIAN_POINT ( 'NONE',  ( -34.50000000000000000, -114.9929510916434339, 11.21034663311131929 ) ) ;
#14190 = LINE ( 'NONE', #25192, #9016 ) ;
#14191 = VECTOR ( 'NONE', #34676, 1000.000000000000000 ) ;
#14192 = CARTESIAN_POINT ( 'NONE',  ( 7.999999999999992895, 0.000000000000000000, 0.000000000000000000 ) ) ;
#14193 = AXIS2_PLACEMENT_3D ( 'NONE', #10326, #32108, #13029 ) ;
#14194 = CARTESIAN_POINT ( 'NONE',  ( 0.000000000000000000, -22.43957647427129842, -41.27978878573651400 ) ) ;
#14195 = DIRECTION ( 'NONE',  ( -0.000000000000000000, 0.7535859266250379829, 0.6573494133204068612 ) ) ;
#14196 = VERTEX_POINT ( 'NONE', #26213 ) ;
#14197 = AXIS2_PLACEMENT_3D ( 'NONE', #32534, #19033, #21911 ) ;
#14198 = LINE ( 'NONE', #8262, #17569 ) ;
#14199 = ORIENTED_EDGE ( 'NONE', *, *, #6449, .F. ) ;
#14200 = CARTESIAN_POINT ( 'NONE',  ( -38.18337828418795965, -110.9754527089670546, 2.534774454178448710 ) ) ;
#14201 = CYLINDRICAL_SURFACE ( 'NONE', #15770, 7.199999999999993960 ) ;
#14202 = CARTESIAN_POINT ( 'NONE',  ( -35.50000000000000711, -112.2144317118258527, -1.239329810084414341 ) ) ;
#14203 = VERTEX_POINT ( 'NONE', #15387 ) ;
#14204 = EDGE_LOOP ( 'NONE', ( #28826, #19513, #1891, #32864 ) ) ;
#14205 = ADVANCED_FACE ( 'NONE', ( #4095 ), #1024, .T. ) ;
#14206 = PLANE ( 'NONE',  #1057 ) ;
#14207 = DIRECTION ( 'NONE',  ( 0.000000000000000000, 0.6427876096865349220, 0.7660444431189816772 ) ) ;
#14208 = ORIENTED_EDGE ( 'NONE', *, *, #17207, .F. ) ;
#14209 = AXIS2_PLACEMENT_3D ( 'NONE', #31952, #7288, #15549 ) ;
#14210 = CARTESIAN_POINT ( 'NONE',  ( 0.000000000000000000, -17.47118961583602470, 0.9861715913087032437 ) ) ;
#14211 = CARTESIAN_POINT ( 'NONE',  ( 4.000000000000003553, -51.93417535146740960, -2.615612846549736581 ) ) ;
#14212 = VERTEX_POINT ( 'NONE', #12714 ) ;
#14213 = ORIENTED_EDGE ( 'NONE', *, *, #9269, .T. ) ;
#14214 = DIRECTION ( 'NONE',  ( 0.000000000000000000, 0.000000000000000000, 1.000000000000000000 ) ) ;
#14215 = AXIS2_PLACEMENT_3D ( 'NONE', #12987, #4726, #26682 ) ;
#14216 =( NAMED_UNIT ( * ) SI_UNIT ( $, .STERADIAN. ) SOLID_ANGLE_UNIT ( ) );
#14217 = DIRECTION ( 'NONE',  ( 1.000000000000000000, -0.000000000000000000, 0.000000000000000000 ) ) ;
#14218 = ORIENTED_EDGE ( 'NONE', *, *, #26936, .F. ) ;
#14219 = ORIENTED_EDGE ( 'NONE', *, *, #16541, .F. ) ;
#14220 = CARTESIAN_POINT ( 'NONE',  ( -34.50000000000000000, -116.9884631899972476, -0.9506101647064282290 ) ) ;
#14221 = APPLICATION_CONTEXT ( 'automotive_design' ) ;
#14222 = CIRCLE ( 'NONE', #23342, 17.49900000000001299 ) ;
#14223 = ORIENTED_EDGE ( 'NONE', *, *, #15219, .T. ) ;
#14224 = CARTESIAN_POINT ( 'NONE',  ( -37.24999999999992895, -114.9929510916434339, 13.11852480586264669 ) ) ;
#14225 = CARTESIAN_POINT ( 'NONE',  ( -35.90191880024782023, -113.9929510916434339, 14.11551573851449071 ) ) ;
#14226 = CARTESIAN_POINT ( 'NONE',  ( 7.999999999999992895, 46.90537658765334328, -2.727856614653800804 ) ) ;
#14227 = DIRECTION ( 'NONE',  ( 0.000000000000000000, 0.000000000000000000, 1.000000000000000000 ) ) ;
#14228 = CARTESIAN_POINT ( 'NONE',  ( -34.50000000000000000, -113.9929510916434339, 10.52000928670414126 ) ) ;
#14229 = CARTESIAN_POINT ( 'NONE',  ( -38.99879592093640923, -114.9929510916434339, 12.67985367974111455 ) ) ;
#14230 = CARTESIAN_POINT ( 'NONE',  ( -35.50000000000000711, -114.9929517792218689, 10.50900788599415314 ) ) ;
#14231 = VECTOR ( 'NONE', #2934, 1000.000000000000000 ) ;
#14232 = CARTESIAN_POINT ( 'NONE',  ( 7.999999999999992895, 35.11945359308165138, -38.34871548465979174 ) ) ;
#14233 = CARTESIAN_POINT ( 'NONE',  ( 0.000000000000000000, 8.931325931664597206, 16.53603053422209612 ) ) ;
#14234 = VECTOR ( 'NONE', #24131, 1000.000000000000000 ) ;
#14235 = ORIENTED_EDGE ( 'NONE', *, *, #11054, .F. ) ;
#14236 = ORIENTED_EDGE ( 'NONE', *, *, #33243, .F. ) ;
#14237 = CARTESIAN_POINT ( 'NONE',  ( 7.999999999999992895, -0.2227391519119825691, 46.98410307550729215 ) ) ;
#14238 = DIRECTION ( 'NONE',  ( -1.000000000000000000, 0.000000000000000000, 0.000000000000000000 ) ) ;
#14239 = AXIS2_PLACEMENT_3D ( 'NONE', #34382, #23384, #25747 ) ;
#14240 = ORIENTED_EDGE ( 'NONE', *, *, #11890, .F. ) ;
#14241 = CARTESIAN_POINT ( 'NONE',  ( 8.000000000000000000, 11.11653975335790179, 12.74840161668735661 ) ) ;
#14242 = ORIENTED_EDGE ( 'NONE', *, *, #5842, .T. ) ;
#14243 = ADVANCED_FACE ( 'NONE', ( #26398 ), #7302, .T. ) ;
#14244 = CARTESIAN_POINT ( 'NONE',  ( -35.50000000000000000, -115.0140978167138428, -0.6247823525986679893 ) ) ;
#14245 = DIRECTION ( 'NONE',  ( 0.000000000000000000, 0.9510565162951521989, 0.3090169943749515036 ) ) ;
#14246 = CARTESIAN_POINT ( 'NONE',  ( -35.54388159064475872, -112.6276912846090568, 4.316024454178448266 ) ) ;
#14247 = VERTEX_POINT ( 'NONE', #31610 ) ;
#14248 = PRESENTATION_LAYER_ASSIGNMENT (  '', '', ( #4521 ) ) ;
#14249 = CARTESIAN_POINT ( 'NONE',  ( 7.999999999999992895, -20.99948489194452250, 42.60488980472776177 ) ) ;
#14250 = ORIENTED_EDGE ( 'NONE', *, *, #12339, .F. ) ;
#14251 = DIRECTION ( 'NONE',  ( 3.154042683594196600E-16, -1.000000000000000000, 0.000000000000000000 ) ) ;
#14252 = CARTESIAN_POINT ( 'NONE',  ( -35.50000000000000711, -113.2637153405686519, 1.912112492696748989 ) ) ;
#14253 = EDGE_LOOP ( 'NONE', ( #31142, #30121, #14956, #16371 ) ) ;
#14254 = ORIENTED_EDGE ( 'NONE', *, *, #26180, .T. ) ;
#14255 = CARTESIAN_POINT ( 'NONE',  ( -38.97545270896704039, -113.1123104723225197, 5.347274454178449155 ) ) ;
#14256 = EDGE_CURVE ( 'NONE', #17129, #26513, #8973, .T. ) ;
#14257 = CARTESIAN_POINT ( 'NONE',  ( -34.49999999999998579, -27.93100416606583991, 81.50764321173598148 ) ) ;
#14258 = ORIENTED_EDGE ( 'NONE', *, *, #27407, .T. ) ;
#14259 = EDGE_LOOP ( 'NONE', ( #23479, #25548, #5765, #31520 ) ) ;
#14260 = CARTESIAN_POINT ( 'NONE',  ( -34.50000000000000000, -112.0140978167138712, -0.3122823525984337878 ) ) ;
#14261 = FACE_OUTER_BOUND ( 'NONE', #8319, .T. ) ;
#14262 = VERTEX_POINT ( 'NONE', #20965 ) ;
#14263 = FACE_OUTER_BOUND ( 'NONE', #31143, .T. ) ;
#14264 = CIRCLE ( 'NONE', #16584, 52.00000000000000711 ) ;
#14265 =( REPRESENTATION_RELATIONSHIP ('NONE','NONE', #26607, #2005 ) REPRESENTATION_RELATIONSHIP_WITH_TRANSFORMATION ( #31032 )SHAPE_REPRESENTATION_RELATIONSHIP( ) );
#14266 = CARTESIAN_POINT ( 'NONE',  ( -35.50000000000000000, -113.9929510916434339, 10.51175824272318415 ) ) ;
#14267 = DIRECTION ( 'NONE',  ( 0.000000000000000000, 0.5000000000000031086, -0.8660254037844368202 ) ) ;
#14268 = DIRECTION ( 'NONE',  ( -0.000000000000000000, 0.000000000000000000, -1.000000000000000000 ) ) ;
#14269 = VECTOR ( 'NONE', #29504, 1000.000000000000000 ) ;
#14270 = CARTESIAN_POINT ( 'NONE',  ( -34.50000000000000000, -112.1946304249441795, 2.703640693953100804 ) ) ;
#14271 = EDGE_CURVE ( 'NONE', #8923, #32022, #7820, .T. ) ;
#14272 = CARTESIAN_POINT ( 'NONE',  ( -35.50000000000000000, -114.4680894751352156, 8.562575367713533225 ) ) ;
#14273 = DIRECTION ( 'NONE',  ( 0.000000000000000000, 0.000000000000000000, 1.000000000000000000 ) ) ;
#14274 = CARTESIAN_POINT ( 'NONE',  ( 8.000000000000000000, 0.000000000000000000, 0.000000000000000000 ) ) ;
#14275 = CARTESIAN_POINT ( 'NONE',  ( 8.000000000000000000, -21.63912866391141065, 3.968388925834729797 ) ) ;
#14276 = CARTESIAN_POINT ( 'NONE',  ( 50.00000000000000000, 10.00000000000000888, -25.00000000000000000 ) ) ;
#14277 = CARTESIAN_POINT ( 'NONE',  ( -9.999999999999994671, 0.000000000000000000, 0.000000000000000000 ) ) ;
#14278 = ORIENTED_EDGE ( 'NONE', *, *, #15678, .F. ) ;
#14279 = DIRECTION ( 'NONE',  ( -1.000000000000000000, 0.000000000000000000, 0.000000000000000000 ) ) ;
#14280 = DIRECTION ( 'NONE',  ( -1.000000000000000000, -0.000000000000000000, -0.000000000000000000 ) ) ;
#14281 = EDGE_CURVE ( 'NONE', #9203, #25659, #28915, .T. ) ;
#14282 = PLANE ( 'NONE',  #34359 ) ;
#14283 = CARTESIAN_POINT ( 'NONE',  ( 46.00000000000000000, 9.797174393178825657E-16, 8.000000000000000000 ) ) ;
#14284 = EDGE_CURVE ( 'NONE', #7515, #9483, #27954, .T. ) ;
#14285 = AXIS2_PLACEMENT_3D ( 'NONE', #13790, #35592, #21343 ) ;
#14286 = AXIS2_PLACEMENT_3D ( 'NONE', #23124, #31412, #4743 ) ;
#14287 = CARTESIAN_POINT ( 'NONE',  ( -49.99999999999998579, -64.99999999999997158, 120.0000000000000000 ) ) ;
#14288 = CARTESIAN_POINT ( 'NONE',  ( -1.799999999999996048, -5.551115123125792563E-16, -8.000000000000051514 ) ) ;
#14289 = ORIENTED_EDGE ( 'NONE', *, *, #20938, .T. ) ;
#14290 = CIRCLE ( 'NONE', #16009, 10.99999999999999645 ) ;
#14291 = CARTESIAN_POINT ( 'NONE',  ( 8.000000000000000000, 3.872983346207417021, -1.000000000000000000 ) ) ;
#14292 = DIRECTION ( 'NONE',  ( -1.000000000000000000, -0.000000000000000000, -0.000000000000000000 ) ) ;
#14293 = DIRECTION ( 'NONE',  ( 0.000000000000000000, -0.2486898871648415832, -0.9685831611286344067 ) ) ;
#14294 = EDGE_LOOP ( 'NONE', ( #25915, #2638, #22160, #25773 ) ) ;
#14295 = CARTESIAN_POINT ( 'NONE',  ( -35.97545270896705460, -114.3549511594417680, 5.590225545821552622 ) ) ;
#14296 = EDGE_CURVE ( 'NONE', #28885, #5282, #15037, .T. ) ;
#14297 = ORIENTED_EDGE ( 'NONE', *, *, #14271, .F. ) ;
#14298 = EDGE_CURVE ( 'NONE', #30312, #19686, #1372, .T. ) ;
#14299 =( NAMED_UNIT ( * ) PLANE_ANGLE_UNIT ( ) SI_UNIT ( $, .RADIAN. ) );
#14300 = ORIENTED_EDGE ( 'NONE', *, *, #33892, .T. ) ;
#14301 = ORIENTED_EDGE ( 'NONE', *, *, #6614, .T. ) ;
#14302 = CYLINDRICAL_SURFACE ( 'NONE', #16027, 4.000000000000000000 ) ;
#14303 = CARTESIAN_POINT ( 'NONE',  ( -35.50000000000000711, -116.0140978167138712, -0.4997823525984418369 ) ) ;
#14304 = DIRECTION ( 'NONE',  ( 0.000000000000000000, 0.000000000000000000, -1.000000000000000000 ) ) ;
#14305 = CARTESIAN_POINT ( 'NONE',  ( -35.50000000000000711, -114.8211182053456838, 9.932864235516914775 ) ) ;
#14306 = CARTESIAN_POINT ( 'NONE',  ( 0.000000000000000000, 9.714451465470119729E-14, 1.000000000000000888 ) ) ;
#14307 = CARTESIAN_POINT ( 'NONE',  ( 0.1374368770859502042, -4.808326913196061980, 0.000000000000000000 ) ) ;
#14308 = EDGE_CURVE ( 'NONE', #30393, #23989, #4401, .T. ) ;
#14309 = CARTESIAN_POINT ( 'NONE',  ( -34.50000000000000000, -114.9929510916434339, 12.39849696637031506 ) ) ;
#14310 = CARTESIAN_POINT ( 'NONE',  ( 7.999999999999992895, -39.55064067543080597, 25.36340625197344778 ) ) ;
#14311 = AXIS2_PLACEMENT_3D ( 'NONE', #17493, #11928, #6345 ) ;
#14312 = FACE_OUTER_BOUND ( 'NONE', #25297, .T. ) ;
#14313 = CARTESIAN_POINT ( 'NONE',  ( -39.00000000000000000, -115.9929510916434481, 11.21034663311206181 ) ) ;
#14314 = CARTESIAN_POINT ( 'NONE',  ( -35.50000000000000711, -112.1403507321855528, -1.128496220798856253 ) ) ;
#14315 = CARTESIAN_POINT ( 'NONE',  ( -0.1085714285714300953, -3.798448662927791819, -0.7999999999999951594 ) ) ;
#14316 = CARTESIAN_POINT ( 'NONE',  ( 0.000000000000000000, 40.47821179127763003, -32.64221760512714354 ) ) ;
#14317 = DIRECTION ( 'NONE',  ( 0.000000000000000000, 0.000000000000000000, 1.000000000000000000 ) ) ;
#14318 = FACE_OUTER_BOUND ( 'NONE', #35311, .T. ) ;
#14319 = EDGE_CURVE ( 'NONE', #6685, #26059, #12429, .T. ) ;
#14320 = CARTESIAN_POINT ( 'NONE',  ( 7.999999999999992895, 0.2227391519116599106, 46.98410307550729215 ) ) ;
#14321 = CYLINDRICAL_SURFACE ( 'NONE', #16654, 10.99999999999999645 ) ;
#14322 = ORIENTED_EDGE ( 'NONE', *, *, #13290, .F. ) ;
#14323 = EDGE_CURVE ( 'NONE', #10821, #4637, #15941, .T. ) ;
#14324 = EDGE_CURVE ( 'NONE', #13189, #20288, #23509, .T. ) ;
#14325 = CARTESIAN_POINT ( 'NONE',  ( -37.47347596530441649, -113.0245472910329880, 3.527725545821551734 ) ) ;
#14326 = CARTESIAN_POINT ( 'NONE',  ( 7.999999999999992895, -46.19362259308826424, -8.585149169758999221 ) ) ;
#14327 = CARTESIAN_POINT ( 'NONE',  ( -39.49999999999999289, 9.432411113711806294, 117.4309090467819772 ) ) ;
#14328 = DIRECTION ( 'NONE',  ( 0.000000000000000000, 0.000000000000000000, 1.000000000000000000 ) ) ;
#14329 = VERTEX_POINT ( 'NONE', #24064 ) ;
#14330 = ORIENTED_EDGE ( 'NONE', *, *, #17735, .T. ) ;
#14331 = CARTESIAN_POINT ( 'NONE',  ( 7.999999999999992895, -22.82995208772716467, 41.06517797613655318 ) ) ;
#14332 = CARTESIAN_POINT ( 'NONE',  ( 7.999999999999992895, 0.000000000000000000, 0.000000000000000000 ) ) ;
#14333 = ORIENTED_EDGE ( 'NONE', *, *, #21512, .T. ) ;
#14334 = VERTEX_POINT ( 'NONE', #7645 ) ;
#14335 = ADVANCED_FACE ( 'NONE', ( #32862 ), #18457, .F. ) ;
#14336 = AXIS2_PLACEMENT_3D ( 'NONE', #15627, #16163, #18697 ) ;
#14337 = DIRECTION ( 'NONE',  ( 0.000000000000000000, 0.000000000000000000, 1.000000000000000000 ) ) ;
#14338 = CARTESIAN_POINT ( 'NONE',  ( 4.000000000000003553, -47.32430374665916872, -21.55018039121578255 ) ) ;
#14339 = VECTOR ( 'NONE', #29934, 1000.000000000000114 ) ;
#14340 = AXIS2_PLACEMENT_3D ( 'NONE', #12953, #10607, #5036 ) ;
#14341 = EDGE_CURVE ( 'NONE', #21809, #1825, #29633, .T. ) ;
#14342 = APPLICATION_PROTOCOL_DEFINITION ( 'draft international standard', 'automotive_design', 1998, #12385 ) ;
#14343 = DIRECTION ( 'NONE',  ( 0.000000000000000000, 0.000000000000000000, 1.000000000000000000 ) ) ;
#14344 = ORIENTED_EDGE ( 'NONE', *, *, #14688, .F. ) ;
#14345 = ORIENTED_EDGE ( 'NONE', *, *, #19007, .T. ) ;
#14346 = DIRECTION ( 'NONE',  ( -1.000000000000000000, 0.000000000000000000, 0.000000000000000000 ) ) ;
#14347 = CARTESIAN_POINT ( 'NONE',  ( -10.00000000000000178, 0.000000000000000000, 0.000000000000000000 ) ) ;
#14348 = ORIENTED_EDGE ( 'NONE', *, *, #6558, .T. ) ;
#14349 = FACE_OUTER_BOUND ( 'NONE', #19283, .T. ) ;
#14350 = ADVANCED_FACE ( 'NONE', ( #10187 ), #27287, .T. ) ;
#14351 = CARTESIAN_POINT ( 'NONE',  ( -34.50000000000000000, -115.0140978167138712, -0.5622823525984408377 ) ) ;
#14352 = CARTESIAN_POINT ( 'NONE',  ( -42.49999999999999289, -13.17619866229204284, 90.66066734786082293 ) ) ;
#14353 = CYLINDRICAL_SURFACE ( 'NONE', #2373, 52.00000000000000711 ) ;
#14354 = CARTESIAN_POINT ( 'NONE',  ( -34.50000000000000000, -114.8124184834118324, 8.677834500183694288 ) ) ;
#14355 = EDGE_CURVE ( 'NONE', #12939, #34112, #11358, .T. ) ;
#14356 = FACE_BOUND ( 'NONE', #14699, .T. ) ;
#14357 = CARTESIAN_POINT ( 'NONE',  ( 70.00000000000001421, -31.33892132276156062, 83.40622150580404082 ) ) ;
#14358 = CARTESIAN_POINT ( 'NONE',  ( -34.50000000000000000, -114.2356323198232673, 8.521029492159460261 ) ) ;
#14359 = DIRECTION ( 'NONE',  ( 0.000000000000000000, -1.000000000000000000, 0.000000000000000000 ) ) ;
#14360 = CARTESIAN_POINT ( 'NONE',  ( -34.50000000000000000, -114.0000000000003411, 9.500000000000035527 ) ) ;
#14361 = AXIS2_PLACEMENT_3D ( 'NONE', #27191, #31293, #33625 ) ;
#14362 = DIRECTION ( 'NONE',  ( 1.000000000000000000, 0.000000000000000000, 0.000000000000000000 ) ) ;
#14363 = CYLINDRICAL_SURFACE ( 'NONE', #31310, 9.999999999999994671 ) ;
#14364 = EDGE_LOOP ( 'NONE', ( #22970, #5811, #21389, #4406 ) ) ;
#14365 = DIRECTION ( 'NONE',  ( -1.000000000000000000, -1.817026393327835042E-30, 1.734723475976807094E-16 ) ) ;
#14366 = ORIENTED_EDGE ( 'NONE', *, *, #9462, .T. ) ;
#14367 = EDGE_CURVE ( 'NONE', #30594, #5465, #1918, .T. ) ;
#14368 = AXIS2_PLACEMENT_3D ( 'NONE', #21725, #27849, #2669 ) ;
#14369 = CARTESIAN_POINT ( 'NONE',  ( -34.57658136524562309, -114.9929510916434339, 13.10177712753338497 ) ) ;
#14370 = CARTESIAN_POINT ( 'NONE',  ( -36.94073759706866156, -111.0000000000000284, 5.628524454178450043 ) ) ;
#14371 = EDGE_CURVE ( 'NONE', #14262, #27701, #15286, .T. ) ;
#14372 = CARTESIAN_POINT ( 'NONE',  ( -4.000000000000000000, 0.000000000000000000, -49.10000000000000142 ) ) ;
#14373 = CARTESIAN_POINT ( 'NONE',  ( -35.50000000000000711, -112.5103839485166333, -1.498529437127682495 ) ) ;
#14374 = EDGE_LOOP ( 'NONE', ( #3252, #6563, #1700, #16772 ) ) ;
#14375 = ORIENTED_EDGE ( 'NONE', *, *, #24318, .F. ) ;
#14377 = DIRECTION ( 'NONE',  ( -1.000000000000000000, 0.000000000000000000, 0.000000000000000000 ) ) ;
#14376 = PRODUCT_DEFINITION_SHAPE ( 'NONE', 'NONE',  #18964 ) ;
#14378 = CARTESIAN_POINT ( 'NONE',  ( 3.799999999999999822, -2.710505431213761085E-17, -21.89999999999999858 ) ) ;
#14379 = EDGE_LOOP ( 'NONE', ( #16602, #31646, #15094, #5149 ) ) ;
#14380 = CARTESIAN_POINT ( 'NONE',  ( -44.00000000000000000, 0.000000000000000000, 0.000000000000000000 ) ) ;
#14381 = EDGE_LOOP ( 'NONE', ( #17117, #32606, #7444, #21515 ) ) ;
#14382 = ORIENTED_EDGE ( 'NONE', *, *, #13922, .T. ) ;
#14383 = DIRECTION ( 'NONE',  ( 0.000000000000000000, 0.000000000000000000, 1.000000000000000000 ) ) ;
#14384 = AXIS2_PLACEMENT_3D ( 'NONE', #21479, #29966, #30138 ) ;
#14385 = DIRECTION ( 'NONE',  ( -1.000000000000000000, 0.000000000000000000, 0.000000000000000000 ) ) ;
#14386 = EDGE_LOOP ( 'NONE', ( #20519, #21427, #19803, #34472 ) ) ;
#14387 = ORIENTED_EDGE ( 'NONE', *, *, #1805, .F. ) ;
#14388 = CIRCLE ( 'NONE', #16110, 4.000000000000000000 ) ;
#14389 = CARTESIAN_POINT ( 'NONE',  ( -34.50000000000000000, -116.9501796819249222, -1.143161139954000260 ) ) ;
#14390 = DIRECTION ( 'NONE',  ( 0.000000000000000000, 0.000000000000000000, 1.000000000000000000 ) ) ;
#14391 = CIRCLE ( 'NONE', #2917, 4.000000000000000000 ) ;
#14392 = VERTEX_POINT ( 'NONE', #12893 ) ;
#14393 = CIRCLE ( 'NONE', #14420, 0.2000000000000000944 ) ;
#14394 = CARTESIAN_POINT ( 'NONE',  ( -37.34375000000001421, -114.9929510916434339, 13.11852480586264669 ) ) ;
#14395 = EDGE_CURVE ( 'NONE', #16096, #12193, #5047, .T. ) ;
#14396 = EDGE_CURVE ( 'NONE', #20157, #4114, #13031, .T. ) ;
#14397 = CARTESIAN_POINT ( 'NONE',  ( -34.50000000000000000, -114.0650276068786582, 9.507762098804159123 ) ) ;
#14398 = LINE ( 'NONE', #11701, #3908 ) ;
#14399 = CARTESIAN_POINT ( 'NONE',  ( -90.00000000000002842, 7.674144758152321929E-16, 4.000000000000021316 ) ) ;
#14400 = CARTESIAN_POINT ( 'NONE',  ( -34.50000000000000000, -113.9929510916434339, 10.53376102667243508 ) ) ;
#14401 = CARTESIAN_POINT ( 'NONE',  ( 0.000000000000000000, 20.99948489194482448, -42.60488980472762677 ) ) ;
#14402 = CARTESIAN_POINT ( 'NONE',  ( -35.50000000000000711, -114.9929510916434339, 12.56351784598954424 ) ) ;
#14403 = SURFACE_SIDE_STYLE ('',( #28282 ) ) ;
#14404 = FACE_OUTER_BOUND ( 'NONE', #32294, .T. ) ;
#14405 = PLANE ( 'NONE',  #14588 ) ;
#14406 = ORIENTED_EDGE ( 'NONE', *, *, #13452, .T. ) ;
#14407 = ORIENTED_EDGE ( 'NONE', *, *, #35480, .T. ) ;
#14408 = VECTOR ( 'NONE', #8770, 1000.000000000000114 ) ;
#14409 = DIRECTION ( 'NONE',  ( -1.000000000000000000, 0.000000000000000000, 0.000000000000000000 ) ) ;
#14410 = DIRECTION ( 'NONE',  ( 0.000000000000000000, 0.000000000000000000, -1.000000000000000000 ) ) ;
#14411 = ORIENTED_EDGE ( 'NONE', *, *, #33687, .F. ) ;
#14412 = CARTESIAN_POINT ( 'NONE',  ( 0.000000000000000000, -2.710505431213761085E-17, 55.00000000000000000 ) ) ;
#14413 = VERTEX_POINT ( 'NONE', #18815 ) ;
#14414 = CARTESIAN_POINT ( 'NONE',  ( -35.50000000000000000, -113.0140978167138712, -0.6247823525988807081 ) ) ;
#14415 = DIRECTION ( 'NONE',  ( 0.02857142857142376188, 0.9995917534020517525, 3.884870526907702485E-16 ) ) ;
#14416 = CARTESIAN_POINT ( 'NONE',  ( -35.62769128460905677, -115.4561184093552413, 6.191024454178448266 ) ) ;
#14417 = EDGE_CURVE ( 'NONE', #28739, #33531, #8412, .T. ) ;
#14418 = CIRCLE ( 'NONE', #6953, 4.200000000000014388 ) ;
#14419 = EDGE_LOOP ( 'NONE', ( #941, #19939, #4720, #33046 ) ) ;
#14420 = AXIS2_PLACEMENT_3D ( 'NONE', #10832, #21602, #26864 ) ;
#14421 = CARTESIAN_POINT ( 'NONE',  ( -36.94073759706868287, -112.0000000000000142, 7.128524454178449155 ) ) ;
#14422 = ORIENTED_EDGE ( 'NONE', *, *, #19082, .T. ) ;
#14423 = DIRECTION ( 'NONE',  ( -1.000000000000000000, -1.836970198721029934E-16, -0.000000000000000000 ) ) ;
#14424 = CARTESIAN_POINT ( 'NONE',  ( -35.50000000000000000, -116.9980674558286040, -0.8858242144478970514 ) ) ;
#14425 = VERTEX_POINT ( 'NONE', #16094 ) ;
#14426 = ORIENTED_EDGE ( 'NONE', *, *, #25832, .F. ) ;
#14427 = CARTESIAN_POINT ( 'NONE',  ( -38.99999999999999289, -113.9407375970686900, 6.753524454178448266 ) ) ;
#14428 = DIRECTION ( 'NONE',  ( 0.000000000000000000, 0.000000000000000000, -1.000000000000000000 ) ) ;
#14429 = ORIENTED_EDGE ( 'NONE', *, *, #29628, .T. ) ;
#14430 = ORIENTED_EDGE ( 'NONE', *, *, #9857, .T. ) ;
#14431 = CARTESIAN_POINT ( 'NONE',  ( -34.50000000000000000, -112.8655373925166572, 1.864575885149403423 ) ) ;
#14432 = DIRECTION ( 'NONE',  ( 0.000000000000000000, 0.6427876096865403621, -0.7660444431189772363 ) ) ;
#14433 = ORIENTED_EDGE ( 'NONE', *, *, #4845, .T. ) ;
#14434 = ORIENTED_EDGE ( 'NONE', *, *, #20003, .F. ) ;
#14435 = CARTESIAN_POINT ( 'NONE',  ( 7.999999999999992895, 0.000000000000000000, 0.000000000000000000 ) ) ;
#14436 = ADVANCED_FACE ( 'NONE', ( #18993 ), #26759, .T. ) ;
#14437 = CARTESIAN_POINT ( 'NONE',  ( -36.87500000000098765, -113.9929510916434339, 13.11852480586264846 ) ) ;
#14438 = DIRECTION ( 'NONE',  ( 0.000000000000000000, 0.000000000000000000, 1.000000000000000000 ) ) ;
#14439 = DIRECTION ( 'NONE',  ( -1.000000000000000000, -0.000000000000000000, -0.000000000000000000 ) ) ;
#14440 = AXIS2_PLACEMENT_3D ( 'NONE', #18190, #29201, #1829 ) ;
#14441 = CIRCLE ( 'NONE', #28832, 20.00000000000000711 ) ;
#14442 = CARTESIAN_POINT ( 'NONE',  ( -34.50000000000000000, -111.0140821919084715, 0.8283428459075261596 ) ) ;
#14443 = CARTESIAN_POINT ( 'NONE',  ( -38.92341863475394348, -115.9929510916434481, 13.10177712753322155 ) ) ;
#14444 = CARTESIAN_POINT ( 'NONE',  ( 7.999999999999992895, -36.34385289850609979, 29.77717097092063980 ) ) ;
#14445 = DIRECTION ( 'NONE',  ( 1.000000000000000000, 0.000000000000000000, 0.000000000000000000 ) ) ;
#14446 = ADVANCED_FACE ( 'NONE', ( #8182 ), #15561, .T. ) ;
#14447 = DIRECTION ( 'NONE',  ( -1.000000000000000000, -0.000000000000000000, -0.000000000000000000 ) ) ;
#14448 = DIRECTION ( 'NONE',  ( 1.000000000000000000, 1.734723475976807094E-16, 0.000000000000000000 ) ) ;
#14449 = DIRECTION ( 'NONE',  ( -1.000000000000000000, 0.000000000000000000, 0.000000000000000000 ) ) ;
#14450 = EDGE_LOOP ( 'NONE', ( #33596, #9165, #20244, #16419 ) ) ;
#14451 = LINE ( 'NONE', #14103, #34114 ) ;
#14452 = DIRECTION ( 'NONE',  ( -1.000000000000000000, 0.000000000000000000, 0.000000000000000000 ) ) ;
#14453 = CYLINDRICAL_SURFACE ( 'NONE', #20533, 8.000000000000003553 ) ;
#14454 = LINE ( 'NONE', #3505, #29356 ) ;
#14455 = DIRECTION ( 'NONE',  ( -1.000000000000000000, 0.000000000000000000, 0.000000000000000000 ) ) ;
#14456 = CARTESIAN_POINT ( 'NONE',  ( 4.000000000000003553, -44.25018368420762016, 27.31155879685168131 ) ) ;
#14457 = VERTEX_POINT ( 'NONE', #26944 ) ;
#14458 =( NAMED_UNIT ( * ) SI_UNIT ( $, .STERADIAN. ) SOLID_ANGLE_UNIT ( ) );
#14459 = DIRECTION ( 'NONE',  ( -1.000000000000000000, 0.000000000000000000, 0.000000000000000000 ) ) ;
#14460 = FACE_OUTER_BOUND ( 'NONE', #32636, .T. ) ;
#14461 = ORIENTED_EDGE ( 'NONE', *, *, #8030, .F. ) ;
#14462 = VERTEX_POINT ( 'NONE', #21497 ) ;
#14463 = CARTESIAN_POINT ( 'NONE',  ( -36.02454729103297382, -113.5265240346956261, 6.902725545821551734 ) ) ;
#14464 = ORIENTED_EDGE ( 'NONE', *, *, #22086, .T. ) ;
#14465 = CIRCLE ( 'NONE', #28289, 47.49900000000002365 ) ;
#14466 = STYLED_ITEM ( 'NONE', ( #12278 ), #30145 ) ;
#14467 = CIRCLE ( 'NONE', #34619, 3.799999999999999822 ) ;
#14468 =( LENGTH_UNIT ( ) NAMED_UNIT ( * ) SI_UNIT ( .MILLI., .METRE. ) );
#14469 = ORIENTED_EDGE ( 'NONE', *, *, #28860, .T. ) ;
#14470 = VERTEX_POINT ( 'NONE', #2454 ) ;
#14471 = CYLINDRICAL_SURFACE ( 'NONE', #7974, 13.99999999999999822 ) ;
#14472 = CARTESIAN_POINT ( 'NONE',  ( -35.50000000000000711, -114.5974311500472425, -1.624782352598427959 ) ) ;
#14473 = LINE ( 'NONE', #22758, #697 ) ;
#14474 = EDGE_CURVE ( 'NONE', #17673, #19029, #11855, .T. ) ;
#14475 = DIRECTION ( 'NONE',  ( -1.000000000000000000, 0.000000000000000000, 0.000000000000000000 ) ) ;
#14476 = DIRECTION ( 'NONE',  ( -1.000000000000000000, 0.000000000000000000, -0.000000000000000000 ) ) ;
#14477 = EDGE_CURVE ( 'NONE', #12175, #7742, #27980, .T. ) ;
#14478 = DIRECTION ( 'NONE',  ( 1.084202172485497655E-16, -6.938893903907204958E-17, -1.000000000000000000 ) ) ;
#14479 = CARTESIAN_POINT ( 'NONE',  ( -34.50000000000000000, -114.1021862393805577, 9.512197583835053649 ) ) ;
#14480 = CYLINDRICAL_SURFACE ( 'NONE', #21993, 4.000000000000000000 ) ;
#14481 = CIRCLE ( 'NONE', #136, 47.49900000000000944 ) ;
#14482 = CYLINDRICAL_SURFACE ( 'NONE', #32990, 3.799999999999999822 ) ;
#14483 = EDGE_CURVE ( 'NONE', #9277, #24314, #10718, .T. ) ;
#14484 = CARTESIAN_POINT ( 'NONE',  ( -35.50000000000000000, -115.9929510916434481, 11.21034663311132107 ) ) ;
#14485 = CARTESIAN_POINT ( 'NONE',  ( -35.50000000000000711, -113.0796441757086939, 1.890140615870383956 ) ) ;
#14486 = CYLINDRICAL_SURFACE ( 'NONE', #30666, 5.000000000000004441 ) ;
#14487 = DIRECTION ( 'NONE',  ( -0.000000000000000000, -0.2538061376417690140, -0.9672551082808337197 ) ) ;
#14488 = DIRECTION ( 'NONE',  ( -1.000000000000000000, 0.000000000000000000, 0.000000000000000000 ) ) ;
#14489 = FACE_OUTER_BOUND ( 'NONE', #8676, .T. ) ;
#14490 = CARTESIAN_POINT ( 'NONE',  ( 5.400000000000015454, -1.000000000000002220, 38.00000000000000000 ) ) ;
#14491 = LINE ( 'NONE', #25503, #576 ) ;
#14492 = ORIENTED_EDGE ( 'NONE', *, *, #10627, .T. ) ;
#14493 = CARTESIAN_POINT ( 'NONE',  ( -36.64504884055821776, -112.9754527089670688, 8.215225545821551734 ) ) ;
#14494 = CARTESIAN_POINT ( 'NONE',  ( 0.000000000000000000, 11.27190672109280811, 4.484851126495202678 ) ) ;
#14495 = DIRECTION ( 'NONE',  ( -1.000000000000000000, 0.000000000000000000, 0.000000000000000000 ) ) ;
#14496 = ORIENTED_EDGE ( 'NONE', *, *, #18323, .F. ) ;
#14497 = VECTOR ( 'NONE', #21142, 1000.000000000000000 ) ;
#14498 = ORIENTED_EDGE ( 'NONE', *, *, #11007, .F. ) ;
#14499 = CARTESIAN_POINT ( 'NONE',  ( 50.00000000000000000, -25.98076211353320275, 76.99999999999992895 ) ) ;
#14500 = FACE_OUTER_BOUND ( 'NONE', #5209, .T. ) ;
#14501 = VERTEX_POINT ( 'NONE', #29281 ) ;
#14502 = CARTESIAN_POINT ( 'NONE',  ( -38.18337828418796676, -117.0245472910329738, 4.465225545821550845 ) ) ;
#14503 = ORIENTED_EDGE ( 'NONE', *, *, #33522, .T. ) ;
#14504 = EDGE_CURVE ( 'NONE', #27575, #3028, #10740, .T. ) ;
#14505 = DIRECTION ( 'NONE',  ( -1.000000000000000000, -1.836970198721029934E-16, -0.000000000000000000 ) ) ;
#14506 = AXIS2_PLACEMENT_3D ( 'NONE', #30620, #17273, #28278 ) ;
#14507 = CARTESIAN_POINT ( 'NONE',  ( -55.00000000000000000, 0.000000000000000000, -5.000000000000011546 ) ) ;
#14508 = PRODUCT_CONTEXT ( 'NONE', #9172, 'mechanical' ) ;
#14509 = CARTESIAN_POINT ( 'NONE',  ( 7.999999999999992895, 11.90021268425617329, -45.45261810511203038 ) ) ;
#14510 = ORIENTED_EDGE ( 'NONE', *, *, #597, .T. ) ;
#14511 = ORIENTED_EDGE ( 'NONE', *, *, #197, .T. ) ;
#14512 = EDGE_CURVE ( 'NONE', #24505, #25823, #21869, .T. ) ;
#14513 = CYLINDRICAL_SURFACE ( 'NONE', #22592, 4.800000000000000711 ) ;
#14514 = EDGE_CURVE ( 'NONE', #22481, #8656, #30515, .T. ) ;
#14515 = EDGE_CURVE ( 'NONE', #4091, #33531, #2715, .T. ) ;
#14516 = VERTEX_POINT ( 'NONE', #14110 ) ;
#14517 = DIRECTION ( 'NONE',  ( -1.000000000000000000, -0.000000000000000000, -0.000000000000000000 ) ) ;
#14518 = CARTESIAN_POINT ( 'NONE',  ( -34.50000000000000000, -114.8057644833805853, -0.6247823525984269599 ) ) ;
#14519 = CARTESIAN_POINT ( 'NONE',  ( 8.000000000000007105, -11.27190672109260028, 4.484851126495120077 ) ) ;
#14520 = CARTESIAN_POINT ( 'NONE',  ( -34.50000000000000000, -116.0140978167138712, 0.6252176474015648244 ) ) ;
#14521 = CARTESIAN_POINT ( 'NONE',  ( -34.50000000000000000, -114.4680894751352156, 8.562575367713533225 ) ) ;
#14522 = VECTOR ( 'NONE', #15953, 1000.000000000000000 ) ;
#14523 = DIRECTION ( 'NONE',  ( -1.000000000000000000, 0.000000000000000000, 0.000000000000000000 ) ) ;
#14524 = CARTESIAN_POINT ( 'NONE',  ( 0.000000000000000000, -2.710505431213761085E-17, 38.00000000000000711 ) ) ;
#14525 = EDGE_CURVE ( 'NONE', #4771, #4637, #6020, .T. ) ;
#14526 = CARTESIAN_POINT ( 'NONE',  ( -38.42182118622945808, -114.9929510916434339, 13.81802396319329773 ) ) ;
#14527 = DIRECTION ( 'NONE',  ( -1.000000000000000000, 0.000000000000000000, 0.000000000000000000 ) ) ;
#14528 = ADVANCED_FACE ( 'NONE', ( #30162 ), #89, .F. ) ;
#14529 = LINE ( 'NONE', #28416, #23609 ) ;
#14530 = LINE ( 'NONE', #17589, #30256 ) ;
#14531 = CARTESIAN_POINT ( 'NONE',  ( 0.000000000000000000, -46.77034588191288833, -22.72740077717277885 ) ) ;
#14532 = VECTOR ( 'NONE', #28823, 1000.000000000000000 ) ;
#14533 = ORIENTED_EDGE ( 'NONE', *, *, #31900, .F. ) ;
#14534 = AXIS2_PLACEMENT_3D ( 'NONE', #13324, #21403, #26656 ) ;
#14535 = FACE_OUTER_BOUND ( 'NONE', #23524, .T. ) ;
#14536 = EDGE_LOOP ( 'NONE', ( #12760, #12096, #11815, #13178 ) ) ;
#14537 = CARTESIAN_POINT ( 'NONE',  ( -34.00000000000000000, -113.9407375970686758, 6.996475545821551734 ) ) ;
#14538 = FACE_OUTER_BOUND ( 'NONE', #18536, .T. ) ;
#14539 = CARTESIAN_POINT ( 'NONE',  ( -35.50000000000000711, -115.3362660311619692, -1.573728109101206085 ) ) ;
#14540 = EDGE_LOOP ( 'NONE', ( #14786, #3501, #34504, #14797 ) ) ;
#14541 = ORIENTED_EDGE ( 'NONE', *, *, #15624, .F. ) ;
#14542 = DIRECTION ( 'NONE',  ( -1.000000000000000000, 0.000000000000000000, 0.000000000000000000 ) ) ;
#14543 = PLANE ( 'NONE',  #27263 ) ;
#14544 = VERTEX_POINT ( 'NONE', #438 ) ;
#14545 = EDGE_LOOP ( 'NONE', ( #7754, #22803, #9432, #6454 ) ) ;
#14546 = ADVANCED_FACE ( 'NONE', ( #3508 ), #5500, .F. ) ;
#14547 = AXIS2_PLACEMENT_3D ( 'NONE', #17397, #8943, #22279 ) ;
#14548 = DIRECTION ( 'NONE',  ( 0.000000000000000000, 0.000000000000000000, 1.000000000000000000 ) ) ;
#14549 = ORIENTED_EDGE ( 'NONE', *, *, #4071, .T. ) ;
#14551 = ORIENTED_EDGE ( 'NONE', *, *, #15496, .F. ) ;
#14550 = EDGE_CURVE ( 'NONE', #24079, #22597, #16810, .T. ) ;
#14552 = CARTESIAN_POINT ( 'NONE',  ( -34.97545270896703329, -114.7691647218148745, 7.090225545821551734 ) ) ;
#14553 = EDGE_CURVE ( 'NONE', #32501, #35307, #19512, .T. ) ;
#14554 = DIRECTION ( 'NONE',  ( 0.000000000000000000, -1.000000000000000000, 0.000000000000000000 ) ) ;
#14555 = VERTEX_POINT ( 'NONE', #27818 ) ;
#14556 = ORIENTED_EDGE ( 'NONE', *, *, #32854, .F. ) ;
#14557 = CARTESIAN_POINT ( 'NONE',  ( -35.50000000000000000, -111.0140978167138570, -0.4685323525984296800 ) ) ;
#14558 = AXIS2_PLACEMENT_3D ( 'NONE', #18721, #30076, #5417 ) ;
#14559 = AXIS2_PLACEMENT_3D ( 'NONE', #13802, #11272, #24790 ) ;
#14560 = EDGE_CURVE ( 'NONE', #11959, #27071, #35471, .T. ) ;
#14561 = CIRCLE ( 'NONE', #17446, 7.199999999999994849 ) ;
#14562 = FACE_OUTER_BOUND ( 'NONE', #21463, .T. ) ;
#14563 = VERTEX_POINT ( 'NONE', #3154 ) ;
#14564 = ADVANCED_FACE ( 'NONE', ( #33738 ), #33216, .T. ) ;
#14565 = CARTESIAN_POINT ( 'NONE',  ( -37.18750000000006395, -114.9929510916434339, 13.11852480586264669 ) ) ;
#14566 = CARTESIAN_POINT ( 'NONE',  ( -37.48437500000004263, -113.9929510916434339, 14.11852480586265024 ) ) ;
#14567 = DIRECTION ( 'NONE',  ( 0.000000000000000000, -1.000000000000000000, 0.000000000000000000 ) ) ;
#14568 = CARTESIAN_POINT ( 'NONE',  ( 7.999999999999992895, 22.82995208772746665, -41.06517797613640397 ) ) ;
#14569 = CARTESIAN_POINT ( 'NONE',  ( -36.50000000000010658, -113.9929510916434339, 14.11852480586265024 ) ) ;
#14570 = DIRECTION ( 'NONE',  ( -1.000000000000000000, 0.000000000000000000, 0.000000000000000000 ) ) ;
#14571 = EDGE_CURVE ( 'NONE', #1603, #3820, #30692, .T. ) ;
#14572 = CARTESIAN_POINT ( 'NONE',  ( -35.87040530316090070, -114.9929510916434339, 13.10254527216545917 ) ) ;
#14573 = FACE_OUTER_BOUND ( 'NONE', #19757, .T. ) ;
#14574 = CIRCLE ( 'NONE', #19730, 1.000000000000000888 ) ;
#14575 = ORIENTED_EDGE ( 'NONE', *, *, #11906, .T. ) ;
#14576 = CIRCLE ( 'NONE', #12866, 3.799999999999999822 ) ;
#14577 = CYLINDRICAL_SURFACE ( 'NONE', #24472, 8.000000000000000000 ) ;
#14578 = CARTESIAN_POINT ( 'NONE',  ( 23.00000000000000711, 4.000000000000005329, 4.898587196589404940E-16 ) ) ;
#14579 = VERTEX_POINT ( 'NONE', #16979 ) ;
#14580 = CARTESIAN_POINT ( 'NONE',  ( -35.50000000000000711, -114.9929510916434339, 12.26648026267477221 ) ) ;
#14581 = ORIENTED_EDGE ( 'NONE', *, *, #34139, .T. ) ;
#14582 = CYLINDRICAL_SURFACE ( 'NONE', #27587, 19.99999999999998579 ) ;
#14583 = CARTESIAN_POINT ( 'NONE',  ( 8.000000000000000000, 0.000000000000000000, 0.000000000000000000 ) ) ;
#14584 = EDGE_LOOP ( 'NONE', ( #5543, #7087, #35434, #16645 ) ) ;
#14585 = FACE_OUTER_BOUND ( 'NONE', #9427, .T. ) ;
#14586 = ORIENTED_EDGE ( 'NONE', *, *, #1841, .T. ) ;
#14587 = VECTOR ( 'NONE', #8455, 999.9999999999998863 ) ;
#14588 = AXIS2_PLACEMENT_3D ( 'NONE', #17280, #32674, #19971 ) ;
#14589 = CARTESIAN_POINT ( 'NONE',  ( -35.50000000000000000, -113.0140978167141128, -0.6247823525984907977 ) ) ;
#14590 = DIRECTION ( 'NONE',  ( -1.000000000000000000, 0.000000000000000000, -0.000000000000000000 ) ) ;
#14591 = CARTESIAN_POINT ( 'NONE',  ( -36.23083527818512550, -116.0245472910329880, 1.784774454178448932 ) ) ;
#14592 = ORIENTED_EDGE ( 'NONE', *, *, #6035, .F. ) ;
#14593 = CARTESIAN_POINT ( 'NONE',  ( -38.97545270896704039, -113.1123104723225197, 3.847274454178449599 ) ) ;
#14594 = ADVANCED_FACE ( 'NONE', ( #3336 ), #19163, .T. ) ;
#14595 = EDGE_CURVE ( 'NONE', #25789, #7877, #22206, .T. ) ;
#14596 = PLANE ( 'NONE',  #34920 ) ;
#14597 = CARTESIAN_POINT ( 'NONE',  ( -35.50000000000000711, -114.3474311500471430, -1.624782352598427959 ) ) ;
#14598 = ORIENTED_EDGE ( 'NONE', *, *, #13924, .T. ) ;
#14599 = ORIENTED_EDGE ( 'NONE', *, *, #3170, .F. ) ;
#14600 = DIRECTION ( 'NONE',  ( 0.000000000000000000, 0.000000000000000000, 1.000000000000000000 ) ) ;
#14601 = DIRECTION ( 'NONE',  ( -1.000000000000000000, 0.000000000000000000, 0.000000000000000000 ) ) ;
#14603 = VERTEX_POINT ( 'NONE', #14288 ) ;
#14602 = AXIS2_PLACEMENT_3D ( 'NONE', #28502, #12292, #31730 ) ;
#14604 = EDGE_LOOP ( 'NONE', ( #12954, #12356, #35565, #13017 ) ) ;
#14605 = CARTESIAN_POINT ( 'NONE',  ( -34.50000000000000000, -112.0140978167138712, 0.0002176474015661141945 ) ) ;
#14606 = CARTESIAN_POINT ( 'NONE',  ( -37.49999999999999289, -10.15468310254180651, 112.5137715831613008 ) ) ;
#14607 = EDGE_CURVE ( 'NONE', #23898, #9389, #6693, .T. ) ;
#14608 = EDGE_LOOP ( 'NONE', ( #1377, #3305, #17169, #11044 ) ) ;
#14609 = VERTEX_POINT ( 'NONE', #19848 ) ;
#14610 = EDGE_CURVE ( 'NONE', #19467, #7819, #25672, .T. ) ;
#14611 = DIRECTION ( 'NONE',  ( -0.000000000000000000, -0.000000000000000000, -1.000000000000000000 ) ) ;
#14612 = AXIS2_PLACEMENT_3D ( 'NONE', #29462, #23695, #18822 ) ;
#14613 = CARTESIAN_POINT ( 'NONE',  ( -37.99994980024369085, -113.9929510916434339, 12.62670525340494621 ) ) ;
#14614 = VECTOR ( 'NONE', #29365, 1000.000000000000000 ) ;
#14615 = CARTESIAN_POINT ( 'NONE',  ( -34.50000000000000000, -112.0140978167138712, 0.7189676474015718188 ) ) ;
#14616 = CARTESIAN_POINT ( 'NONE',  ( 7.999999999999992895, 0.000000000000000000, 0.000000000000000000 ) ) ;
#14617 = CARTESIAN_POINT ( 'NONE',  ( -35.87040530316090070, -113.9929510916434339, 13.10254527216545917 ) ) ;
#14618 = CIRCLE ( 'NONE', #3804, 19.99999999999998579 ) ;
#14619 = CARTESIAN_POINT ( 'NONE',  ( -35.50160444427493189, -115.9929510916434481, 12.65937477241749853 ) ) ;
#14620 = DIRECTION ( 'NONE',  ( 0.000000000000000000, 0.000000000000000000, 1.000000000000000000 ) ) ;
#14621 = ADVANCED_BREP_SHAPE_REPRESENTATION ( '', ( #22652, #21307 ), #24262 ) ;
#14622 = CARTESIAN_POINT ( 'NONE',  ( -42.49999999999999289, -12.00833024919776371, 94.79903810567661537 ) ) ;
#14623 = DIRECTION ( 'NONE',  ( 0.000000000000000000, 0.3681245526846785854, -0.9297764858882511252 ) ) ;
#14624 = CYLINDRICAL_SURFACE ( 'NONE', #26018, 20.00000000000000711 ) ;
#14625 = CYLINDRICAL_SURFACE ( 'NONE', #11095, 20.00000000000000711 ) ;
#14626 = VERTEX_POINT ( 'NONE', #2819 ) ;
#14627 = LINE ( 'NONE', #25637, #17977 ) ;
#14628 = DIRECTION ( 'NONE',  ( 1.000000000000000000, 0.000000000000000000, 0.000000000000000000 ) ) ;
#14629 = CARTESIAN_POINT ( 'NONE',  ( 0.000000000000000000, 0.000000000000000000, 0.000000000000000000 ) ) ;
#14630 = CARTESIAN_POINT ( 'NONE',  ( 0.9999999999999453770, -6.008326913195871199, -0.7999999999999951594 ) ) ;
#14631 = CONTEXT_DEPENDENT_SHAPE_REPRESENTATION ( #2574, #14966 ) ;
#14632 = DIRECTION ( 'NONE',  ( 0.000000000000000000, 0.000000000000000000, -1.000000000000000000 ) ) ;
#14633 = CARTESIAN_POINT ( 'NONE',  ( 3.799999999999999822, -2.710505431213761085E-17, -45.00000000000000000 ) ) ;
#14634 = ORIENTED_EDGE ( 'NONE', *, *, #14514, .F. ) ;
#14635 = EDGE_CURVE ( 'NONE', #1616, #30950, #13780, .T. ) ;
#14636 = CARTESIAN_POINT ( 'NONE',  ( -3.799999999999999822, 4.653657836759942730E-16, -40.00000000000000000 ) ) ;
#14637 = AXIS2_PLACEMENT_3D ( 'NONE', #16130, #27149, #2489 ) ;
#14638 = DIRECTION ( 'NONE',  ( 0.000000000000000000, 0.3090169943749477288, -0.9510565162951534202 ) ) ;
#14639 = CARTESIAN_POINT ( 'NONE',  ( 46.00000000000000000, -25.98076211353320275, 92.99999999999991473 ) ) ;
#14640 = VERTEX_POINT ( 'NONE', #8354 ) ;
#14641 = ORIENTED_EDGE ( 'NONE', *, *, #13218, .T. ) ;
#14642 = CARTESIAN_POINT ( 'NONE',  ( -38.02454729103295961, -113.6450488405582462, 7.840225545821554398 ) ) ;
#14643 = VERTEX_POINT ( 'NONE', #30346 ) ;
#14644 = AXIS2_PLACEMENT_3D ( 'NONE', #7868, #10941, #22083 ) ;
#14645 = ORIENTED_EDGE ( 'NONE', *, *, #24984, .F. ) ;
#14646 = ORIENTED_EDGE ( 'NONE', *, *, #2381, .F. ) ;
#14647 = CARTESIAN_POINT ( 'NONE',  ( -9.999999999999994671, 0.000000000000000000, 0.000000000000000000 ) ) ;
#14648 = AXIS2_PLACEMENT_3D ( 'NONE', #10337, #16607, #33353 ) ;
#14649 = DIRECTION ( 'NONE',  ( 1.000000000000000000, -0.000000000000000000, -0.000000000000000000 ) ) ;
#14650 = DIRECTION ( 'NONE',  ( 3.469446951953614682E-16, -1.000000000000000000, 0.000000000000000000 ) ) ;
#14651 = AXIS2_PLACEMENT_3D ( 'NONE', #18932, #18753, #7593 ) ;
#14652 = CARTESIAN_POINT ( 'NONE',  ( -35.50000000000000711, -114.9929510916434339, 10.68227981832981044 ) ) ;
#14653 = LINE ( 'NONE', #14306, #10346 ) ;
#14654 = DIRECTION ( 'NONE',  ( 1.000000000000000000, -0.000000000000000000, -0.000000000000000000 ) ) ;
#14655 = CARTESIAN_POINT ( 'NONE',  ( -34.50000000000000000, -114.2598117360253696, 9.542047897280109936 ) ) ;
#14656 = CARTESIAN_POINT ( 'NONE',  ( 8.000000000000000000, 8.128228055639098670, -16.94522934049206242 ) ) ;
#14657 = CLOSED_SHELL ( 'NONE', ( #25407, #23529, #16914, #26676, #28015, #16076, #20160, #3092, #13011, #32238, #3090, #31071, #19527, #11478, #6854, #22610, #28623, #14814, #20317, #13851, #3745, #20639, #22538, #18276, #16512, #23740, #18431, #23338, #25972, #29511, #18766, #11814, #34878, #22051, #8161, #18965, #10367, #10412, #7985, #31937, #20729, #30001, #23777, #14171 ) ) ;
#14658 = PRODUCT_DEFINITION_SHAPE ( 'NONE', 'NONE',  #35619 ) ;
#14659 = AXIS2_PLACEMENT_3D ( 'NONE', #17192, #23138, #6758 ) ;
#14660 = DIRECTION ( 'NONE',  ( -1.000000000000000000, 0.000000000000000000, -0.000000000000000000 ) ) ;
#14661 = ORIENTED_EDGE ( 'NONE', *, *, #12787, .F. ) ;
#14662 = CARTESIAN_POINT ( 'NONE',  ( -35.50000000000000000, -115.9929510916434481, 10.51725893871049067 ) ) ;
#14663 = CYLINDRICAL_SURFACE ( 'NONE', #27475, 20.00000000000000711 ) ;
#14664 = DIRECTION ( 'NONE',  ( 0.000000000000000000, -1.000000000000000000, 0.000000000000000000 ) ) ;
#14665 = CARTESIAN_POINT ( 'NONE',  ( 7.999999999999992895, 39.55064067543098361, -25.36340625197317067 ) ) ;
#14666 = CIRCLE ( 'NONE', #25624, 20.00000000000000711 ) ;
#14667 = CARTESIAN_POINT ( 'NONE',  ( 7.999999999999992895, 43.83938735307295076, -18.28286404005752175 ) ) ;
#14668 = CYLINDRICAL_SURFACE ( 'NONE', #20483, 22.00000000000000000 ) ;
#14669 = DIRECTION ( 'NONE',  ( 0.000000000000000000, 0.000000000000000000, 1.000000000000000000 ) ) ;
#14670 = DIRECTION ( 'NONE',  ( -1.000000000000000000, -1.836970198721029934E-16, -0.000000000000000000 ) ) ;
#14671 = CARTESIAN_POINT ( 'NONE',  ( -9.999999999999994671, 0.000000000000000000, 0.000000000000000000 ) ) ;
#14672 = ORIENTED_EDGE ( 'NONE', *, *, #2901, .F. ) ;
#14673 = CARTESIAN_POINT ( 'NONE',  ( -37.47347596530441649, -114.9754527089670262, 1.972274454178448932 ) ) ;
#14674 = DIRECTION ( 'NONE',  ( 0.000000000000000000, -0.5877852522924802425, 0.8090169943749421222 ) ) ;
#14675 = CARTESIAN_POINT ( 'NONE',  ( -29.99999999999999289, 2.571758278209443239E-15, 0.000000000000000000 ) ) ;
#14676 = ORIENTED_EDGE ( 'NONE', *, *, #26180, .F. ) ;
#14677 = AXIS2_PLACEMENT_3D ( 'NONE', #30422, #13680, #159 ) ;
#14678 = ORIENTED_EDGE ( 'NONE', *, *, #29590, .T. ) ;
#14679 = ADVANCED_FACE ( 'NONE', ( #14994 ), #23098, .T. ) ;
#14680 = DIRECTION ( 'NONE',  ( -1.000000000000000000, 0.000000000000000000, -0.000000000000000000 ) ) ;
#14681 = CARTESIAN_POINT ( 'NONE',  ( 8.000000000000000000, 0.000000000000000000, 0.000000000000000000 ) ) ;
#14682 = EDGE_LOOP ( 'NONE', ( #10327, #20690, #35541, #35034 ) ) ;
#14683 = CARTESIAN_POINT ( 'NONE',  ( -34.92058450342251064, -116.1632251905417945, 6.191024454178448266 ) ) ;
#14684 = EDGE_LOOP ( 'NONE', ( #3594, #35279, #13030, #24493 ) ) ;
#14685 = CYLINDRICAL_SURFACE ( 'NONE', #8329, 4.800000000000000711 ) ;
#14686 = CIRCLE ( 'NONE', #24485, 4.000000000000000000 ) ;
#14687 = DIRECTION ( 'NONE',  ( 0.000000000000000000, -1.067522139062650474E-15, -1.000000000000000000 ) ) ;
#14688 = EDGE_CURVE ( 'NONE', #5174, #891, #18207, .T. ) ;
#14689 = PRODUCT_CONTEXT ( 'NONE', #9855, 'mechanical' ) ;
#14690 = CIRCLE ( 'NONE', #4961, 4.000000000000000000 ) ;
#14691 = CIRCLE ( 'NONE', #34851, 20.00000000000000711 ) ;
#14692 = CARTESIAN_POINT ( 'NONE',  ( 8.000000000000007105, 0.000000000000000000, 0.000000000000000000 ) ) ;
#14693 = ORIENTED_EDGE ( 'NONE', *, *, #33010, .T. ) ;
#14694 = VERTEX_POINT ( 'NONE', #28702 ) ;
#14695 = EDGE_CURVE ( 'NONE', #16232, #25092, #15882, .T. ) ;
#14696 = AXIS2_PLACEMENT_3D ( 'NONE', #6625, #34010, #8968 ) ;
#14697 = CARTESIAN_POINT ( 'NONE',  ( 8.000000000000007105, 5.908880290975762506, -9.604183132802354805 ) ) ;
#14698 = FACE_OUTER_BOUND ( 'NONE', #4964, .T. ) ;
#14699 = EDGE_LOOP ( 'NONE', ( #6379, #23245 ) ) ;
#14700 = CARTESIAN_POINT ( 'NONE',  ( -34.50000000000001421, -12.00833024919776371, 94.79903810567661537 ) ) ;
#14701 = AXIS2_PLACEMENT_3D ( 'NONE', #27116, #2457, #13428 ) ;
#14702 = VECTOR ( 'NONE', #19746, 1000.000000000000000 ) ;
#14703 = CARTESIAN_POINT ( 'NONE',  ( -34.50000000000000000, -113.0796441757086939, 1.890140615870383956 ) ) ;
#14704 = DIRECTION ( 'NONE',  ( -1.000000000000000000, 0.000000000000000000, 0.000000000000000000 ) ) ;
#14705 = FACE_OUTER_BOUND ( 'NONE', #662, .T. ) ;
#14706 = CARTESIAN_POINT ( 'NONE',  ( -39.00000000000000711, -114.9929510916434339, 12.50851088611646311 ) ) ;
#14707 = DIRECTION ( 'NONE',  ( 0.000000000000000000, 0.000000000000000000, -1.000000000000000000 ) ) ;
#14708 = DIRECTION ( 'NONE',  ( 1.000000000000000000, 0.000000000000000000, 0.000000000000000000 ) ) ;
#14709 = CARTESIAN_POINT ( 'NONE',  ( -34.50000000000000000, -114.2067765580549832, 8.517583185305328541 ) ) ;
#14710 = FACE_OUTER_BOUND ( 'NONE', #34640, .T. ) ;
#14711 = EDGE_CURVE ( 'NONE', #28836, #2106, #25099, .T. ) ;
#14712 = CARTESIAN_POINT ( 'NONE',  ( 8.000000000000000000, -8.605879768205133118, -12.89022243466717299 ) ) ;
#14713 = FACE_OUTER_BOUND ( 'NONE', #24030, .T. ) ;
#14714 = DIRECTION ( 'NONE',  ( 0.000000000000000000, -0.3420201433256564449, -0.9396926207859127578 ) ) ;
#14715 = AXIS2_PLACEMENT_3D ( 'NONE', #29043, #31739, #1870 ) ;
#14716 = EDGE_LOOP ( 'NONE', ( #5633, #7043, #15814, #1204 ) ) ;
#14717 = DIRECTION ( 'NONE',  ( -1.000000000000000000, 5.339440136655842133E-16, 1.047965281155519420E-16 ) ) ;
#14718 = VERTEX_POINT ( 'NONE', #14633 ) ;
#14719 = CARTESIAN_POINT ( 'NONE',  ( -37.05926240293131713, -111.0000000000000284, 5.121475545821551734 ) ) ;
#14720 = VECTOR ( 'NONE', #3452, 1000.000000000000000 ) ;
#14721 = DIRECTION ( 'NONE',  ( 1.000000000000000000, 0.000000000000000000, -0.000000000000000000 ) ) ;
#14722 = AXIS2_PLACEMENT_3D ( 'NONE', #6979, #6447, #28954 ) ;
#14723 = CARTESIAN_POINT ( 'NONE',  ( -35.50000000000000711, -113.3474311500483935, -1.624782352598427959 ) ) ;
#14724 = ORIENTED_EDGE ( 'NONE', *, *, #33629, .T. ) ;
#14725 = VERTEX_POINT ( 'NONE', #9072 ) ;
#14726 = AXIS2_PLACEMENT_3D ( 'NONE', #5848, #25108, #6197 ) ;
#14727 = ADVANCED_FACE ( 'NONE', ( #1155 ), #978, .T. ) ;
#14728 = DIRECTION ( 'NONE',  ( 0.000000000000000000, 0.000000000000000000, 1.000000000000000000 ) ) ;
#14729 = DIRECTION ( 'NONE',  ( 0.000000000000000000, 0.000000000000000000, 1.000000000000000000 ) ) ;
#14730 = EDGE_LOOP ( 'NONE', ( #34189, #33752 ) ) ;
#14731 = EDGE_CURVE ( 'NONE', #21342, #30730, #3265, .T. ) ;
#14732 = EDGE_CURVE ( 'NONE', #29371, #29366, #21047, .T. ) ;
#14733 = ORIENTED_EDGE ( 'NONE', *, *, #3416, .T. ) ;
#14734 = VECTOR ( 'NONE', #10575, 1000.000000000000000 ) ;
#14735 = CYLINDRICAL_SURFACE ( 'NONE', #14239, 5.000000000000011546 ) ;
#14736 = ORIENTED_EDGE ( 'NONE', *, *, #8873, .T. ) ;
#14737 = CARTESIAN_POINT ( 'NONE',  ( -38.99999999999999289, -114.0592624029313242, 4.746475545821550845 ) ) ;
#14738 = EDGE_CURVE ( 'NONE', #15547, #16117, #20204, .T. ) ;
#14739 =( NAMED_UNIT ( * ) SI_UNIT ( $, .STERADIAN. ) SOLID_ANGLE_UNIT ( ) );
#14740 = EDGE_CURVE ( 'NONE', #17196, #6339, #27402, .T. ) ;
#14741 = FACE_OUTER_BOUND ( 'NONE', #15742, .T. ) ;
#14742 = AXIS2_PLACEMENT_3D ( 'NONE', #7384, #32570, #15463 ) ;
#14743 = VERTEX_POINT ( 'NONE', #34464 ) ;
#14744 = ORIENTED_EDGE ( 'NONE', *, *, #29725, .T. ) ;
#14745 = CARTESIAN_POINT ( 'NONE',  ( -35.50000000000000000, -111.0140978167138570, -0.1247823525984260717 ) ) ;
#14746 = CARTESIAN_POINT ( 'NONE',  ( -21.15833593587365513, -24.48076211353329157, 98.99999999999994316 ) ) ;
#14747 = ORIENTED_EDGE ( 'NONE', *, *, #23894, .T. ) ;
#14748 = DIRECTION ( 'NONE',  ( 0.000000000000000000, 0.000000000000000000, -1.000000000000000000 ) ) ;
#14749 = AXIS2_PLACEMENT_3D ( 'NONE', #25869, #1193, #9645 ) ;
#14750 = VECTOR ( 'NONE', #22172, 1000.000000000000000 ) ;
#14751 = CARTESIAN_POINT ( 'NONE',  ( -39.00000000000000000, -113.9929510916434339, 11.91443571948719615 ) ) ;
#14752 = AXIS2_PLACEMENT_3D ( 'NONE', #6228, #14144, #11618 ) ;
#14753 = CARTESIAN_POINT ( 'NONE',  ( 7.999999999999992895, -41.20225022064655462, 23.63323037071389621 ) ) ;
#14754 = CARTESIAN_POINT ( 'NONE',  ( -0.1085714285714300953, -3.798448662927791819, 0.000000000000000000 ) ) ;
#14755 = CARTESIAN_POINT ( 'NONE',  ( -37.48437500000004263, -113.9929510916434339, 14.11852480586265024 ) ) ;
#14756 = CARTESIAN_POINT ( 'NONE',  ( 8.000000000000000000, -14.80634052301617309, -8.177498406287382338 ) ) ;
#14757 = EDGE_CURVE ( 'NONE', #23698, #16800, #31989, .T. ) ;
#14758 = CARTESIAN_POINT ( 'NONE',  ( -35.99181955245763476, -114.9929510916434339, 13.11847460610632687 ) ) ;
#14759 = AXIS2_PLACEMENT_3D ( 'NONE', #15920, #30340, #8175 ) ;
#14760 = DIRECTION ( 'NONE',  ( 0.9914448613738109373, -0.1305261922200477154, -1.219156652430115488E-15 ) ) ;
#14761 = ORIENTED_EDGE ( 'NONE', *, *, #11203, .F. ) ;
#14762 = DIRECTION ( 'NONE',  ( -1.000000000000000000, 0.000000000000000000, -0.000000000000000000 ) ) ;
#14763 = PLANE ( 'NONE',  #24970 ) ;
#14764 = EDGE_LOOP ( 'NONE', ( #21420, #15656, #10547, #15296 ) ) ;
#14765 = PRODUCT_RELATED_PRODUCT_CATEGORY ( 'part', '', ( #17848 ) ) ;
#14766 = CARTESIAN_POINT ( 'NONE',  ( -35.56312645773537895, -114.9929510916434339, 12.87038173996308998 ) ) ;
#14767 = VERTEX_POINT ( 'NONE', #14827 ) ;
#14768 = PLANE ( 'NONE',  #34694 ) ;
#14769 = CIRCLE ( 'NONE', #30317, 20.00000000000000711 ) ;
#14770 = ORIENTED_EDGE ( 'NONE', *, *, #23019, .T. ) ;
#14771 = FACE_OUTER_BOUND ( 'NONE', #25432, .T. ) ;
#14772 = ORIENTED_EDGE ( 'NONE', *, *, #24670, .F. ) ;
#14773 = AXIS2_PLACEMENT_3D ( 'NONE', #16499, #13814, #3195 ) ;
#14774 = ADVANCED_FACE ( 'NONE', ( #31389, #12676 ), #22923, .F. ) ;
#14775 = CARTESIAN_POINT ( 'NONE',  ( -35.50000000000000000, -113.0140978167136581, -0.6247823525984261828 ) ) ;
#14776 = DIRECTION ( 'NONE',  ( -1.000000000000000000, 0.000000000000000000, 0.000000000000000000 ) ) ;
#14777 = LINE ( 'NONE', #9381, #15151 ) ;
#14778 = EDGE_CURVE ( 'NONE', #15404, #17296, #30274, .T. ) ;
#14779 = ADVANCED_FACE ( 'NONE', ( #6539 ), #4397, .F. ) ;
#14780 = ORIENTED_EDGE ( 'NONE', *, *, #31705, .T. ) ;
#14781 = CARTESIAN_POINT ( 'NONE',  ( -38.37230871539094323, -112.5438815906447729, 2.441024454178448710 ) ) ;
#14782 = CIRCLE ( 'NONE', #21699, 47.49900000000001654 ) ;
#14783 = VECTOR ( 'NONE', #4362, 1000.000000000000000 ) ;
#14784 = LINE ( 'NONE', #25793, #16511 ) ;
#14785 = CARTESIAN_POINT ( 'NONE',  ( -35.50000000000000711, -112.8511839106603247, -1.611965039240275122 ) ) ;
#14786 = ORIENTED_EDGE ( 'NONE', *, *, #24435, .F. ) ;
#14787 = EDGE_LOOP ( 'NONE', ( #33459, #13906, #27888, #18205 ) ) ;
#14788 = CIRCLE ( 'NONE', #33765, 11.00000000000000000 ) ;
#14789 = DIRECTION ( 'NONE',  ( 0.000000000000000000, -0.5877852522924624790, -0.8090169943749551118 ) ) ;
#14790 = AXIS2_PLACEMENT_3D ( 'NONE', #33221, #8543, #5850 ) ;
#14791 = ADVANCED_FACE ( 'NONE', ( #4050 ), #31744, .T. ) ;
#14792 = DIRECTION ( 'NONE',  ( -1.000000000000000000, 0.000000000000000000, -0.000000000000000000 ) ) ;
#14793 = ORIENTED_EDGE ( 'NONE', *, *, #10323, .T. ) ;
#14794 = VERTEX_POINT ( 'NONE', #34274 ) ;
#14795 = CARTESIAN_POINT ( 'NONE',  ( -34.50000000000000000, -112.9486715495423681, -1.623175561345890472 ) ) ;
#14796 = DIRECTION ( 'NONE',  ( -1.047965281155519913E-16, -6.938893903907192632E-17, -1.000000000000000000 ) ) ;
#14797 = ORIENTED_EDGE ( 'NONE', *, *, #28808, .F. ) ;
#14798 = ORIENTED_EDGE ( 'NONE', *, *, #22973, .F. ) ;
#14799 = EDGE_CURVE ( 'NONE', #9468, #21073, #2747, .T. ) ;
#14800 = CARTESIAN_POINT ( 'NONE',  ( 4.000000000000000000, -0.5097555531874695678, 19.99350267651955093 ) ) ;
#14801 = AXIS2_PLACEMENT_3D ( 'NONE', #15024, #32480, #5486 ) ;
#14802 = TOROIDAL_SURFACE ( 'NONE', #8487, 6.983999999999990216, 0.04099999999999958539 ) ;
#14803 = CARTESIAN_POINT ( 'NONE',  ( -35.83891589277641287, -113.9929510916434339, 13.09299768411358400 ) ) ;
#14804 = CARTESIAN_POINT ( 'NONE',  ( -34.50000000000000000, -113.1256619669233885, 1.895633585076891947 ) ) ;
#14805 = DIRECTION ( 'NONE',  ( -1.047965281155519790E-16, -6.938893903907192632E-17, -1.000000000000000000 ) ) ;
#14806 = CARTESIAN_POINT ( 'NONE',  ( -36.03125000000003553, -113.9929510916434339, 13.11852480586264846 ) ) ;
#14807 = VECTOR ( 'NONE', #19442, 1000.000000000000000 ) ;
#14808 = EDGE_CURVE ( 'NONE', #17845, #3877, #12489, .T. ) ;
#14809 = CARTESIAN_POINT ( 'NONE',  ( -35.50000000000000000, -115.9929510916434481, 12.60752341388803721 ) ) ;
#14810 = DIRECTION ( 'NONE',  ( 0.000000000000000000, 1.000000000000000000, 3.614007241618346010E-15 ) ) ;
#14811 = VECTOR ( 'NONE', #22442, 1000.000000000000000 ) ;
#14812 = EDGE_CURVE ( 'NONE', #17844, #20597, #27248, .T. ) ;
#14813 = CARTESIAN_POINT ( 'NONE',  ( -49.99999999999999289, -26.00000000000000000, 113.9999999999999858 ) ) ;
#14814 = ADVANCED_FACE ( 'NONE', ( #15702 ), #29946, .F. ) ;
#14815 = DIRECTION ( 'NONE',  ( 1.000000000000000000, -5.339440136655842133E-16, -1.047965281155519420E-16 ) ) ;
#14816 = LINE ( 'NONE', #25094, #10492 ) ;
#14817 = CIRCLE ( 'NONE', #34974, 20.00000000000000355 ) ;
#14818 = DIRECTION ( 'NONE',  ( -0.000000000000000000, 0.000000000000000000, -1.000000000000000000 ) ) ;
#14819 = ORIENTED_EDGE ( 'NONE', *, *, #2527, .F. ) ;
#14820 = FACE_OUTER_BOUND ( 'NONE', #34730, .T. ) ;
#14821 = DIRECTION ( 'NONE',  ( 0.000000000000000000, 0.000000000000000000, 1.000000000000000000 ) ) ;
#14822 = CARTESIAN_POINT ( 'NONE',  ( -35.50000000000000711, -113.2637153405686519, 1.912112492696748989 ) ) ;
#14823 = LINE ( 'NONE', #28697, #16701 ) ;
#14824 = EDGE_CURVE ( 'NONE', #4873, #31912, #16051, .T. ) ;
#14825 = EDGE_CURVE ( 'NONE', #22572, #15935, #9601, .T. ) ;
#14826 = CARTESIAN_POINT ( 'NONE',  ( 8.000000000000000000, 0.000000000000000000, 0.000000000000000000 ) ) ;
#14827 = CARTESIAN_POINT ( 'NONE',  ( -34.49999999999998579, -34.27980021920977549, 73.62564434701768334 ) ) ;
#14828 = ORIENTED_EDGE ( 'NONE', *, *, #16909, .T. ) ;
#14829 = CYLINDRICAL_SURFACE ( 'NONE', #35449, 15.49899999999998457 ) ;
#14830 = CARTESIAN_POINT ( 'NONE',  ( -34.50000000000000000, -112.6882700046066645, -2.599147725882136939 ) ) ;
#14831 = DIRECTION ( 'NONE',  ( 0.000000000000000000, -0.9929510916431035783, 0.1185248058626076212 ) ) ;
#14832 = ORIENTED_EDGE ( 'NONE', *, *, #26194, .F. ) ;
#14833 = ORIENTED_EDGE ( 'NONE', *, *, #11448, .T. ) ;
#14834 = CARTESIAN_POINT ( 'NONE',  ( -36.33479806579561000, -114.7490116281687165, 1.691024454178448932 ) ) ;
#14835 = VERTEX_POINT ( 'NONE', #21288 ) ;
#14836 = ORIENTED_EDGE ( 'NONE', *, *, #25168, .T. ) ;
#14837 = ORIENTED_EDGE ( 'NONE', *, *, #9409, .F. ) ;
#14838 = AXIS2_PLACEMENT_3D ( 'NONE', #16423, #27260, #17931 ) ;
#14839 = CARTESIAN_POINT ( 'NONE',  ( -35.50000000000000000, -115.0140978167140986, -0.6247823525984417259 ) ) ;
#14840 = DIRECTION ( 'NONE',  ( -1.000000000000000000, -0.000000000000000000, -0.000000000000000000 ) ) ;
#14841 = DIRECTION ( 'NONE',  ( -1.000000000000000000, 0.000000000000000000, 0.000000000000000000 ) ) ;
#14842 = CARTESIAN_POINT ( 'NONE',  ( -35.50000000000000711, -114.9929510916434339, 10.56126450660895699 ) ) ;
#14843 = DIRECTION ( 'NONE',  ( -1.000000000000000000, 0.000000000000000000, 0.000000000000000000 ) ) ;
#14844 = DIRECTION ( 'NONE',  ( -1.000000000000000000, 0.000000000000000000, 0.000000000000000000 ) ) ;
#14845 = EDGE_CURVE ( 'NONE', #22897, #25036, #32643, .T. ) ;
#14846 = CARTESIAN_POINT ( 'NONE',  ( -34.50000000000000000, -114.0928965812550757, 9.511088712577292270 ) ) ;
#14847 = DIRECTION ( 'NONE',  ( 0.000000000000000000, -0.8660254037844432595, 0.4999999999999918954 ) ) ;
#14848 = EDGE_CURVE ( 'NONE', #3935, #12448, #18946, .T. ) ;
#14849 = CYLINDRICAL_SURFACE ( 'NONE', #8250, 20.00000000000000355 ) ;
#14850 = VERTEX_POINT ( 'NONE', #31918 ) ;
#14851 = CARTESIAN_POINT ( 'NONE',  ( -35.50000000000000000, -114.2114213871176958, 8.518137620934190579 ) ) ;
#14852 = CARTESIAN_POINT ( 'NONE',  ( -35.50000000000000711, -112.0140978167138712, 0.7502176474015694874 ) ) ;
#14853 = DIRECTION ( 'NONE',  ( 0.000000000000000000, -0.8660254037844350439, -0.5000000000000061062 ) ) ;
#14854 = CARTESIAN_POINT ( 'NONE',  ( 8.000000000000000000, -0.9861715913088822116, 17.47118961583599273 ) ) ;
#14855 = CYLINDRICAL_SURFACE ( 'NONE', #30859, 8.000000000000000000 ) ;
#14856 = AXIS2_PLACEMENT_3D ( 'NONE', #13754, #13570, #18786 ) ;
#14857 = CYLINDRICAL_SURFACE ( 'NONE', #31427, 47.49900000000001654 ) ;
#14858 = CYLINDRICAL_SURFACE ( 'NONE', #7762, 2.999999999999988898 ) ;
#14859 = CARTESIAN_POINT ( 'NONE',  ( 4.000000000000000000, 4.898587196589412829E-16, 36.00000000000000000 ) ) ;
#14860 = DIRECTION ( 'NONE',  ( -1.000000000000000000, 0.000000000000000000, 0.000000000000000000 ) ) ;
#14861 = EDGE_LOOP ( 'NONE', ( #2003, #33729, #14254, #2200 ) ) ;
#14862 = CARTESIAN_POINT ( 'NONE',  ( -36.64504884055821776, -112.9754527089670688, 5.215225545821552622 ) ) ;
#14863 = DIRECTION ( 'NONE',  ( -1.000000000000000000, 0.000000000000000000, 0.000000000000000000 ) ) ;
#14864 = DIRECTION ( 'NONE',  ( 1.000000000000000000, -5.339440136655842133E-16, -1.047965281155519420E-16 ) ) ;
#14865 = ORIENTED_EDGE ( 'NONE', *, *, #13092, .T. ) ;
#14866 = ORIENTED_EDGE ( 'NONE', *, *, #26258, .F. ) ;
#14867 = CARTESIAN_POINT ( 'NONE',  ( -34.49999999999998579, -25.99649394950417047, 81.00003093645244689 ) ) ;
#14868 = DIRECTION ( 'NONE',  ( 0.000000000000000000, 0.000000000000000000, -1.000000000000000000 ) ) ;
#14869 = ORIENTED_EDGE ( 'NONE', *, *, #10678, .F. ) ;
#14870 = CARTESIAN_POINT ( 'NONE',  ( -39.99999999999999289, -114.0592624029313242, 9.246475545821549957 ) ) ;
#14871 = ORIENTED_EDGE ( 'NONE', *, *, #33047, .T. ) ;
#14872 = DIRECTION ( 'NONE',  ( -1.000000000000000000, 0.000000000000000000, 0.000000000000000000 ) ) ;
#14873 = PLANE ( 'NONE',  #1459 ) ;
#14874 = CARTESIAN_POINT ( 'NONE',  ( 39.30000000000000426, 10.50000000000000355, 1.285879139104720436E-15 ) ) ;
#14875 = SHAPE_DEFINITION_REPRESENTATION ( #14376, #8186 ) ;
#14876 = CARTESIAN_POINT ( 'NONE',  ( -4.000000000000000000, -2.710505431213761085E-17, 38.00000000000000711 ) ) ;
#14877 = ORIENTED_EDGE ( 'NONE', *, *, #28577, .T. ) ;
#14878 = ORIENTED_EDGE ( 'NONE', *, *, #19363, .T. ) ;
#14879 = CIRCLE ( 'NONE', #33887, 3.799999999999999822 ) ;
#14880 = CARTESIAN_POINT ( 'NONE',  ( 8.000000000000000000, 0.000000000000000000, 0.000000000000000000 ) ) ;
#14881 = CARTESIAN_POINT ( 'NONE',  ( 0.000000000000000000, -2.710505431213761085E-17, 45.99999999999998579 ) ) ;
#14882 = VERTEX_POINT ( 'NONE', #32285 ) ;
#14883 = CARTESIAN_POINT ( 'NONE',  ( 4.000000000000000000, 4.898587196589412829E-16, -55.00000000000000000 ) ) ;
#14884 = CARTESIAN_POINT ( 'NONE',  ( -34.50000000000000000, -114.5974311500472567, -0.6247823525984269599 ) ) ;
#14885 = CARTESIAN_POINT ( 'NONE',  ( -1.479000000000008086, 0.000000000000000000, 0.000000000000000000 ) ) ;
#14886 = DIRECTION ( 'NONE',  ( -1.000000000000000000, 0.000000000000000000, 0.000000000000000000 ) ) ;
#14887 = ADVANCED_FACE ( 'NONE', ( #7604 ), #7437, .T. ) ;
#14888 = CARTESIAN_POINT ( 'NONE',  ( -39.00000000000000711, -114.9929510916434339, 10.85830208992306822 ) ) ;
#14889 = DIRECTION ( 'NONE',  ( 1.000000000000000000, 0.000000000000000000, -1.691777834109591064E-31 ) ) ;
#14890 = CARTESIAN_POINT ( 'NONE',  ( -39.00000000000000711, -114.9929510916434339, 11.73841344789285657 ) ) ;
#14891 = CARTESIAN_POINT ( 'NONE',  ( 4.000000000000000000, 0.5097555531875970214, -19.99350267651952606 ) ) ;
#14892 = CARTESIAN_POINT ( 'NONE',  ( -6.938893903907228378E-15, 0.7408941433508786645, -1.200000000000006617 ) ) ;
#14893 = DIRECTION ( 'NONE',  ( -1.000000000000000000, -0.000000000000000000, -0.000000000000000000 ) ) ;
#14894 = DIRECTION ( 'NONE',  ( 1.000000000000000000, 0.000000000000000000, 0.000000000000000000 ) ) ;
#14895 = APPLICATION_CONTEXT ( 'automotive_design' ) ;
#14896 = CYLINDRICAL_SURFACE ( 'NONE', #22180, 8.000000000000014211 ) ;
#14897 = ORIENTED_EDGE ( 'NONE', *, *, #19633, .T. ) ;
#14898 = CIRCLE ( 'NONE', #2301, 4.000000000000000000 ) ;
#14899 = EDGE_CURVE ( 'NONE', #18111, #23442, #7252, .T. ) ;
#14900 = CARTESIAN_POINT ( 'NONE',  ( -38.18337828418796676, -117.0245472910329738, 4.465225545821550845 ) ) ;
#14901 = LINE ( 'NONE', #31125, #289 ) ;
#14902 = CARTESIAN_POINT ( 'NONE',  ( -35.50000000000000000, -113.0140978167138712, 0.5627176474015715968 ) ) ;
#14903 = ORIENTED_EDGE ( 'NONE', *, *, #6598, .F. ) ;
#14904 = AXIS2_PLACEMENT_3D ( 'NONE', #14435, #9225, #22717 ) ;
#14905 = EDGE_LOOP ( 'NONE', ( #8339, #3148, #9583, #31789 ) ) ;
#14906 = DIRECTION ( 'NONE',  ( 0.000000000000000000, 0.000000000000000000, -1.000000000000000000 ) ) ;
#14907 = DIRECTION ( 'NONE',  ( 0.000000000000000000, 0.000000000000000000, 1.000000000000000000 ) ) ;
#14908 = ORIENTED_EDGE ( 'NONE', *, *, #29189, .F. ) ;
#14909 = ORIENTED_EDGE ( 'NONE', *, *, #30443, .T. ) ;
#14910 = CIRCLE ( 'NONE', #29895, 4.000000000000000000 ) ;
#14911 = AXIS2_PLACEMENT_3D ( 'NONE', #12412, #7182, #9354 ) ;
#14912 = DIRECTION ( 'NONE',  ( -1.000000000000000000, 0.000000000000000000, 0.000000000000000000 ) ) ;
#14913 = ORIENTED_EDGE ( 'NONE', *, *, #6648, .T. ) ;
#14914 = DIRECTION ( 'NONE',  ( 0.000000000000000000, -0.9999978841041033961, 0.002057130845644380805 ) ) ;
#14915 = CARTESIAN_POINT ( 'NONE',  ( 7.999999999999992895, -30.03615769709763583, 42.44795908868979950 ) ) ;
#14916 = ORIENTED_EDGE ( 'NONE', *, *, #29991, .T. ) ;
#14917 = ORIENTED_EDGE ( 'NONE', *, *, #14808, .T. ) ;
#14918 = CARTESIAN_POINT ( 'NONE',  ( -35.50000000000000000, -115.1449503510569059, -2.621568770093253953 ) ) ;
#14919 = CARTESIAN_POINT ( 'NONE',  ( -55.00000000000000000, 6.123233995736780087E-16, 5.000000000000011546 ) ) ;
#14920 = EDGE_LOOP ( 'NONE', ( #8242, #21557, #12499, #12399 ) ) ;
#14921 = CARTESIAN_POINT ( 'NONE',  ( -37.62959469683911351, -114.9929510916434339, 13.10254527216511633 ) ) ;
#14922 = CIRCLE ( 'NONE', #19923, 8.000000000000007105 ) ;
#14923 = EDGE_CURVE ( 'NONE', #577, #16232, #34639, .T. ) ;
#14924 = CARTESIAN_POINT ( 'NONE',  ( -37.56132887387857267, -113.9929510916434339, 14.11732072679899197 ) ) ;
#14925 = ADVANCED_FACE ( 'NONE', ( #29414 ), #18236, .T. ) ;
#14926 = DIRECTION ( 'NONE',  ( 0.000000000000000000, 0.000000000000000000, -1.000000000000000000 ) ) ;
#14927 = DIRECTION ( 'NONE',  ( 0.000000000000000000, -0.6845471059286950544, 0.7289686274214053352 ) ) ;
#14928 = CARTESIAN_POINT ( 'NONE',  ( 4.000000000000000000, 4.898587196589412829E-16, -49.10000000000000142 ) ) ;
#14929 = CARTESIAN_POINT ( 'NONE',  ( -38.99518666717493431, -113.9929510916434339, 12.74107470552714894 ) ) ;
#14931 = CARTESIAN_POINT ( 'NONE',  ( 0.000000000000000000, 0.000000000000000000, -1.200000000000006617 ) ) ;
#14930 = AXIS2_PLACEMENT_3D ( 'NONE', #32327, #5333, #5160 ) ;
#14932 = CARTESIAN_POINT ( 'NONE',  ( -36.07812499999994316, -114.9929510916434339, 13.11852480586264669 ) ) ;
#14933 = CARTESIAN_POINT ( 'NONE',  ( -9.999999999999994671, 0.000000000000000000, 0.000000000000000000 ) ) ;
#14934 = ORIENTED_EDGE ( 'NONE', *, *, #32762, .T. ) ;
#14935 = DIRECTION ( 'NONE',  ( 0.000000000000000000, -0.2538061376417695136, -0.9672551082808337197 ) ) ;
#14936 = FACE_OUTER_BOUND ( 'NONE', #34201, .T. ) ;
#14937 = EDGE_LOOP ( 'NONE', ( #22987, #33870, #14297, #11383 ) ) ;
#14938 = CARTESIAN_POINT ( 'NONE',  ( -35.50000000000000711, -114.9929510916434339, 10.61627146648203812 ) ) ;
#14939 = VERTEX_POINT ( 'NONE', #7783 ) ;
#14940 = EDGE_CURVE ( 'NONE', #33784, #28703, #23983, .T. ) ;
#14941 = CARTESIAN_POINT ( 'NONE',  ( -37.05926240293131713, -115.9999999999999858, 3.378524454178448710 ) ) ;
#14942 = EDGE_CURVE ( 'NONE', #10214, #13511, #13210, .T. ) ;
#14943 = ORIENTED_EDGE ( 'NONE', *, *, #24591, .T. ) ;
#14944 = DIRECTION ( 'NONE',  ( -1.000000000000000000, 0.000000000000000000, 0.000000000000000000 ) ) ;
#14945 = ORIENTED_EDGE ( 'NONE', *, *, #21631, .F. ) ;
#14946 =( REPRESENTATION_RELATIONSHIP ('NONE','NONE', #26607, #2005 ) REPRESENTATION_RELATIONSHIP_WITH_TRANSFORMATION ( #28511 )SHAPE_REPRESENTATION_RELATIONSHIP( ) );
#14947 = CARTESIAN_POINT ( 'NONE',  ( -34.50000000000000000, -113.0140978167137860, 0.8752176474016654106 ) ) ;
#14948 = DIRECTION ( 'NONE',  ( 1.000000000000000000, 0.000000000000000000, 0.000000000000000000 ) ) ;
#14949 = CARTESIAN_POINT ( 'NONE',  ( -36.94073759706868287, -112.0000000000000142, 8.628524454178448266 ) ) ;
#14950 = ORIENTED_EDGE ( 'NONE', *, *, #33524, .T. ) ;
#14951 = CARTESIAN_POINT ( 'NONE',  ( -34.97545270896703329, -113.2308352781851539, 5.909774454178449155 ) ) ;
#14952 = AXIS2_PLACEMENT_3D ( 'NONE', #24832, #5746, #157 ) ;
#14953 = CARTESIAN_POINT ( 'NONE',  ( 0.000000000000000000, 0.000000000000000000, -33.50000000000000711 ) ) ;
#14954 = CARTESIAN_POINT ( 'NONE',  ( -35.50000000000000711, -114.1807644833817648, -1.624782352598427959 ) ) ;
#14955 = ORIENTED_EDGE ( 'NONE', *, *, #13462, .T. ) ;
#14956 = ORIENTED_EDGE ( 'NONE', *, *, #15129, .T. ) ;
#14957 = DIRECTION ( 'NONE',  ( -1.000000000000000000, 0.000000000000000000, 0.000000000000000000 ) ) ;
#14958 = VECTOR ( 'NONE', #31961, 1000.000000000000000 ) ;
#14959 = AXIS2_PLACEMENT_3D ( 'NONE', #24850, #7, #27566 ) ;
#14960 = EDGE_CURVE ( 'NONE', #21576, #28168, #31448, .T. ) ;
#14961 = DIRECTION ( 'NONE',  ( -1.174092375852890260E-15, 4.222049128630259891E-16, 1.000000000000000000 ) ) ;
#14962 = ORIENTED_EDGE ( 'NONE', *, *, #5723, .F. ) ;
#14963 = ORIENTED_EDGE ( 'NONE', *, *, #22015, .F. ) ;
#14964 = CARTESIAN_POINT ( 'NONE',  ( -34.50000000000000000, -113.0071371610607684, 2.888584676720006961 ) ) ;
#14965 = CARTESIAN_POINT ( 'NONE',  ( -35.50000000000000711, -112.7472371723319355, 1.839427296857320648 ) ) ;
#14966 = PRODUCT_DEFINITION_SHAPE ( 'NONE', 'NONE',  #35637 ) ;
#14967 = EDGE_LOOP ( 'NONE', ( #13910, #34784, #29325, #6871, #6248, #21275, #31355, #20827, #24990, #9725, #25472, #20407, #11476, #20776, #2068, #29154, #1420, #24414, #24529, #18027, #29209, #16638, #10000, #14242, #28859, #28210, #20353, #31567, #2859, #35097, #35404, #4926, #10472, #6200, #29457, #1103, #24470, #26761, #21959, #32467, #12619, #18761, #23575, #11019, #13580, #27866, #8547, #90, #8549, #22522, #2295, #32073, #34072, #14989, #31278, #26399, #3204, #8590, #4110, #27235, #17760, #14124, #9032, #4192, #3398, #20756, #12078, #21058, #14036, #11349, #35500, #5665, #8233, #33376, #17386, #31437, #3110 ) ) ;
#14968 = ORIENTED_EDGE ( 'NONE', *, *, #19604, .T. ) ;
#14969 = DIRECTION ( 'NONE',  ( 1.000000000000000000, 0.000000000000000000, 0.000000000000000000 ) ) ;
#14970 = ADVANCED_FACE ( 'NONE', ( #24188 ), #32456, .T. ) ;
#14971 = CARTESIAN_POINT ( 'NONE',  ( -37.93687354226506869, -113.9929510916434339, 12.87038173996323565 ) ) ;
#14972 = EDGE_CURVE ( 'NONE', #25342, #26672, #17061, .T. ) ;
#14973 = CARTESIAN_POINT ( 'NONE',  ( 7.999999999999992895, 0.000000000000000000, 0.000000000000000000 ) ) ;
#14974 = EDGE_CURVE ( 'NONE', #28609, #30332, #29773, .T. ) ;
#14975 = CARTESIAN_POINT ( 'NONE',  ( -35.50000000000000000, -113.9929510916434339, 12.17846912687782712 ) ) ;
#14976 = CARTESIAN_POINT ( 'NONE',  ( -35.50000000000000000, -115.9792481177720731, 10.26484292309424795 ) ) ;
#14977 = UNCERTAINTY_MEASURE_WITH_UNIT (LENGTH_MEASURE( 1.000000000000000082E-05 ), #27787, 'distance_accuracy_value', 'NONE');
#14978 = DIRECTION ( 'NONE',  ( 0.000000000000000000, 0.000000000000000000, 1.000000000000000000 ) ) ;
#14979 = CYLINDRICAL_SURFACE ( 'NONE', #1991, 3.800000000000018918 ) ;
#14980 = EDGE_CURVE ( 'NONE', #18383, #23680, #2155, .T. ) ;
#14981 = CIRCLE ( 'NONE', #23030, 8.000000000000007105 ) ;
#14982 = MECHANICAL_DESIGN_GEOMETRIC_PRESENTATION_REPRESENTATION (  '', ( #30529 ), #623 ) ;
#14983 = PLANE ( 'NONE',  #10246 ) ;
#14984 = DIRECTION ( 'NONE',  ( -0.000000000000000000, -0.9659258262890674240, -0.2588190451025240701 ) ) ;
#14985 = CIRCLE ( 'NONE', #9240, 20.00000000000000711 ) ;
#14986 = CARTESIAN_POINT ( 'NONE',  ( 8.000000000000007105, -9.433698091065103597, 1.111908866155073117 ) ) ;
#14987 = ADVANCED_FACE ( 'NONE', ( #11035 ), #21997, .T. ) ;
#14988 = AXIS2_PLACEMENT_3D ( 'NONE', #3210, #13995, #8587 ) ;
#14989 = ORIENTED_EDGE ( 'NONE', *, *, #13937, .F. ) ;
#14990 = DIRECTION ( 'NONE',  ( 0.000000000000000000, 0.000000000000000000, 1.000000000000000000 ) ) ;
#14991 = CARTESIAN_POINT ( 'NONE',  ( -35.50000000000000711, -112.8655373925166572, 1.864575885149403423 ) ) ;
#14992 = CARTESIAN_POINT ( 'NONE',  ( -37.49999999999999289, -11.52052244843579309, 115.1848168619253698 ) ) ;
#14993 = CARTESIAN_POINT ( 'NONE',  ( -35.50000000000000711, -114.0998638248492085, 9.511920366020609308 ) ) ;
#14994 = FACE_OUTER_BOUND ( 'NONE', #787, .T. ) ;
#14995 = VERTEX_POINT ( 'NONE', #24719 ) ;
#14996 = DIRECTION ( 'NONE',  ( -1.783119874454246424E-31, -1.187911941725854497E-31, 1.000000000000000000 ) ) ;
#14997 = CARTESIAN_POINT ( 'NONE',  ( -34.50000000000000000, -113.4307644833805142, -2.624782352598442614 ) ) ;
#14998 = CYLINDRICAL_SURFACE ( 'NONE', #25442, 7.999999999999992895 ) ;
#14999 = ORIENTED_EDGE ( 'NONE', *, *, #13890, .F. ) ;
#15000 = VERTEX_POINT ( 'NONE', #27940 ) ;
#15001 = CARTESIAN_POINT ( 'NONE',  ( -36.25098837183130485, -114.6652019342044184, 8.683975545821549957 ) ) ;
#15002 = ORIENTED_EDGE ( 'NONE', *, *, #6405, .F. ) ;
#15003 = EDGE_CURVE ( 'NONE', #26946, #25789, #3290, .T. ) ;
#15004 = ORIENTED_EDGE ( 'NONE', *, *, #26373, .F. ) ;
#15005 = ORIENTED_EDGE ( 'NONE', *, *, #6968, .F. ) ;
#15006 = CARTESIAN_POINT ( 'NONE',  ( -35.50000000000000000, -115.0140978167138712, -0.3747823525984422255 ) ) ;
#15007 = EDGE_CURVE ( 'NONE', #24147, #4250, #13904, .T. ) ;
#15009 = EDGE_CURVE ( 'NONE', #7912, #23627, #33760, .T. ) ;
#15008 = AXIS2_PLACEMENT_3D ( 'NONE', #4178, #1649, #1461 ) ;
#15010 = MECHANICAL_DESIGN_GEOMETRIC_PRESENTATION_REPRESENTATION (  '', ( #15570 ), #2402 ) ;
#15011 = AXIS2_PLACEMENT_3D ( 'NONE', #33651, #30782, #6115 ) ;
#15012 = DIRECTION ( 'NONE',  ( -1.000000000000000000, 0.000000000000000000, 0.000000000000000000 ) ) ;
#15013 = CARTESIAN_POINT ( 'NONE',  ( 70.00000000000001421, 81.48267994499606459, 30.15054357219658954 ) ) ;
#15014 = CARTESIAN_POINT ( 'NONE',  ( -35.50040135968785648, -114.9929510916434339, 12.63896776382214071 ) ) ;
#15015 = CARTESIAN_POINT ( 'NONE',  ( -90.00000000000002842, -4.871103520542888323E-16, -7.020000000000039542 ) ) ;
#15016 = EDGE_CURVE ( 'NONE', #27829, #5432, #5979, .T. ) ;
#15017 = CYLINDRICAL_SURFACE ( 'NONE', #4542, 47.49900000000001654 ) ;
#15018 = EDGE_CURVE ( 'NONE', #33791, #25789, #21822, .T. ) ;
#15019 = CARTESIAN_POINT ( 'NONE',  ( -34.51922597003733273, -114.9929510916434339, 12.86289566494349224 ) ) ;
#15020 = DIRECTION ( 'NONE',  ( 1.000000000000000000, 0.000000000000000000, 0.000000000000000000 ) ) ;
#15021 = LINE ( 'NONE', #31066, #7126 ) ;
#15022 = VERTEX_POINT ( 'NONE', #27777 ) ;
#15023 = CARTESIAN_POINT ( 'NONE',  ( -35.50000000000000000, -114.2067765580549832, 8.517583185305328541 ) ) ;
#15024 = CARTESIAN_POINT ( 'NONE',  ( 7.999999999999992895, 11.46872990052444408, -45.56340405422432127 ) ) ;
#15025 = CARTESIAN_POINT ( 'NONE',  ( -1.519999999999993578, 0.000000000000000000, 0.000000000000000000 ) ) ;
#15026 = CARTESIAN_POINT ( 'NONE',  ( -34.49999999999998579, -22.68172400785658382, 87.71410161513770731 ) ) ;
#15027 = FACE_BOUND ( 'NONE', #6646, .T. ) ;
#15028 = LINE ( 'NONE', #1363, #30309 ) ;
#15029 = CYLINDRICAL_SURFACE ( 'NONE', #27898, 20.00000000000000355 ) ;
#15030 = LINE ( 'NONE', #28737, #390 ) ;
#15031 = CARTESIAN_POINT ( 'NONE',  ( 0.000000000000000000, 10.58300524425836109, 3.000000000000002665 ) ) ;
#15032 = ORIENTED_EDGE ( 'NONE', *, *, #13664, .T. ) ;
#15033 = CIRCLE ( 'NONE', #28854, 47.49900000000001654 ) ;
#15034 = CARTESIAN_POINT ( 'NONE',  ( -36.33479806579560289, -113.2509883718313262, 8.308975545821549957 ) ) ;
#15035 = AXIS2_PLACEMENT_3D ( 'NONE', #11475, #8760, #6074 ) ;
#15036 = PLANE ( 'NONE',  #24436 ) ;
#15037 = LINE ( 'NONE', #33965, #23436 ) ;
#15038 = EDGE_LOOP ( 'NONE', ( #8367, #29641, #10086, #7326 ) ) ;
#15039 = VERTEX_POINT ( 'NONE', #10863 ) ;
#15040 = DIRECTION ( 'NONE',  ( 1.000000000000000000, 0.000000000000000000, -0.000000000000000000 ) ) ;
#15041 = EDGE_LOOP ( 'NONE', ( #27680, #35322, #21381, #34651 ) ) ;
#15042 = CARTESIAN_POINT ( 'NONE',  ( -38.18337828418796676, -117.0245472910329738, 5.965225545821550845 ) ) ;
#15043 = ORIENTED_EDGE ( 'NONE', *, *, #4421, .T. ) ;
#15044 = EDGE_CURVE ( 'NONE', #31746, #28247, #28574, .T. ) ;
#15045 = LINE ( 'NONE', #23334, #15408 ) ;
#15046 = EDGE_CURVE ( 'NONE', #29853, #22200, #30120, .T. ) ;
#15047 = DIRECTION ( 'NONE',  ( 0.000000000000000000, -0.9822872507286903865, 0.1873813145857150808 ) ) ;
#15048 = CARTESIAN_POINT ( 'NONE',  ( -42.49999999999999289, -22.68172400785649501, 82.28589838486220742 ) ) ;
#15049 = ORIENTED_EDGE ( 'NONE', *, *, #9326, .F. ) ;
#15050 = EDGE_LOOP ( 'NONE', ( #3472, #3551, #21390, #16753 ) ) ;
#15051 = DIRECTION ( 'NONE',  ( -1.000000000000000000, 0.000000000000000000, 0.000000000000000000 ) ) ;
#15052 = DIRECTION ( 'NONE',  ( 0.000000000000000000, 0.000000000000000000, -1.000000000000000000 ) ) ;
#15053 = CIRCLE ( 'NONE', #13918, 8.000000000000000000 ) ;
#15054 = VERTEX_POINT ( 'NONE', #16935 ) ;
#15055 = CIRCLE ( 'NONE', #23112, 20.00000000000000355 ) ;
#15056 = FACE_OUTER_BOUND ( 'NONE', #165, .T. ) ;
#15057 = CARTESIAN_POINT ( 'NONE',  ( -34.50000000000000000, -112.5103839485166333, -1.498529437127682495 ) ) ;
#15058 = CYLINDRICAL_SURFACE ( 'NONE', #12501, 22.00000000000000000 ) ;
#15059 = CARTESIAN_POINT ( 'NONE',  ( 0.000000000000000000, 19.35373470438985777, 10.46102064772347795 ) ) ;
#15060 = CARTESIAN_POINT ( 'NONE',  ( -36.07812499999994316, -115.9929510916434481, 14.11852480586265024 ) ) ;
#15061 = CARTESIAN_POINT ( 'NONE',  ( -34.49999999999998579, -25.98076211353320986, 84.99999999999994316 ) ) ;
#15062 = DIRECTION ( 'NONE',  ( 0.000000000000000000, 0.000000000000000000, -1.000000000000000000 ) ) ;
#15063 = CARTESIAN_POINT ( 'NONE',  ( -37.98325232167028531, -114.9929510916434339, 14.04194344061727406 ) ) ;
#15064 = DIRECTION ( 'NONE',  ( 0.000000000000000000, 0.8443279255020125218, 0.5358267949790005424 ) ) ;
#15065 = AXIS2_PLACEMENT_3D ( 'NONE', #6357, #3675, #22914 ) ;
#15066 = LINE ( 'NONE', #8780, #14702 ) ;
#15067 = FACE_BOUND ( 'NONE', #20270, .T. ) ;
#15068 = CARTESIAN_POINT ( 'NONE',  ( 0.000000000000000000, 32.32520163883582853, 34.09746168776048592 ) ) ;
#15069 = ORIENTED_EDGE ( 'NONE', *, *, #13484, .T. ) ;
#15070 = CARTESIAN_POINT ( 'NONE',  ( -34.00000000000000000, -113.9407375970686758, 3.996475545821551734 ) ) ;
#15071 = DIRECTION ( 'NONE',  ( -1.000000000000000000, 0.000000000000000000, 0.000000000000000000 ) ) ;
#15072 = CARTESIAN_POINT ( 'NONE',  ( -35.50000000000000000, -113.0140978167138712, -0.6247823525979733228 ) ) ;
#15073 = ORIENTED_EDGE ( 'NONE', *, *, #24883, .T. ) ;
#15074 = VERTEX_POINT ( 'NONE', #33514 ) ;
#15075 = CARTESIAN_POINT ( 'NONE',  ( 0.000000000000000000, -47.00885577955417460, 6.806061952192132836 ) ) ;
#15076 = AXIS2_PLACEMENT_3D ( 'NONE', #8290, #8818, #30793 ) ;
#15077 = FACE_OUTER_BOUND ( 'NONE', #7027, .T. ) ;
#15078 = VERTEX_POINT ( 'NONE', #3116 ) ;
#15079 = VERTEX_POINT ( 'NONE', #388 ) ;
#15080 = AXIS2_PLACEMENT_3D ( 'NONE', #20941, #4947, #31760 ) ;
#15081 = VERTEX_POINT ( 'NONE', #27608 ) ;
#15082 = EDGE_CURVE ( 'NONE', #16940, #14203, #22822, .T. ) ;
#15083 = DIRECTION ( 'NONE',  ( 1.000000000000000000, 0.000000000000000000, 0.000000000000000000 ) ) ;
#15084 = CARTESIAN_POINT ( 'NONE',  ( -34.97545270896703329, -114.7691647218148745, 5.590225545821551734 ) ) ;
#15085 = CARTESIAN_POINT ( 'NONE',  ( 38.00000000000000000, 3.252606517456513302E-16, 70.00000000000001421 ) ) ;
#15086 = DIRECTION ( 'NONE',  ( -1.000000000000000000, 0.000000000000000000, 0.000000000000000000 ) ) ;
#15087 = ORIENTED_EDGE ( 'NONE', *, *, #11251, .F. ) ;
#15088 = ORIENTED_EDGE ( 'NONE', *, *, #33049, .F. ) ;
#15089 = CARTESIAN_POINT ( 'NONE',  ( -35.50000000000000000, -115.5324766040685631, -2.560864217809699195 ) ) ;
#15090 = VECTOR ( 'NONE', #26378, 1000.000000000000000 ) ;
#15091 = PLANE ( 'NONE',  #4233 ) ;
#15092 = EDGE_CURVE ( 'NONE', #16713, #11969, #5019, .T. ) ;
#15093 = DIRECTION ( 'NONE',  ( -1.000000000000000000, 0.000000000000000000, 0.000000000000000000 ) ) ;
#15094 = ORIENTED_EDGE ( 'NONE', *, *, #7549, .T. ) ;
#15095 = CARTESIAN_POINT ( 'NONE',  ( -37.53269373325071712, -114.9929510916434339, 13.11752178341324360 ) ) ;
#15096 = AXIS2_PLACEMENT_3D ( 'NONE', #14277, #16799, #11235 ) ;
#15097 = CARTESIAN_POINT ( 'NONE',  ( -34.50000000000000000, -114.1414532730574507, 9.517316564499758158 ) ) ;
#15098 = CIRCLE ( 'NONE', #29505, 20.00000000000000711 ) ;
#15099 = CARTESIAN_POINT ( 'NONE',  ( 7.999999999999992895, 0.000000000000000000, 0.000000000000000000 ) ) ;
#15100 = CARTESIAN_POINT ( 'NONE',  ( -36.99999999999989342, -114.9929510916434339, 13.11852480586264669 ) ) ;
#15101 = DIRECTION ( 'NONE',  ( -1.000000000000000000, -1.734723475976807094E-16, -0.000000000000000000 ) ) ;
#15102 = AXIS2_PLACEMENT_3D ( 'NONE', #6729, #3688, #17705 ) ;
#15103 = CARTESIAN_POINT ( 'NONE',  ( -37.42187499999996447, -113.9929510916434339, 14.11852480586265024 ) ) ;
#15104 = LINE ( 'NONE', #26113, #2701 ) ;
#15105 = CARTESIAN_POINT ( 'NONE',  ( -35.50000000000000711, -114.9929510916434339, 12.57451923796416082 ) ) ;
#15106 = FACE_OUTER_BOUND ( 'NONE', #11597, .T. ) ;
#15107 = VERTEX_POINT ( 'NONE', #14249 ) ;
#15108 = CARTESIAN_POINT ( 'NONE',  ( 8.000000000000000000, -5.482169781018729537, -16.00140663693126086 ) ) ;
#15109 = DIRECTION ( 'NONE',  ( -1.000000000000000000, 0.000000000000000000, 0.000000000000000000 ) ) ;
#15110 = ORIENTED_EDGE ( 'NONE', *, *, #26516, .F. ) ;
#15111 = CARTESIAN_POINT ( 'NONE',  ( -35.50000000000000711, -114.9929517792218689, 10.50900788599415314 ) ) ;
#15112 = ORIENTED_EDGE ( 'NONE', *, *, #2697, .T. ) ;
#15113 = CARTESIAN_POINT ( 'NONE',  ( -35.00000000000000000, -114.0592624029313242, 3.003524454178448710 ) ) ;
#15114 = ORIENTED_EDGE ( 'NONE', *, *, #11699, .T. ) ;
#15115 = CARTESIAN_POINT ( 'NONE',  ( -34.49999999999998579, -5.633167542791597704, 121.0048025873810218 ) ) ;
#15116 = ORIENTED_EDGE ( 'NONE', *, *, #16794, .F. ) ;
#15117 = CARTESIAN_POINT ( 'NONE',  ( -34.50000000000000000, -113.0140978167138712, -0.1247823525984260717 ) ) ;
#15118 = DIRECTION ( 'NONE',  ( -5.339440136655842133E-16, -1.000000000000000000, 6.938893903907197563E-17 ) ) ;
#15119 = DIRECTION ( 'NONE',  ( 0.000000000000000000, 0.000000000000000000, -1.000000000000000000 ) ) ;
#15120 = VERTEX_POINT ( 'NONE', #16767 ) ;
#15121 = CARTESIAN_POINT ( 'NONE',  ( -38.45611840935523418, -115.3723087153909432, 6.566024454178448266 ) ) ;
#15122 = CARTESIAN_POINT ( 'NONE',  ( -4.121423858225413461, -12.61643262889540473, 0.000000000000000000 ) ) ;
#15123 = AXIS2_PLACEMENT_3D ( 'NONE', #4924, #32630, #32985 ) ;
#15124 = ADVANCED_FACE ( 'NONE', ( #27427 ), #32820, .T. ) ;
#15125 = CARTESIAN_POINT ( 'NONE',  ( -35.50000000000000711, -112.5103839485166333, -1.498529437127682495 ) ) ;
#15126 = AXIS2_PLACEMENT_3D ( 'NONE', #16836, #35601, #3183 ) ;
#15127 = VERTEX_POINT ( 'NONE', #11389 ) ;
#15128 = ORIENTED_EDGE ( 'NONE', *, *, #33644, .F. ) ;
#15129 = EDGE_CURVE ( 'NONE', #1992, #22338, #21669, .T. ) ;
#15130 = CARTESIAN_POINT ( 'NONE',  ( 7.999999999999992895, 0.000000000000000000, 0.000000000000000000 ) ) ;
#15131 = AXIS2_PLACEMENT_3D ( 'NONE', #26723, #2060, #4404 ) ;
#15132 = FILL_AREA_STYLE ('',( #20544 ) ) ;
#15133 = LINE ( 'NONE', #25966, #9214 ) ;
#15134 = EDGE_LOOP ( 'NONE', ( #14102, #4023, #34499, #3199 ) ) ;
#15135 = ORIENTED_EDGE ( 'NONE', *, *, #20086, .F. ) ;
#15136 = CARTESIAN_POINT ( 'NONE',  ( -34.50000000000000000, -113.8474311500459777, -1.624782352598427959 ) ) ;
#15137 = CARTESIAN_POINT ( 'NONE',  ( -35.50000000000000711, -112.0250551866464548, 1.025914454044489332 ) ) ;
#15138 = ADVANCED_FACE ( 'NONE', ( #19636 ), #11556, .T. ) ;
#15139 = CARTESIAN_POINT ( 'NONE',  ( 4.000000000000003553, -9.508666619816507293, -19.83898331853700370 ) ) ;
#15140 = ORIENTED_EDGE ( 'NONE', *, *, #19598, .T. ) ;
#15141 = ORIENTED_EDGE ( 'NONE', *, *, #28401, .F. ) ;
#15142 = DIRECTION ( 'NONE',  ( -1.000000000000000000, -0.000000000000000000, 0.000000000000000000 ) ) ;
#15143 = CIRCLE ( 'NONE', #23203, 15.49899999999998457 ) ;
#15144 = CIRCLE ( 'NONE', #2547, 4.000000000000000000 ) ;
#15145 = CARTESIAN_POINT ( 'NONE',  ( -37.66108410722335265, -113.9929510916434339, 13.09299768411426612 ) ) ;
#15146 = DIRECTION ( 'NONE',  ( -1.000000000000000000, 0.000000000000000000, 0.000000000000000000 ) ) ;
#15147 = CARTESIAN_POINT ( 'NONE',  ( -37.34375000000001421, -113.9929510916434339, 13.11852480586264846 ) ) ;
#15148 = CARTESIAN_POINT ( 'NONE',  ( -35.50000000000000000, -115.9929510916434481, 10.56126450660895699 ) ) ;
#15149 = CARTESIAN_POINT ( 'NONE',  ( 7.999999999999992895, 46.11014828289842882, -9.022736828080857308 ) ) ;
#15151 = VECTOR ( 'NONE', #12807, 1000.000000000000000 ) ;
#15150 = CYLINDRICAL_SURFACE ( 'NONE', #7185, 20.00000000000000355 ) ;
#15152 = AXIS2_PLACEMENT_3D ( 'NONE', #21314, #24049, #31949 ) ;
#15153 = VERTEX_POINT ( 'NONE', #30815 ) ;
#15154 = DIRECTION ( 'NONE',  ( -1.000000000000000000, 0.000000000000000000, 0.000000000000000000 ) ) ;
#15155 = DIRECTION ( 'NONE',  ( -1.000000000000000000, 0.000000000000000000, 0.000000000000000000 ) ) ;
#15156 = DIRECTION ( 'NONE',  ( 0.000000000000000000, 0.000000000000000000, -1.000000000000000000 ) ) ;
#15157 = EDGE_CURVE ( 'NONE', #16196, #6246, #6153, .T. ) ;
#15158 = VERTEX_POINT ( 'NONE', #35536 ) ;
#15159 = DIRECTION ( 'NONE',  ( 1.000000000000000000, 0.000000000000000000, 0.000000000000000000 ) ) ;
#15160 = CARTESIAN_POINT ( 'NONE',  ( -35.50000000000000711, -112.0140978167138712, -0.4685323525984295134 ) ) ;
#15161 = DIRECTION ( 'NONE',  ( 0.000000000000000000, -0.8090169943749533354, 0.5877852522924649215 ) ) ;
#15162 = CARTESIAN_POINT ( 'NONE',  ( -35.50000000000000711, -114.0743172650041686, 9.508870970061893857 ) ) ;
#15163 = DIRECTION ( 'NONE',  ( 0.000000000000000000, -0.8090169943749405679, -0.5877852522924825740 ) ) ;
#15164 = ORIENTED_EDGE ( 'NONE', *, *, #7459, .F. ) ;
#15165 = DIRECTION ( 'NONE',  ( 0.000000000000000000, 0.000000000000000000, -1.000000000000000000 ) ) ;
#15166 = ADVANCED_FACE ( 'NONE', ( #8139 ), #12828, .T. ) ;
#15167 = CARTESIAN_POINT ( 'NONE',  ( -34.50000000000000000, -117.0140978167138854, -0.5622823525984408377 ) ) ;
#15168 = CARTESIAN_POINT ( 'NONE',  ( -21.15833593587365513, -27.48076211353330578, 101.9999999999999432 ) ) ;
#15169 = VERTEX_POINT ( 'NONE', #22354 ) ;
#15170 = VERTEX_POINT ( 'NONE', #30652 ) ;
#15171 = EDGE_CURVE ( 'NONE', #9761, #17170, #5986, .T. ) ;
#15172 = CARTESIAN_POINT ( 'NONE',  ( -35.99999999999999289, -114.0592624029313242, 3.003524454178448710 ) ) ;
#15173 = EDGE_CURVE ( 'NONE', #20385, #1882, #11563, .T. ) ;
#15174 = EDGE_LOOP ( 'NONE', ( #30605, #2160, #15603, #31146, #25524 ) ) ;
#15175 = ORIENTED_EDGE ( 'NONE', *, *, #10163, .T. ) ;
#15176 = CARTESIAN_POINT ( 'NONE',  ( -35.50000000000000000, -115.0140978167137860, -0.6247823525984403936 ) ) ;
#15177 = AXIS2_PLACEMENT_3D ( 'NONE', #31130, #23198, #28613 ) ;
#15178 = EDGE_CURVE ( 'NONE', #7873, #11499, #5578, .T. ) ;
#15179 = CARTESIAN_POINT ( 'NONE',  ( -10.00000000000000178, 0.000000000000000000, 0.000000000000000000 ) ) ;
#15180 = EDGE_CURVE ( 'NONE', #33007, #25823, #25702, .T. ) ;
#15181 = PLANE ( 'NONE',  #25445 ) ;
#15182 = CARTESIAN_POINT ( 'NONE',  ( -35.50025087934803736, -114.9929510916434339, 12.63488142334835196 ) ) ;
#15183 = DIRECTION ( 'NONE',  ( -1.000000000000000000, 0.000000000000000000, 0.000000000000000000 ) ) ;
#15184 = CARTESIAN_POINT ( 'NONE',  ( -37.56132887387857267, -114.9929510916434339, 14.11732072679899197 ) ) ;
#15185 = DIRECTION ( 'NONE',  ( -1.734723475976807094E-16, 0.5000000000000092149, -0.8660254037844333785 ) ) ;
#15186 = LINE ( 'NONE', #20948, #30137 ) ;
#15187 = ORIENTED_EDGE ( 'NONE', *, *, #9512, .F. ) ;
#15188 = CARTESIAN_POINT ( 'NONE',  ( -35.50000000000000000, -115.9929510916434481, 12.60752341388803721 ) ) ;
#15189 = CARTESIAN_POINT ( 'NONE',  ( -35.50000000000000711, -114.8474311500471572, -1.624782352598427959 ) ) ;
#15190 =( LENGTH_UNIT ( ) NAMED_UNIT ( * ) SI_UNIT ( .MILLI., .METRE. ) );
#15191 = LINE ( 'NONE', #34671, #20489 ) ;
#15192 = ADVANCED_FACE ( 'NONE', ( #12275 ), #15309, .T. ) ;
#15193 = LINE ( 'NONE', #13069, #35504 ) ;
#15194 = CARTESIAN_POINT ( 'NONE',  ( 4.000000000000003553, -7.162210897276083621, 51.50439529848826936 ) ) ;
#15195 = DIRECTION ( 'NONE',  ( 1.174092375852890260E-15, -4.222049128630259891E-16, -1.000000000000000000 ) ) ;
#15196 = AXIS2_PLACEMENT_3D ( 'NONE', #3387, #3030, #11467 ) ;
#15197 = AXIS2_PLACEMENT_3D ( 'NONE', #15962, #24268, #10755 ) ;
#15198 = CARTESIAN_POINT ( 'NONE',  ( 3.799999999999999822, 0.000000000000000000, -40.00000000000000000 ) ) ;
#15199 = CARTESIAN_POINT ( 'NONE',  ( -46.00000000000000000, 9.797174393178841435E-16, 61.99999999999999289 ) ) ;
#15200 = ORIENTED_EDGE ( 'NONE', *, *, #10525, .F. ) ;
#15201 = ADVANCED_FACE ( 'NONE', ( #1290 ), #31000, .T. ) ;
#15202 = CARTESIAN_POINT ( 'NONE',  ( -37.35495115944176803, -115.0245472910329880, 7.465225545821552622 ) ) ;
#15203 = CYLINDRICAL_SURFACE ( 'NONE', #7202, 20.00000000000000355 ) ;
#15204 = CARTESIAN_POINT ( 'NONE',  ( 0.000000000000000000, 0.000000000000000000, -49.10000000000000142 ) ) ;
#15205 = AXIS2_PLACEMENT_3D ( 'NONE', #11115, #13636, #19379 ) ;
#15206 = EDGE_LOOP ( 'NONE', ( #8422, #22121, #25784, #12902 ) ) ;
#15207 = EDGE_LOOP ( 'NONE', ( #18825, #34229, #17282, #5451 ) ) ;
#15208 = SURFACE_STYLE_USAGE ( .BOTH. , #18284 ) ;
#15209 = CARTESIAN_POINT ( 'NONE',  ( 0.000000000000000000, 3.384281271888069487, -18.48663108841355296 ) ) ;
#15210 = ORIENTED_EDGE ( 'NONE', *, *, #12390, .T. ) ;
#15211 = ADVANCED_FACE ( 'NONE', ( #6867 ), #23067, .F. ) ;
#15212 = CARTESIAN_POINT ( 'NONE',  ( -35.81662171581203324, -110.9754527089670546, 9.715225545821551734 ) ) ;
#15213 = EDGE_CURVE ( 'NONE', #10641, #21218, #392, .T. ) ;
#15214 = ORIENTED_EDGE ( 'NONE', *, *, #34592, .T. ) ;
#15215 = AXIS2_PLACEMENT_3D ( 'NONE', #31198, #6526, #23459 ) ;
#15216 = ORIENTED_EDGE ( 'NONE', *, *, #29832, .T. ) ;
#15217 = CARTESIAN_POINT ( 'NONE',  ( 0.000000000000000000, 4.898587196589412829E-16, -4.000000000000000000 ) ) ;
#15218 = DIRECTION ( 'NONE',  ( -1.000000000000000000, 0.000000000000000000, 0.000000000000000000 ) ) ;
#15219 = EDGE_CURVE ( 'NONE', #14718, #28677, #28038, .T. ) ;
#15220 = CARTESIAN_POINT ( 'NONE',  ( 0.2000000000000057288, -6.997142273814354496, -0.7999999999999951594 ) ) ;
#15221 = ORIENTED_EDGE ( 'NONE', *, *, #17833, .F. ) ;
#15222 = VERTEX_POINT ( 'NONE', #3651 ) ;
#15223 = VECTOR ( 'NONE', #1359, 1000.000000000000000 ) ;
#15224 = AXIS2_PLACEMENT_3D ( 'NONE', #25682, #20604, #9456 ) ;
#15225 = CARTESIAN_POINT ( 'NONE',  ( 70.00001200000001234, -29.17942948312593643, 87.45818687989958562 ) ) ;
#15226 = CYLINDRICAL_SURFACE ( 'NONE', #2861, 20.00000000000000355 ) ;
#15227 = EDGE_LOOP ( 'NONE', ( #353, #3689, #15247, #24843 ) ) ;
#15228 = CARTESIAN_POINT ( 'NONE',  ( 63.00000000000001421, -28.31857036507964764, 80.03062855292515110 ) ) ;
#15229 = CIRCLE ( 'NONE', #35368, 20.00000000000000355 ) ;
#15230 = CARTESIAN_POINT ( 'NONE',  ( 7.999999999999992895, -42.60732521687556584, -19.80331771201704427 ) ) ;
#15231 = DIRECTION ( 'NONE',  ( 1.000000000000000000, -5.339440136655842133E-16, -1.047965281155519420E-16 ) ) ;
#15232 = CIRCLE ( 'NONE', #3190, 17.49900000000001654 ) ;
#15233 = CARTESIAN_POINT ( 'NONE',  ( -34.50000000000000000, -115.9929510916434481, 12.53051367006571581 ) ) ;
#15234 = LINE ( 'NONE', #12741, #1967 ) ;
#15235 = LINE ( 'NONE', #9681, #30676 ) ;
#15236 = CARTESIAN_POINT ( 'NONE',  ( -34.68937937320795584, -115.9929510916434481, 13.37409560816408671 ) ) ;
#15237 = CARTESIAN_POINT ( 'NONE',  ( -34.49999999999998579, -37.28532556477433246, 76.74125644078564790 ) ) ;
#15238 = EDGE_CURVE ( 'NONE', #908, #25349, #17839, .T. ) ;
#15239 = FACE_OUTER_BOUND ( 'NONE', #2902, .T. ) ;
#15240 = CIRCLE ( 'NONE', #27353, 3.999999999999994671 ) ;
#15241 = DIRECTION ( 'NONE',  ( 0.000000000000000000, -6.866613759074853001E-15, 1.000000000000000000 ) ) ;
#15242 = DIRECTION ( 'NONE',  ( 1.000000000000000000, -1.110223024625156540E-16, 0.000000000000000000 ) ) ;
#15243 = ADVANCED_FACE ( 'NONE', ( #31357 ), #9390, .T. ) ;
#15244 = EDGE_CURVE ( 'NONE', #27298, #4328, #5042, .T. ) ;
#15245 = CARTESIAN_POINT ( 'NONE',  ( 46.00000000000000000, 0.000000000000000000, 70.00000000000000000 ) ) ;
#15246 = CARTESIAN_POINT ( 'NONE',  ( 4.000000000000000000, 4.627536653468036720E-16, -22.00000000000000000 ) ) ;
#15247 = ORIENTED_EDGE ( 'NONE', *, *, #12370, .T. ) ;
#15248 = CARTESIAN_POINT ( 'NONE',  ( -38.18337828418796676, -117.0245472910329738, 2.965225545821551734 ) ) ;
#15249 = CARTESIAN_POINT ( 'NONE',  ( 8.000000000000000000, 18.62763138773856397, -2.494040418455147456 ) ) ;
#15250 = CARTESIAN_POINT ( 'NONE',  ( -35.50000000000000000, -112.9977353549762000, -0.6247823525983134951 ) ) ;
#15251 = ORIENTED_EDGE ( 'NONE', *, *, #27246, .T. ) ;
#15252 = VERTEX_POINT ( 'NONE', #12638 ) ;
#15254 = CARTESIAN_POINT ( 'NONE',  ( 0.000000000000000000, 24.72041153920790180, -40.55929306992661765 ) ) ;
#15253 = PRODUCT_DEFINITION_SHAPE ( 'NONE', 'NONE',  #27561 ) ;
#15255 = CIRCLE ( 'NONE', #21579, 52.00000000000000711 ) ;
#15256 = DIRECTION ( 'NONE',  ( -1.000000000000000000, 0.000000000000000000, 0.000000000000000000 ) ) ;
#15257 = EDGE_LOOP ( 'NONE', ( #30801, #6068 ) ) ;
#15258 = EDGE_CURVE ( 'NONE', #11298, #26946, #26138, .T. ) ;
#15259 = ORIENTED_EDGE ( 'NONE', *, *, #16541, .T. ) ;
#15260 = EDGE_CURVE ( 'NONE', #28836, #14516, #7040, .T. ) ;
#15261 = ORIENTED_EDGE ( 'NONE', *, *, #14161, .F. ) ;
#15262 = AXIS2_PLACEMENT_3D ( 'NONE', #30500, #19497, #19834 ) ;
#15263 = CIRCLE ( 'NONE', #4941, 22.00000000000000000 ) ;
#15264 = DIRECTION ( 'NONE',  ( 0.000000000000000000, 0.000000000000000000, 1.000000000000000000 ) ) ;
#15265 = CARTESIAN_POINT ( 'NONE',  ( -35.62769128460905677, -112.5438815906447729, 8.308975545821549957 ) ) ;
#15266 = LINE ( 'NONE', #23568, #17890 ) ;
#15268 = ORIENTED_EDGE ( 'NONE', *, *, #32356, .T. ) ;
#15267 = AXIS2_PLACEMENT_3D ( 'NONE', #29890, #3056, #11328 ) ;
#15269 = ORIENTED_EDGE ( 'NONE', *, *, #7218, .T. ) ;
#15270 = CARTESIAN_POINT ( 'NONE',  ( -35.50000000000000000, -111.0140978167138570, -0.4997823525984338988 ) ) ;
#15271 = CARTESIAN_POINT ( 'NONE',  ( 1.599999999999990319, 6.765000000000020997, -2.775557561562891351E-14 ) ) ;
#15272 = CARTESIAN_POINT ( 'NONE',  ( 46.00000000000000000, 0.000000000000000000, 0.000000000000000000 ) ) ;
#15273 = ORIENTED_EDGE ( 'NONE', *, *, #8633, .T. ) ;
#15274 = CARTESIAN_POINT ( 'NONE',  ( -38.00000000000000711, -114.9929510916434339, 10.50625754673587231 ) ) ;
#15275 = CARTESIAN_POINT ( 'NONE',  ( -34.50000000000000000, -114.9929510916434339, 12.60752341388803544 ) ) ;
#15276 = CIRCLE ( 'NONE', #12418, 20.00000000000000711 ) ;
#15277 = DIRECTION ( 'NONE',  ( -1.000000000000000000, 0.000000000000000000, 0.000000000000000000 ) ) ;
#15278 = CARTESIAN_POINT ( 'NONE',  ( -37.93687354226506869, -114.9929510916434339, 12.87038173996323565 ) ) ;
#15279 = DIRECTION ( 'NONE',  ( 0.000000000000000000, 0.000000000000000000, 1.000000000000000000 ) ) ;
#15280 = CARTESIAN_POINT ( 'NONE',  ( -35.24442919769867899, -113.9929510916434339, 13.92914543265605509 ) ) ;
#15281 = DIRECTION ( 'NONE',  ( 1.000000000000000000, 0.000000000000000000, -0.000000000000000000 ) ) ;
#15282 = VECTOR ( 'NONE', #28336, 1000.000000000000000 ) ;
#15283 = CARTESIAN_POINT ( 'NONE',  ( 0.000000000000000000, -19.83898331853694685, 9.508666619816580123 ) ) ;
#15284 = DIRECTION ( 'NONE',  ( -1.000000000000000000, -0.000000000000000000, 0.000000000000000000 ) ) ;
#15285 = VERTEX_POINT ( 'NONE', #1470 ) ;
#15286 = CIRCLE ( 'NONE', #35443, 7.199999999999994849 ) ;
#15287 = DIRECTION ( 'NONE',  ( -1.000000000000000000, 0.000000000000000000, 0.000000000000000000 ) ) ;
#15288 = CYLINDRICAL_SURFACE ( 'NONE', #29002, 20.00000000000000355 ) ;
#15289 = EDGE_CURVE ( 'NONE', #31693, #9081, #34606, .T. ) ;
#15290 = ORIENTED_EDGE ( 'NONE', *, *, #6279, .T. ) ;
#15291 = CARTESIAN_POINT ( 'NONE',  ( -35.50000000000000711, -114.9929510916434339, 10.51175824272318415 ) ) ;
#15292 = ORIENTED_EDGE ( 'NONE', *, *, #26992, .T. ) ;
#15293 = CARTESIAN_POINT ( 'NONE',  ( -35.62769128460905677, -115.4561184093552413, 1.691024454178448710 ) ) ;
#15294 = AXIS2_PLACEMENT_3D ( 'NONE', #13258, #35225, #10374 ) ;
#15295 = CIRCLE ( 'NONE', #28553, 3.799999999999999822 ) ;
#15296 = ORIENTED_EDGE ( 'NONE', *, *, #35040, .T. ) ;
#15297 = CYLINDRICAL_SURFACE ( 'NONE', #26252, 3.799999999999999822 ) ;
#15298 = ORIENTED_EDGE ( 'NONE', *, *, #14711, .T. ) ;
#15299 = CARTESIAN_POINT ( 'NONE',  ( -34.50000000000000000, -113.0140978167138712, 0.2502176474015764263 ) ) ;
#15300 = LINE ( 'NONE', #18006, #8126 ) ;
#15301 = CARTESIAN_POINT ( 'NONE',  ( -35.62769128460905677, -115.4561184093552413, 7.691024454178449155 ) ) ;
#15302 = ORIENTED_EDGE ( 'NONE', *, *, #20001, .T. ) ;
#15303 = CARTESIAN_POINT ( 'NONE',  ( -35.81662171581204746, -117.0245472910329738, 1.784774454178449155 ) ) ;
#15304 = CARTESIAN_POINT ( 'NONE',  ( 0.000000000000000000, 0.000000000000000000, -55.00000000000000000 ) ) ;
#15305 = VECTOR ( 'NONE', #27853, 1000.000000000000114 ) ;
#15306 = CARTESIAN_POINT ( 'NONE',  ( -35.50000000000000711, -116.0124910254613297, -0.6902086197697608894 ) ) ;
#15307 = VERTEX_POINT ( 'NONE', #34434 ) ;
#15308 = VERTEX_POINT ( 'NONE', #25965 ) ;
#15309 = CYLINDRICAL_SURFACE ( 'NONE', #26868, 20.00000000000000355 ) ;
#15310 = CIRCLE ( 'NONE', #3856, 17.49900000000001299 ) ;
#15311 = AXIS2_PLACEMENT_3D ( 'NONE', #12927, #7349, #32008 ) ;
#15312 = LINE ( 'NONE', #9925, #24208 ) ;
#15313 = ORIENTED_EDGE ( 'NONE', *, *, #19173, .F. ) ;
#15314 = ORIENTED_EDGE ( 'NONE', *, *, #16324, .T. ) ;
#15315 = CARTESIAN_POINT ( 'NONE',  ( -34.50000000000000000, -116.0140978167138712, -0.5622823525984409487 ) ) ;
#15316 = AXIS2_PLACEMENT_3D ( 'NONE', #2988, #8539, #11425 ) ;
#15317 = CARTESIAN_POINT ( 'NONE',  ( -35.50000000000000711, -112.0140978167138712, 0.6252176474015680441 ) ) ;
#15318 = CARTESIAN_POINT ( 'NONE',  ( 0.000000000000000000, 41.20225022064637699, 23.63323037071417332 ) ) ;
#15319 = EDGE_LOOP ( 'NONE', ( #20526, #1738, #23231, #17440 ) ) ;
#15320 = ORIENTED_EDGE ( 'NONE', *, *, #13047, .F. ) ;
#15321 = MECHANICAL_DESIGN_GEOMETRIC_PRESENTATION_REPRESENTATION (  '', ( #2131 ), #3272 ) ;
#15322 = CARTESIAN_POINT ( 'NONE',  ( 7.999999999999992895, -50.95304419620833158, 10.38206564895643957 ) ) ;
#15323 = CARTESIAN_POINT ( 'NONE',  ( -34.50000000000000000, -113.9697269463297431, 10.50348536859153370 ) ) ;
#15324 = LINE ( 'NONE', #20360, #19097 ) ;
#15325 = CARTESIAN_POINT ( 'NONE',  ( -35.49999931242378182, -113.9929510916434339, 12.61439929482945743 ) ) ;
#15326 = CARTESIAN_POINT ( 'NONE',  ( -35.87040530316090070, -115.9929510916434481, 13.10254527216545917 ) ) ;
#15327 = AXIS2_PLACEMENT_3D ( 'NONE', #11662, #4125, #9502 ) ;
#15328 = CARTESIAN_POINT ( 'NONE',  ( 0.000000000000000000, 0.000000000000000000, 65.00000000000000000 ) ) ;
#15329 = CARTESIAN_POINT ( 'NONE',  ( 4.000000000000000000, 6.359167119270465740, 18.96209359615096446 ) ) ;
#15330 = ADVANCED_FACE ( 'NONE', ( #9749 ), #25613, .T. ) ;
#15331 = CIRCLE ( 'NONE', #15930, 11.00000000000000000 ) ;
#15332 = ORIENTED_EDGE ( 'NONE', *, *, #24109, .F. ) ;
#15333 = LINE ( 'NONE', #12839, #27497 ) ;
#15334 = CARTESIAN_POINT ( 'NONE',  ( 0.000000000000000000, 46.21320724403665281, -10.97699764141904488 ) ) ;
#15335 = DIRECTION ( 'NONE',  ( -1.000000000000000000, 0.000000000000000000, 0.000000000000000000 ) ) ;
#15336 = AXIS2_PLACEMENT_3D ( 'NONE', #18088, #4967, #1913 ) ;
#15337 = ORIENTED_EDGE ( 'NONE', *, *, #7475, .T. ) ;
#15338 = CARTESIAN_POINT ( 'NONE',  ( 8.000000000000000000, 13.60411018104320036, 12.96676809804154118 ) ) ;
#15339 = CARTESIAN_POINT ( 'NONE',  ( -35.50000000000000711, -115.0468226098135744, -1.624774171496087716 ) ) ;
#15340 = DIRECTION ( 'NONE',  ( -1.000000000000000000, -0.000000000000000000, -0.000000000000000000 ) ) ;
#15341 = VECTOR ( 'NONE', #32679, 1000.000000000000000 ) ;
#15342 = CIRCLE ( 'NONE', #35505, 8.000000000000000000 ) ;
#15343 = EDGE_CURVE ( 'NONE', #984, #14262, #934, .T. ) ;
#15344 = CARTESIAN_POINT ( 'NONE',  ( -35.50000000000000711, -114.1189822439768449, 9.514224058074130852 ) ) ;
#15345 = CARTESIAN_POINT ( 'NONE',  ( 7.999999999999992895, -27.43636312076347394, 38.14186064215141414 ) ) ;
#15346 = ORIENTED_EDGE ( 'NONE', *, *, #17609, .F. ) ;
#15347 = DIRECTION ( 'NONE',  ( -1.000000000000000000, 0.000000000000000000, 0.000000000000000000 ) ) ;
#15348 = CARTESIAN_POINT ( 'NONE',  ( -35.50000000000000000, -113.1451905347060460, 2.905063584339864668 ) ) ;
#15349 = CARTESIAN_POINT ( 'NONE',  ( 8.000000000000007105, 0.000000000000000000, 0.000000000000000000 ) ) ;
#15350 = ORIENTED_EDGE ( 'NONE', *, *, #28492, .F. ) ;
#15351 = EDGE_LOOP ( 'NONE', ( #18267, #31303, #19129, #26634 ) ) ;
#15352 = CARTESIAN_POINT ( 'NONE',  ( -37.05926240293133134, -115.0000000000000000, 4.878524454178448266 ) ) ;
#15353 = AXIS2_PLACEMENT_3D ( 'NONE', #23859, #10173, #7636 ) ;
#15354 = EDGE_LOOP ( 'NONE', ( #35399, #25381, #28991, #16143 ) ) ;
#15355 = ORIENTED_EDGE ( 'NONE', *, *, #11299, .T. ) ;
#15356 = CARTESIAN_POINT ( 'NONE',  ( -35.50000000000000000, -115.0140978167137860, -0.6411448143358557950 ) ) ;
#15357 = VECTOR ( 'NONE', #18305, 999.9999999999998863 ) ;
#15358 = DIRECTION ( 'NONE',  ( -0.000000000000000000, 0.000000000000000000, -1.000000000000000000 ) ) ;
#15359 = AXIS2_PLACEMENT_3D ( 'NONE', #21782, #8099, #10098 ) ;
#15360 = CARTESIAN_POINT ( 'NONE',  ( 0.000000000000000000, -38.92705108641712286, -27.21837053747841395 ) ) ;
#15361 = AXIS2_PLACEMENT_3D ( 'NONE', #34241, #4014, #20542 ) ;
#15362 = CARTESIAN_POINT ( 'NONE',  ( -35.50000000000000000, -113.9917898843777522, 10.50611893782865813 ) ) ;
#15363 = LINE ( 'NONE', #15015, #27628 ) ;
#15364 = AXIS2_PLACEMENT_3D ( 'NONE', #22748, #3342, #14638 ) ;
#15365 = CARTESIAN_POINT ( 'NONE',  ( -36.03906250000000000, -114.9929510916434339, 14.11852480586264846 ) ) ;
#15366 = CARTESIAN_POINT ( 'NONE',  ( 8.000000000000000000, 16.59870953437680896, 3.253005020243904255 ) ) ;
#15367 = EDGE_CURVE ( 'NONE', #2175, #1839, #33792, .T. ) ;
#15368 = EDGE_CURVE ( 'NONE', #26302, #15547, #33883, .T. ) ;
#15369 = DIRECTION ( 'NONE',  ( 0.000000000000000000, 0.000000000000000000, 1.000000000000000000 ) ) ;
#15370 = ORIENTED_EDGE ( 'NONE', *, *, #35407, .F. ) ;
#15371 = CARTESIAN_POINT ( 'NONE',  ( -35.99181955245763476, -115.9929510916434481, 13.11847460610632510 ) ) ;
#15372 = CARTESIAN_POINT ( 'NONE',  ( -35.50000000000000711, -116.0140978167138712, 0.3752176474015736507 ) ) ;
#15373 = DIRECTION ( 'NONE',  ( 0.000000000000000000, -1.000000000000000000, -1.047252562447196865E-14 ) ) ;
#15374 = DIRECTION ( 'NONE',  ( 0.000000000000000000, 0.000000000000000000, 1.000000000000000000 ) ) ;
#15375 = ORIENTED_EDGE ( 'NONE', *, *, #11387, .F. ) ;
#15376 = FACE_OUTER_BOUND ( 'NONE', #25295, .T. ) ;
#15377 = DIRECTION ( 'NONE',  ( 0.000000000000000000, 0.000000000000000000, -1.000000000000000000 ) ) ;
#15378 = AXIS2_PLACEMENT_3D ( 'NONE', #28988, #27011, #34754 ) ;
#15379 = CARTESIAN_POINT ( 'NONE',  ( -34.49999999999998579, -25.98076211353322051, 84.99999999999992895 ) ) ;
#15380 = CYLINDRICAL_SURFACE ( 'NONE', #10923, 8.000000000000001776 ) ;
#15381 = ORIENTED_EDGE ( 'NONE', *, *, #15388, .F. ) ;
#15382 = AXIS2_PLACEMENT_3D ( 'NONE', #5396, #18700, #15992 ) ;
#15383 = EDGE_CURVE ( 'NONE', #32804, #31713, #3321, .T. ) ;
#15384 = CARTESIAN_POINT ( 'NONE',  ( -36.64504884055823908, -115.0245472910329880, 7.784774454178449155 ) ) ;
#15385 = CARTESIAN_POINT ( 'NONE',  ( 0.000000000000000000, 16.53603053422208902, -8.931325931664652273 ) ) ;
#15386 = CIRCLE ( 'NONE', #19979, 47.49900000000001654 ) ;
#15387 = CARTESIAN_POINT ( 'NONE',  ( 3.799999999999999822, -2.710505431213761085E-17, 45.10000000000000142 ) ) ;
#15388 = EDGE_CURVE ( 'NONE', #28924, #28609, #25257, .T. ) ;
#15389 = EDGE_LOOP ( 'NONE', ( #23654, #19487, #17666, #26817 ) ) ;
#15390 = ORIENTED_EDGE ( 'NONE', *, *, #8629, .T. ) ;
#15391 = AXIS2_PLACEMENT_3D ( 'NONE', #16514, #3034, #32915 ) ;
#15392 = DIRECTION ( 'NONE',  ( -1.783119874454246424E-31, -1.187911941725854497E-31, 1.000000000000000000 ) ) ;
#15393 = CARTESIAN_POINT ( 'NONE',  ( 7.999999999999992895, 5.667686777402359155, -46.64153600743598105 ) ) ;
#15394 = ORIENTED_EDGE ( 'NONE', *, *, #23998, .T. ) ;
#15395 = CARTESIAN_POINT ( 'NONE',  ( -36.94073759706868287, -115.9999999999999858, 2.871475545821551290 ) ) ;
#15396 = ORIENTED_EDGE ( 'NONE', *, *, #17238, .F. ) ;
#15397 = VECTOR ( 'NONE', #3595, 1000.000000000000000 ) ;
#15398 = CARTESIAN_POINT ( 'NONE',  ( 0.000000000000000000, -47.32430374665916872, -21.55018039121578255 ) ) ;
#15399 = ORIENTED_EDGE ( 'NONE', *, *, #14136, .T. ) ;
#15400 = CARTESIAN_POINT ( 'NONE',  ( 7.999999999999992895, 49.65209126885763879, 15.44894276735568539 ) ) ;
#15401 = CARTESIAN_POINT ( 'NONE',  ( 7.999999999999992895, 0.000000000000000000, 0.000000000000000000 ) ) ;
#15402 = EDGE_CURVE ( 'NONE', #23525, #33336, #32042, .T. ) ;
#15403 = DIRECTION ( 'NONE',  ( 1.000000000000000000, 0.000000000000000000, 0.000000000000000000 ) ) ;
#15404 = VERTEX_POINT ( 'NONE', #2018 ) ;
#15405 = VERTEX_POINT ( 'NONE', #1842 ) ;
#15406 = CYLINDRICAL_SURFACE ( 'NONE', #35218, 4.800000000000000711 ) ;
#15407 = PLANE ( 'NONE',  #35065 ) ;
#15408 = VECTOR ( 'NONE', #29110, 1000.000000000000000 ) ;
#15409 = ORIENTED_EDGE ( 'NONE', *, *, #11636, .T. ) ;
#15410 = DIRECTION ( 'NONE',  ( 1.000000000000000000, -0.000000000000000000, -0.000000000000000000 ) ) ;
#15411 = AXIS2_PLACEMENT_3D ( 'NONE', #27307, #22068, #30182 ) ;
#15412 = DIRECTION ( 'NONE',  ( 0.000000000000000000, 0.000000000000000000, 1.000000000000000000 ) ) ;
#15413 = DIRECTION ( 'NONE',  ( 0.000000000000000000, 0.000000000000000000, 1.000000000000000000 ) ) ;
#15414 = AXIS2_PLACEMENT_3D ( 'NONE', #18785, #31982, #18963 ) ;
#15415 = CARTESIAN_POINT ( 'NONE',  ( -34.54793860109200665, -115.9929510916434481, 13.00730889637958221 ) ) ;
#15416 = ADVANCED_FACE ( 'NONE', ( #10470 ), #23977, .T. ) ;
#15417 = EDGE_CURVE ( 'NONE', #16883, #688, #15939, .T. ) ;
#15418 = CARTESIAN_POINT ( 'NONE',  ( 8.000000000000000000, -13.60411018104326963, 12.96676809804144348 ) ) ;
#15419 = CARTESIAN_POINT ( 'NONE',  ( -38.99999999999999289, -113.9407375970686900, 6.753524454178448266 ) ) ;
#15420 = ADVANCED_FACE ( 'NONE', ( #10644 ), #2558, .T. ) ;
#15421 = CARTESIAN_POINT ( 'NONE',  ( -34.50000000000000000, -115.9929510916434481, 12.59102132592610346 ) ) ;
#15422 = CARTESIAN_POINT ( 'NONE',  ( 7.999999999999992895, 0.000000000000000000, 0.000000000000000000 ) ) ;
#15423 = CARTESIAN_POINT ( 'NONE',  ( -34.49999999999998579, -3.784235812937200460, 96.08311962715481513 ) ) ;
#15424 = DIRECTION ( 'NONE',  ( -1.000000000000000000, 0.000000000000000000, 0.000000000000000000 ) ) ;
#15425 = DIRECTION ( 'NONE',  ( 1.000000000000000000, 1.734723475976807094E-16, 0.000000000000000000 ) ) ;
#15426 = DIRECTION ( 'NONE',  ( 1.000000000000000000, -0.000000000000000000, 0.000000000000000000 ) ) ;
#15427 = ORIENTED_EDGE ( 'NONE', *, *, #28355, .F. ) ;
#15428 = CARTESIAN_POINT ( 'NONE',  ( -38.45611840935523418, -112.6276912846090568, 3.433975545821551290 ) ) ;
#15429 = CARTESIAN_POINT ( 'NONE',  ( -50.00000000000000000, -25.98076211353320275, 84.99999999999992895 ) ) ;
#15430 = CARTESIAN_POINT ( 'NONE',  ( -35.50000000000000000, -113.0140978167143260, -0.6247823525984285142 ) ) ;
#15431 = EDGE_CURVE ( 'NONE', #7438, #32535, #24602, .T. ) ;
#15432 = ORIENTED_EDGE ( 'NONE', *, *, #21312, .F. ) ;
#15433 = ORIENTED_EDGE ( 'NONE', *, *, #8269, .T. ) ;
#15434 = PRESENTATION_STYLE_ASSIGNMENT (( #34727 ) ) ;
#15435 = DIRECTION ( 'NONE',  ( -1.000000000000000000, -0.000000000000000000, 0.000000000000000000 ) ) ;
#15436 = ORIENTED_EDGE ( 'NONE', *, *, #21195, .F. ) ;
#15437 = AXIS2_PLACEMENT_3D ( 'NONE', #16648, #26235, #1937 ) ;
#15438 = VERTEX_POINT ( 'NONE', #20885 ) ;
#15439 = ORIENTED_EDGE ( 'NONE', *, *, #34749, .T. ) ;
#15440 = AXIS2_PLACEMENT_3D ( 'NONE', #4065, #15012, #17891 ) ;
#15441 = FACE_OUTER_BOUND ( 'NONE', #2010, .T. ) ;
#15442 = CARTESIAN_POINT ( 'NONE',  ( 0.000000000000000000, 47.22458491092828581, -5.098390039073752433 ) ) ;
#15443 = CARTESIAN_POINT ( 'NONE',  ( 0.000000000000000000, 0.000000000000000000, 0.000000000000000000 ) ) ;
#15444 = EDGE_CURVE ( 'NONE', #33885, #29327, #29766, .T. ) ;
#15445 = CARTESIAN_POINT ( 'NONE',  ( 0.000000000000000000, 4.898587196589412829E-16, -4.000000000000000000 ) ) ;
#15446 = ORIENTED_EDGE ( 'NONE', *, *, #4602, .T. ) ;
#15447 = ORIENTED_EDGE ( 'NONE', *, *, #6823, .T. ) ;
#15448 = CARTESIAN_POINT ( 'NONE',  ( -35.50000000000000711, -112.0140978167138712, -0.3747823525984256832 ) ) ;
#15449 = EDGE_CURVE ( 'NONE', #33861, #423, #33199, .T. ) ;
#15450 = CARTESIAN_POINT ( 'NONE',  ( -34.49999999999998579, -31.64142946139417134, 97.80456345124110840 ) ) ;
#15451 = LINE ( 'NONE', #26467, #25288 ) ;
#15452 = VERTEX_POINT ( 'NONE', #32601 ) ;
#15453 = DIRECTION ( 'NONE',  ( -4.662936703425629071E-15, 1.000000000000000000, -4.222049128630314618E-16 ) ) ;
#15454 = CARTESIAN_POINT ( 'NONE',  ( -34.50000000000000000, -112.4434344552011282, 1.705278471174987986 ) ) ;
#15455 = CARTESIAN_POINT ( 'NONE',  ( -34.50000000000000000, -114.9929517792218689, 10.50900788599415314 ) ) ;
#15456 = DIRECTION ( 'NONE',  ( -1.000000000000000000, 0.000000000000000000, 0.000000000000000000 ) ) ;
#15457 = ADVANCED_FACE ( 'NONE', ( #21070 ), #27037, .T. ) ;
#15458 = CIRCLE ( 'NONE', #21227, 11.00000000000000000 ) ;
#15459 = CARTESIAN_POINT ( 'NONE',  ( -36.62499999999902656, -114.9929510916434339, 13.11852480586264669 ) ) ;
#15460 = CARTESIAN_POINT ( 'NONE',  ( 4.000000000000003553, 44.25018368420781911, -27.31155879685134735 ) ) ;
#15461 = EDGE_CURVE ( 'NONE', #2204, #32025, #27487, .T. ) ;
#15462 = CARTESIAN_POINT ( 'NONE',  ( -34.50000000000000000, -114.5636144531578680, 9.676196722963288366 ) ) ;
#15463 = DIRECTION ( 'NONE',  ( 0.000000000000000000, 0.000000000000000000, 1.000000000000000000 ) ) ;
#15464 = CARTESIAN_POINT ( 'NONE',  ( -37.58145695302688694, -114.9929510916434339, 13.11211614918362756 ) ) ;
#15465 = VERTEX_POINT ( 'NONE', #7408 ) ;
#15466 = AXIS2_PLACEMENT_3D ( 'NONE', #20896, #15142, #20554 ) ;
#15467 = LINE ( 'NONE', #20688, #23909 ) ;
#15468 = CARTESIAN_POINT ( 'NONE',  ( -37.49999999999999289, -11.52052244843579309, 115.1848168619253698 ) ) ;
#15469 = EDGE_LOOP ( 'NONE', ( #33638, #9351 ) ) ;
#15470 = CARTESIAN_POINT ( 'NONE',  ( -36.50000000000011369, -114.9929510916434339, 13.11852480586264669 ) ) ;
#15471 = ORIENTED_EDGE ( 'NONE', *, *, #6213, .F. ) ;
#15472 = VECTOR ( 'NONE', #4491, 1000.000000000000000 ) ;
#15473 = CARTESIAN_POINT ( 'NONE',  ( -38.45611840935523418, -115.3723087153909432, 3.566024454178448710 ) ) ;
#15474 = AXIS2_PLACEMENT_3D ( 'NONE', #4152, #32037, #17447 ) ;
#15475 = CARTESIAN_POINT ( 'NONE',  ( 0.000000000000000000, -13.56094713063537327, -50.20060470671755581 ) ) ;
#15476 = ORIENTED_EDGE ( 'NONE', *, *, #11929, .T. ) ;
#15477 = DIRECTION ( 'NONE',  ( 1.000000000000000000, -0.000000000000000000, -0.000000000000000000 ) ) ;
#15478 = ORIENTED_EDGE ( 'NONE', *, *, #26638, .F. ) ;
#15479 = CARTESIAN_POINT ( 'NONE',  ( -34.50000000000000000, -113.0140978167136581, -0.6247823525984261828 ) ) ;
#15480 = CARTESIAN_POINT ( 'NONE',  ( 8.000000000000000000, -19.77827456857333743, -2.969824084036674527 ) ) ;
#15481 = DIRECTION ( 'NONE',  ( 0.02040816326530611735, -0.9997917317482359900, 1.302694377452200301E-31 ) ) ;
#15482 = VERTEX_POINT ( 'NONE', #7219 ) ;
#15483 = CARTESIAN_POINT ( 'NONE',  ( -39.02454729103295961, -114.7691647218148745, 8.159774454178448266 ) ) ;
#15484 = CARTESIAN_POINT ( 'NONE',  ( 2.321707774797385326, -4.824281976788927118, -0.7999999999999951594 ) ) ;
#15485 = CARTESIAN_POINT ( 'NONE',  ( -35.50000000000000711, -116.0140978167138712, -0.1247823525984439463 ) ) ;
#15486 = ORIENTED_EDGE ( 'NONE', *, *, #5738, .T. ) ;
#15487 = ORIENTED_EDGE ( 'NONE', *, *, #18141, .T. ) ;
#15488 = CARTESIAN_POINT ( 'NONE',  ( 0.000000000000000000, 18.62763138773855687, 2.494040418455418351 ) ) ;
#15489 = CIRCLE ( 'NONE', #20672, 5.000000000000011546 ) ;
#15490 = EDGE_CURVE ( 'NONE', #21171, #30484, #35526, .T. ) ;
#15491 = DIRECTION ( 'NONE',  ( -1.000000000000000000, 0.000000000000000000, 0.000000000000000000 ) ) ;
#15492 = ORIENTED_EDGE ( 'NONE', *, *, #17218, .T. ) ;
#15493 = VERTEX_POINT ( 'NONE', #181 ) ;
#15494 = VECTOR ( 'NONE', #5223, 1000.000000000000000 ) ;
#15495 = CARTESIAN_POINT ( 'NONE',  ( -34.50000000000000000, -115.8878449012421754, -1.128496220799388494 ) ) ;
#15496 = EDGE_CURVE ( 'NONE', #34524, #31265, #25389, .T. ) ;
#15497 = FACE_OUTER_BOUND ( 'NONE', #20674, .T. ) ;
#15498 = PRODUCT_DEFINITION_FORMATION_WITH_SPECIFIED_SOURCE ( 'ANY', '', #31947, .NOT_KNOWN. ) ;
#15499 = ORIENTED_EDGE ( 'NONE', *, *, #9054, .F. ) ;
#15500 = ORIENTED_EDGE ( 'NONE', *, *, #33042, .F. ) ;
#15501 = AXIS2_PLACEMENT_3D ( 'NONE', #24410, #4976, #29639 ) ;
#15502 = FACE_OUTER_BOUND ( 'NONE', #987, .T. ) ;
#15503 = CARTESIAN_POINT ( 'NONE',  ( -38.00000000000000711, -113.9929510916434339, 12.53051367006571937 ) ) ;
#15504 = CARTESIAN_POINT ( 'NONE',  ( 4.000000000000003553, -21.63912866391140710, 3.968388925834730685 ) ) ;
#15505 = CARTESIAN_POINT ( 'NONE',  ( -34.50000000000000000, -113.8814751941377352, 10.49295109164313722 ) ) ;
#15506 = CARTESIAN_POINT ( 'NONE',  ( -37.97447287825094264, -115.9929510916434481, 12.77960891308616809 ) ) ;
#15507 = DIRECTION ( 'NONE',  ( -1.000000000000000000, 0.000000000000000000, 0.000000000000000000 ) ) ;
#15508 = CARTESIAN_POINT ( 'NONE',  ( 4.000000000000000000, 4.898587196589412829E-16, -53.39999999999999858 ) ) ;
#15509 = VERTEX_POINT ( 'NONE', #8463 ) ;
#15510 = CIRCLE ( 'NONE', #6325, 20.00000000000000000 ) ;
#15511 = DIRECTION ( 'NONE',  ( -1.000000000000000000, 0.000000000000000000, 0.000000000000000000 ) ) ;
#15512 = CARTESIAN_POINT ( 'NONE',  ( 0.000000000000000000, 0.000000000000000000, 0.000000000000000000 ) ) ;
#15513 = CARTESIAN_POINT ( 'NONE',  ( -4.000000000000000000, -2.710505431213761085E-17, 29.09999999999999787 ) ) ;
#15514 = ORIENTED_EDGE ( 'NONE', *, *, #14845, .T. ) ;
#15515 = CIRCLE ( 'NONE', #20108, 12.99999999999999467 ) ;
#15516 = DIRECTION ( 'NONE',  ( -1.000000000000000000, 0.000000000000000000, 0.000000000000000000 ) ) ;
#15517 = CARTESIAN_POINT ( 'NONE',  ( -35.50000000000000711, -112.0250551866464548, 1.025914454044489332 ) ) ;
#15518 = DIRECTION ( 'NONE',  ( -1.000000000000000000, 0.000000000000000000, 0.000000000000000000 ) ) ;
#15519 = VECTOR ( 'NONE', #23870, 1000.000000000000000 ) ;
#15520 = CIRCLE ( 'NONE', #6336, 9.499000000000009436 ) ;
#15521 = CARTESIAN_POINT ( 'NONE',  ( -35.50000000000000711, -114.1861579685891712, 9.524983039397698192 ) ) ;
#15522 = CARTESIAN_POINT ( 'NONE',  ( 0.000000000000000000, -2.710505431213761085E-17, 55.00000000000000000 ) ) ;
#15523 = VERTEX_POINT ( 'NONE', #10828 ) ;
#15524 = CARTESIAN_POINT ( 'NONE',  ( 0.000000000000000000, 51.93417535146742381, 2.615612846549361770 ) ) ;
#15525 = CARTESIAN_POINT ( 'NONE',  ( -34.50000000000000000, -113.8474311500459777, -2.624782352598442614 ) ) ;
#15526 = LINE ( 'NONE', #1880, #28957 ) ;
#15527 = ORIENTED_EDGE ( 'NONE', *, *, #32670, .F. ) ;
#15528 = ORIENTED_EDGE ( 'NONE', *, *, #6405, .T. ) ;
#15529 = CARTESIAN_POINT ( 'NONE',  ( -37.66520193420439000, -113.2509883718312977, 6.941024454178450043 ) ) ;
#15530 = FACE_OUTER_BOUND ( 'NONE', #28077, .T. ) ;
#15531 = ORIENTED_EDGE ( 'NONE', *, *, #22650, .F. ) ;
#15532 = ORIENTED_EDGE ( 'NONE', *, *, #10478, .F. ) ;
#15533 = CARTESIAN_POINT ( 'NONE',  ( -34.50000000000000000, -112.9990795116828650, 0.8734249692896993711 ) ) ;
#15534 = SHAPE_REPRESENTATION ( 'shaft', ( #21307 ), #24262 ) ;
#15535 = EDGE_CURVE ( 'NONE', #13123, #12814, #5773, .T. ) ;
#15536 = AXIS2_PLACEMENT_3D ( 'NONE', #30667, #25085, #413 ) ;
#15537 = CARTESIAN_POINT ( 'NONE',  ( 3.799999999999999822, 4.653657836759942730E-16, -39.50000000000000711 ) ) ;
#15538 = CARTESIAN_POINT ( 'NONE',  ( 8.000000000000000000, 0.000000000000000000, 0.000000000000000000 ) ) ;
#15539 = CARTESIAN_POINT ( 'NONE',  ( -37.80727372874345349, -114.9929510916434339, 13.01835785830664527 ) ) ;
#15540 = CARTESIAN_POINT ( 'NONE',  ( -2.141980652367370119, -6.189445006155602336, -0.7999999999999951594 ) ) ;
#15541 = EDGE_CURVE ( 'NONE', #1868, #19467, #30442, .T. ) ;
#15542 = CIRCLE ( 'NONE', #34544, 9.499000000000000554 ) ;
#15543 = CARTESIAN_POINT ( 'NONE',  ( -35.75562914091914024, -114.9929510916434339, 14.09929883582542409 ) ) ;
#15544 = CARTESIAN_POINT ( 'NONE',  ( 8.000000000000000000, 0.000000000000000000, 0.000000000000000000 ) ) ;
#15545 = PRODUCT ( 'shaft', 'shaft', '', ( #28755 ) ) ;
#15546 = CYLINDRICAL_SURFACE ( 'NONE', #11718, 20.00000000000000355 ) ;
#15547 = VERTEX_POINT ( 'NONE', #22317 ) ;
#15548 = CARTESIAN_POINT ( 'NONE',  ( -35.87040530316090070, -115.9929510916434481, 13.10254527216545917 ) ) ;
#15549 = DIRECTION ( 'NONE',  ( 0.000000000000000000, -0.8660254037844432595, 0.4999999999999920619 ) ) ;
#15550 = CARTESIAN_POINT ( 'NONE',  ( 0.000000000000000000, -14.18878633068154826, -6.236773481718229206 ) ) ;
#15551 = CARTESIAN_POINT ( 'NONE',  ( 8.000000000000000000, -8.931325931664478190, -16.53603053422218494 ) ) ;
#15552 = CARTESIAN_POINT ( 'NONE',  ( 0.000000000000000000, -18.48663108841356717, -3.384281271888017084 ) ) ;
#15553 = EDGE_LOOP ( 'NONE', ( #3791, #28036, #34488, #6651 ) ) ;
#15554 = LINE ( 'NONE', #4087, #27990 ) ;
#15555 = PLANE ( 'NONE',  #21014 ) ;
#15556 = CYLINDRICAL_SURFACE ( 'NONE', #15336, 20.00000000000000355 ) ;
#15557 = DIRECTION ( 'NONE',  ( -0.000000000000000000, 0.000000000000000000, -1.000000000000000000 ) ) ;
#15558 = ORIENTED_EDGE ( 'NONE', *, *, #28400, .F. ) ;
#15559 = CARTESIAN_POINT ( 'NONE',  ( -37.05926240293133134, -115.0000000000000000, 3.378524454178448710 ) ) ;
#15560 = CARTESIAN_POINT ( 'NONE',  ( -39.49999999999999289, -15.63316754279159326, 121.0048025873809792 ) ) ;
#15561 = CYLINDRICAL_SURFACE ( 'NONE', #30854, 3.799999999999999822 ) ;
#15562 = ORIENTED_EDGE ( 'NONE', *, *, #19417, .T. ) ;
#15563 = VERTEX_POINT ( 'NONE', #30261 ) ;
#15564 = CARTESIAN_POINT ( 'NONE',  ( -49.99999999999999289, -25.98076211353320275, 84.99999999999992895 ) ) ;
#15565 = LINE ( 'NONE', #5161, #24992 ) ;
#15566 = ORIENTED_EDGE ( 'NONE', *, *, #10478, .T. ) ;
#15567 = CARTESIAN_POINT ( 'NONE',  ( -35.00000000000000000, -113.9407375970686900, 2.496475545821551290 ) ) ;
#15568 = ORIENTED_EDGE ( 'NONE', *, *, #21852, .F. ) ;
#15569 = CIRCLE ( 'NONE', #4719, 13.99999999999999645 ) ;
#15570 = STYLED_ITEM ( 'NONE', ( #5295 ), #1766 ) ;
#15571 = VERTEX_POINT ( 'NONE', #8102 ) ;
#15572 = EDGE_LOOP ( 'NONE', ( #32119, #10020, #17080, #29330 ) ) ;
#15573 = CYLINDRICAL_SURFACE ( 'NONE', #7946, 14.70000000000000107 ) ;
#15574 = EDGE_CURVE ( 'NONE', #22574, #13336, #10792, .T. ) ;
#15575 = ADVANCED_FACE ( 'NONE', ( #5601 ), #28092, .T. ) ;
#15576 = LINE ( 'NONE', #12731, #29454 ) ;
#15577 = VERTEX_POINT ( 'NONE', #16564 ) ;
#15578 = ORIENTED_EDGE ( 'NONE', *, *, #26164, .T. ) ;
#15579 = DIRECTION ( 'NONE',  ( 0.000000000000000000, 0.000000000000000000, 1.000000000000000000 ) ) ;
#15580 = CARTESIAN_POINT ( 'NONE',  ( -12.55910585664919132, 0.7408941433508802188, -1.200000000000006617 ) ) ;
#15581 = EDGE_CURVE ( 'NONE', #24282, #16219, #13095, .T. ) ;
#15582 = ORIENTED_EDGE ( 'NONE', *, *, #34853, .F. ) ;
#15583 = CARTESIAN_POINT ( 'NONE',  ( 55.00000000000000000, -2.775557561562891351E-14, 110.0000000000000000 ) ) ;
#15584 = CARTESIAN_POINT ( 'NONE',  ( -38.50000000000000711, -114.9929510916434339, 10.50625754673587231 ) ) ;
#15585 = DIRECTION ( 'NONE',  ( 1.000000000000000000, 0.000000000000000000, 0.000000000000000000 ) ) ;
#15586 = CARTESIAN_POINT ( 'NONE',  ( -34.50000000000000000, -115.9929510916434481, 11.73841344789270202 ) ) ;
#15587 = FACE_OUTER_BOUND ( 'NONE', #22876, .T. ) ;
#15588 = CARTESIAN_POINT ( 'NONE',  ( -37.05926240293131713, -115.9999999999999858, 7.878524454178450043 ) ) ;
#15589 = CIRCLE ( 'NONE', #2426, 8.000000000000051514 ) ;
#15590 = CARTESIAN_POINT ( 'NONE',  ( -34.50000000000000000, -115.9710363517788068, 10.20486393345008835 ) ) ;
#15592 = CARTESIAN_POINT ( 'NONE',  ( -26.99999999999999289, 3.122849337825751800E-15, 0.000000000000000000 ) ) ;
#15591 = AXIS2_PLACEMENT_3D ( 'NONE', #22982, #1037, #6255 ) ;
#15593 = DIRECTION ( 'NONE',  ( 0.000000000000000000, 0.9848077530122085754, -0.1736481776669275556 ) ) ;
#15594 = CARTESIAN_POINT ( 'NONE',  ( -9.999999999999994671, 0.000000000000000000, 0.000000000000000000 ) ) ;
#15595 = PLANE ( 'NONE',  #14637 ) ;
#15596 = CARTESIAN_POINT ( 'NONE',  ( -39.49999999999999289, -4.676198662292047281, 104.0227405789415798 ) ) ;
#15597 = PRESENTATION_STYLE_ASSIGNMENT (( #24270 ) ) ;
#15598 = ORIENTED_EDGE ( 'NONE', *, *, #27389, .T. ) ;
#15599 = CARTESIAN_POINT ( 'NONE',  ( -35.54388159064475872, -115.3723087153909432, 2.683975545821551290 ) ) ;
#15600 = LINE ( 'NONE', #15968, #25597 ) ;
#15601 = EDGE_CURVE ( 'NONE', #2787, #32375, #32634, .T. ) ;
#15602 = CARTESIAN_POINT ( 'NONE',  ( -35.50000000000000000, -113.2441867727860227, 0.9026824934337903672 ) ) ;
#15603 = ORIENTED_EDGE ( 'NONE', *, *, #35222, .T. ) ;
#15604 = VERTEX_POINT ( 'NONE', #3080 ) ;
#15605 = LINE ( 'NONE', #34374, #24044 ) ;
#15606 = DIRECTION ( 'NONE',  ( 0.000000000000000000, 0.8660254037844362651, 0.5000000000000041078 ) ) ;
#15607 = VERTEX_POINT ( 'NONE', #27572 ) ;
#15608 = VERTEX_POINT ( 'NONE', #6114 ) ;
#15609 = ORIENTED_EDGE ( 'NONE', *, *, #20245, .T. ) ;
#15610 = EDGE_CURVE ( 'NONE', #11168, #4839, #17088, .T. ) ;
#15611 = CARTESIAN_POINT ( 'NONE',  ( 7.999999999999992895, 10.58300524425836109, -3.000000000000002665 ) ) ;
#15612 = EDGE_CURVE ( 'NONE', #25092, #20425, #2908, .T. ) ;
#15613 = CARTESIAN_POINT ( 'NONE',  ( -0.6000000000000037526, -12.74999999999999822, -1.691777834109591940E-31 ) ) ;
#15614 = ADVANCED_FACE ( 'NONE', ( #3435 ), #19086, .T. ) ;
#15615 = VECTOR ( 'NONE', #20268, 1000.000000000000000 ) ;
#15616 = AXIS2_PLACEMENT_3D ( 'NONE', #22403, #24781, #3359 ) ;
#15617 = DIRECTION ( 'NONE',  ( 0.000000000000000000, 0.000000000000000000, -1.000000000000000000 ) ) ;
#15618 = DIRECTION ( 'NONE',  ( 0.000000000000000000, 1.000000000000000000, 3.469446951953613400E-15 ) ) ;
#15619 = ORIENTED_EDGE ( 'NONE', *, *, #13022, .F. ) ;
#15620 = ORIENTED_EDGE ( 'NONE', *, *, #29873, .T. ) ;
#15621 = CARTESIAN_POINT ( 'NONE',  ( -35.50000000000000711, -112.0269151300720409, -0.7876962586524208776 ) ) ;
#15622 =( REPRESENTATION_RELATIONSHIP ('NONE','NONE', #26607, #1790 ) REPRESENTATION_RELATIONSHIP_WITH_TRANSFORMATION ( #14108 )SHAPE_REPRESENTATION_RELATIONSHIP( ) );
#15623 = FACE_OUTER_BOUND ( 'NONE', #840, .T. ) ;
#15624 = EDGE_CURVE ( 'NONE', #24598, #2557, #17662, .T. ) ;
#15625 = DIRECTION ( 'NONE',  ( -1.000000000000000000, -0.000000000000000000, -0.000000000000000000 ) ) ;
#15626 = ORIENTED_EDGE ( 'NONE', *, *, #34064, .T. ) ;
#15627 = CARTESIAN_POINT ( 'NONE',  ( 7.999999999999992895, 36.05989434073656241, -30.12041790338579261 ) ) ;
#15628 = EDGE_CURVE ( 'NONE', #6999, #26953, #16504, .T. ) ;
#15629 = VECTOR ( 'NONE', #24577, 1000.000000000000000 ) ;
#15630 = CARTESIAN_POINT ( 'NONE',  ( -39.49999999999999289, 9.432411113711806294, 117.4309090467819772 ) ) ;
#15631 = CARTESIAN_POINT ( 'NONE',  ( -34.50000000000000000, -114.8847986568751907, 10.03799953695244618 ) ) ;
#15632 = LINE ( 'NONE', #21753, #19976 ) ;
#15633 = CARTESIAN_POINT ( 'NONE',  ( -36.01562499999996447, -114.9929510916434339, 13.11852480586264669 ) ) ;
#15634 = DIRECTION ( 'NONE',  ( 0.000000000000000000, -0.5877852522924803536, 0.8090169943749422332 ) ) ;
#15635 = CARTESIAN_POINT ( 'NONE',  ( -34.50000000000000000, -114.6604609523327838, 9.751889438017201428 ) ) ;
#15636 = DIRECTION ( 'NONE',  ( 1.000000000000000000, 0.000000000000000000, 0.000000000000000000 ) ) ;
#15637 = CARTESIAN_POINT ( 'NONE',  ( -37.99999897736218202, -114.9929510916434339, 12.62466071271732915 ) ) ;
#15638 = DIRECTION ( 'NONE',  ( 0.000000000000000000, -0.9929510916431035783, 0.1185248058626076212 ) ) ;
#15639 = ORIENTED_EDGE ( 'NONE', *, *, #35414, .F. ) ;
#15640 = DIRECTION ( 'NONE',  ( 0.000000000000000000, -1.000000000000000000, 0.000000000000000000 ) ) ;
#15641 = DIRECTION ( 'NONE',  ( -1.000000000000000000, -0.000000000000000000, -0.000000000000000000 ) ) ;
#15642 = EDGE_LOOP ( 'NONE', ( #34144, #35223, #23686, #8069 ) ) ;
#15643 = AXIS2_PLACEMENT_3D ( 'NONE', #23995, #27406, #16205 ) ;
#15644 = CARTESIAN_POINT ( 'NONE',  ( -37.99959864031215773, -114.9929510916434339, 12.63896776382213538 ) ) ;
#15645 = ORIENTED_EDGE ( 'NONE', *, *, #32661, .T. ) ;
#15646 = VECTOR ( 'NONE', #26402, 1000.000000000000000 ) ;
#15647 = CIRCLE ( 'NONE', #34073, 17.49900000000001654 ) ;
#15648 = CARTESIAN_POINT ( 'NONE',  ( -36.11231047232249125, -112.0245472910329880, 7.222274454178451819 ) ) ;
#15649 = DIRECTION ( 'NONE',  ( 0.000000000000000000, 1.000000000000000000, 1.224646799147353207E-16 ) ) ;
#15650 = EDGE_CURVE ( 'NONE', #4059, #966, #32960, .T. ) ;
#15651 = ORIENTED_EDGE ( 'NONE', *, *, #7955, .F. ) ;
#15652 = ORIENTED_EDGE ( 'NONE', *, *, #20955, .T. ) ;
#15653 = EDGE_CURVE ( 'NONE', #31530, #10826, #2180, .T. ) ;
#15654 = LINE ( 'NONE', #18549, #9979 ) ;
#15655 = ADVANCED_FACE ( 'NONE', ( #16373 ), #10995, .T. ) ;
#15656 = ORIENTED_EDGE ( 'NONE', *, *, #10617, .F. ) ;
#15657 = CARTESIAN_POINT ( 'NONE',  ( -37.05926240293133134, -116.9999999999999858, 1.878524454178448710 ) ) ;
#15658 = AXIS2_PLACEMENT_3D ( 'NONE', #15271, #21220, #18520 ) ;
#15659 = AXIS2_PLACEMENT_3D ( 'NONE', #11787, #19532, #13970 ) ;
#15660 = CARTESIAN_POINT ( 'NONE',  ( 0.000000000000000000, -2.710505431213761085E-17, -45.89999999999999858 ) ) ;
#15661 = CARTESIAN_POINT ( 'NONE',  ( 4.000000000000000000, 4.627536653468036720E-16, -21.89999999999999858 ) ) ;
#15662 = ORIENTED_EDGE ( 'NONE', *, *, #9948, .F. ) ;
#15663 = ORIENTED_EDGE ( 'NONE', *, *, #33847, .F. ) ;
#15664 = EDGE_CURVE ( 'NONE', #14413, #26963, #31476, .T. ) ;
#15665 = DIRECTION ( 'NONE',  ( -0.000000000000000000, -0.2588190451025194627, -0.9659258262890686453 ) ) ;
#15666 = EDGE_CURVE ( 'NONE', #19761, #24733, #16482, .T. ) ;
#15667 = FILL_AREA_STYLE_COLOUR ( '', #10463 ) ;
#15668 = FACE_OUTER_BOUND ( 'NONE', #35174, .T. ) ;
#15669 = VERTEX_POINT ( 'NONE', #7175 ) ;
#15670 = ORIENTED_EDGE ( 'NONE', *, *, #231, .F. ) ;
#15671 = CARTESIAN_POINT ( 'NONE',  ( -34.50000000000000000, -113.0974311500471714, -2.624782352598442614 ) ) ;
#15672 = CIRCLE ( 'NONE', #5348, 5.000000000000011546 ) ;
#15673 = AXIS2_PLACEMENT_3D ( 'NONE', #29355, #24305, #5228 ) ;
#15674 = CARTESIAN_POINT ( 'NONE',  ( 7.999999999999992895, -42.03146605346771025, -22.12489237027362421 ) ) ;
#15675 = EDGE_LOOP ( 'NONE', ( #5502, #3284, #11710, #321 ) ) ;
#15676 = ORIENTED_EDGE ( 'NONE', *, *, #25683, .T. ) ;
#15677 = CARTESIAN_POINT ( 'NONE',  ( -35.50000000000000711, -114.4026847875275337, 9.592046023459676718 ) ) ;
#15678 = EDGE_CURVE ( 'NONE', #33648, #10684, #21720, .T. ) ;
#15679 = CARTESIAN_POINT ( 'NONE',  ( -34.50000000000000000, -113.9743717753924699, 10.50403980422039396 ) ) ;
#15680 = LINE ( 'NONE', #17721, #30398 ) ;
#15681 = CARTESIAN_POINT ( 'NONE',  ( -39.49999999999999289, -14.17619866229204106, 94.12476896299857287 ) ) ;
#15682 = CARTESIAN_POINT ( 'NONE',  ( -38.00000000000000711, -113.9929510916434339, 12.53051367006571937 ) ) ;
#15683 = CARTESIAN_POINT ( 'NONE',  ( -37.89983305244309264, -115.9929510916434481, 12.92579853460519423 ) ) ;
#15684 = DIRECTION ( 'NONE',  ( 1.000000000000000000, 0.000000000000000000, 0.000000000000000000 ) ) ;
#15685 = AXIS2_PLACEMENT_3D ( 'NONE', #8592, #14523, #33816 ) ;
#15686 = DIRECTION ( 'NONE',  ( 1.000000000000000000, 1.734723475976807094E-16, 0.000000000000000000 ) ) ;
#15687 = VECTOR ( 'NONE', #7917, 1000.000000000000114 ) ;
#15688 = ORIENTED_EDGE ( 'NONE', *, *, #3341, .T. ) ;
#15689 = CARTESIAN_POINT ( 'NONE',  ( -21.15833593587365513, -29.98076211353323828, 86.49999999999990052 ) ) ;
#15690 = DIRECTION ( 'NONE',  ( -1.000000000000000000, 0.000000000000000000, 0.000000000000000000 ) ) ;
#15691 = CARTESIAN_POINT ( 'NONE',  ( 4.000000000000000000, 4.627536653468036720E-16, 45.00000000000000000 ) ) ;
#15692 = ADVANCED_FACE ( 'NONE', ( #29867 ), #1610, .T. ) ;
#15693 = ORIENTED_EDGE ( 'NONE', *, *, #32762, .F. ) ;
#15694 = DIRECTION ( 'NONE',  ( 0.000000000000000000, 0.000000000000000000, -1.000000000000000000 ) ) ;
#15695 = EDGE_CURVE ( 'NONE', #23680, #15252, #23931, .T. ) ;
#15696 = CIRCLE ( 'NONE', #9954, 8.000000000000001776 ) ;
#15697 = AXIS2_PLACEMENT_3D ( 'NONE', #8383, #286, #33242 ) ;
#15698 = CARTESIAN_POINT ( 'NONE',  ( -35.50000000000000711, -112.0140978167138712, -0.4997823525984337878 ) ) ;
#15699 = DIRECTION ( 'NONE',  ( 1.000000000000000000, 0.000000000000000000, 0.000000000000000000 ) ) ;
#15700 = CIRCLE ( 'NONE', #20290, 7.199999999999993960 ) ;
#15701 = CARTESIAN_POINT ( 'NONE',  ( 7.999999999999992895, -26.17370628620627215, -39.63700417846191471 ) ) ;
#15702 = FACE_OUTER_BOUND ( 'NONE', #33637, .T. ) ;
#15703 = VERTEX_POINT ( 'NONE', #12765 ) ;
#15704 = DIRECTION ( 'NONE',  ( 0.000000000000000000, -1.000000000000000000, 0.000000000000000000 ) ) ;
#15705 = CARTESIAN_POINT ( 'NONE',  ( -35.50000000000000000, -113.1807644833805426, -2.624782352598442614 ) ) ;
#15706 = DIRECTION ( 'NONE',  ( -1.783119874454246424E-31, -1.187911941725854497E-31, 1.000000000000000000 ) ) ;
#15707 = VERTEX_POINT ( 'NONE', #29160 ) ;
#15708 = ORIENTED_EDGE ( 'NONE', *, *, #23890, .T. ) ;
#15709 = ADVANCED_FACE ( 'NONE', ( #32206 ), #18338, .T. ) ;
#15710 = CARTESIAN_POINT ( 'NONE',  ( -37.74901162816869515, -114.6652019342044042, 6.566024454178448266 ) ) ;
#15711 = EDGE_CURVE ( 'NONE', #11436, #5280, #10596, .T. ) ;
#15712 =( NAMED_UNIT ( * ) PLANE_ANGLE_UNIT ( ) SI_UNIT ( $, .RADIAN. ) );
#15713 = CARTESIAN_POINT ( 'NONE',  ( 1.110223024625156540E-13, -1.000000000000042633, -32.00000000000000000 ) ) ;
#15714 = VERTEX_POINT ( 'NONE', #15613 ) ;
#15715 = ORIENTED_EDGE ( 'NONE', *, *, #7085, .F. ) ;
#15716 = CARTESIAN_POINT ( 'NONE',  ( -34.50000000000000000, -113.2224311500466030, -0.6247823525984269599 ) ) ;
#15717 = DIRECTION ( 'NONE',  ( 0.000000000000000000, 0.8443279255020161855, -0.5358267949789946583 ) ) ;
#15718 = CARTESIAN_POINT ( 'NONE',  ( 0.000000000000000000, 27.43636312076321104, 38.14186064215159888 ) ) ;
#15719 = AXIS2_PLACEMENT_3D ( 'NONE', #19075, #32590, #13692 ) ;
#15720 = CARTESIAN_POINT ( 'NONE',  ( -37.50613590685470911, -114.9929510916434339, 13.11852378322482515 ) ) ;
#15721 = CIRCLE ( 'NONE', #10578, 7.199999999999992184 ) ;
#15722 = DIRECTION ( 'NONE',  ( 1.000000000000000000, -5.339440136655842133E-16, -1.047965281155519420E-16 ) ) ;
#15723 = DIRECTION ( 'NONE',  ( -1.174092375852890260E-15, 4.222049128630259891E-16, 1.000000000000000000 ) ) ;
#15724 = CARTESIAN_POINT ( 'NONE',  ( -34.50000000000000000, -112.0140978167138712, 0.7189676474015718188 ) ) ;
#15725 = CARTESIAN_POINT ( 'NONE',  ( -34.49999793727135255, -114.9929510916434339, 12.61164896875036590 ) ) ;
#15726 = DIRECTION ( 'NONE',  ( 0.000000000000000000, 0.000000000000000000, 1.000000000000000000 ) ) ;
#15727 = DIRECTION ( 'NONE',  ( -1.000000000000000000, -1.836970198721029934E-16, -0.000000000000000000 ) ) ;
#15728 = ORIENTED_EDGE ( 'NONE', *, *, #11627, .F. ) ;
#15729 = CARTESIAN_POINT ( 'NONE',  ( -37.24999999999992184, -115.9929510916434481, 13.11852480586264846 ) ) ;
#15730 = CARTESIAN_POINT ( 'NONE',  ( -35.50000000000000711, -115.5178116849130276, -1.498529437126731034 ) ) ;
#15731 = CARTESIAN_POINT ( 'NONE',  ( 70.00000000000001421, 46.66021779527611102, 66.80632251401318911 ) ) ;
#15732 = DIRECTION ( 'NONE',  ( -1.000000000000000000, 0.000000000000000000, 0.000000000000000000 ) ) ;
#15733 = VERTEX_POINT ( 'NONE', #15977 ) ;
#15734 = CARTESIAN_POINT ( 'NONE',  ( -3.799999999999999378, 1.782605128514165574E-14, -4.461551028240973403E-15 ) ) ;
#15735 = CYLINDRICAL_SURFACE ( 'NONE', #30790, 47.49900000000001654 ) ;
#15736 = ADVANCED_FACE ( 'NONE', ( #18510 ), #26275, .T. ) ;
#15737 = DIRECTION ( 'NONE',  ( -1.000000000000000000, 0.000000000000000000, 0.000000000000000000 ) ) ;
#15738 = CARTESIAN_POINT ( 'NONE',  ( 3.799999999999999822, 4.382607293638566128E-16, -45.10000000000000142 ) ) ;
#15739 = CARTESIAN_POINT ( 'NONE',  ( -36.33479806579561000, -114.7490116281687165, 7.691024454178450043 ) ) ;
#15740 = CYLINDRICAL_SURFACE ( 'NONE', #12978, 7.999999999999992895 ) ;
#15741 = DIRECTION ( 'NONE',  ( -1.000000000000000000, -1.836970198721029934E-16, -0.000000000000000000 ) ) ;
#15742 = EDGE_LOOP ( 'NONE', ( #1928, #8408, #2682, #17796 ) ) ;
#15743 = ORIENTED_EDGE ( 'NONE', *, *, #34093, .F. ) ;
#15744 = CIRCLE ( 'NONE', #33015, 7.199999999999995737 ) ;
#15745 = CARTESIAN_POINT ( 'NONE',  ( -35.00000000000000000, -114.0592624029313953, 1.503524454178449599 ) ) ;
#15746 = AXIS2_PLACEMENT_3D ( 'NONE', #20863, #31865, #7196 ) ;
#15747 = CARTESIAN_POINT ( 'NONE',  ( 70.00000000000001421, 54.25778039068027425, 73.39034659349927381 ) ) ;
#15748 = CYLINDRICAL_SURFACE ( 'NONE', #14612, 52.00000000000000711 ) ;
#15749 = ORIENTED_EDGE ( 'NONE', *, *, #14367, .T. ) ;
#15750 = CARTESIAN_POINT ( 'NONE',  ( -36.94073759706868287, -115.9999999999999858, 8.871475545821551734 ) ) ;
#15751 = ORIENTED_EDGE ( 'NONE', *, *, #23395, .T. ) ;
#15752 = EDGE_LOOP ( 'NONE', ( #31879, #35232, #3241, #6375 ) ) ;
#15753 = EDGE_LOOP ( 'NONE', ( #21888, #20668, #10726, #29892 ) ) ;
#15754 = DIRECTION ( 'NONE',  ( -1.000000000000000000, 0.000000000000000000, 0.000000000000000000 ) ) ;
#15755 = DIRECTION ( 'NONE',  ( 1.734723475976807834E-16, -1.000000000000000000, 0.000000000000000000 ) ) ;
#15756 = VERTEX_POINT ( 'NONE', #15442 ) ;
#15757 = ORIENTED_EDGE ( 'NONE', *, *, #20259, .T. ) ;
#15758 = LINE ( 'NONE', #21348, #10482 ) ;
#15759 = CARTESIAN_POINT ( 'NONE',  ( -3.799999999999999822, 4.653657836759942730E-16, -53.39999999999999858 ) ) ;
#15760 = ORIENTED_EDGE ( 'NONE', *, *, #11126, .T. ) ;
#15761 = CARTESIAN_POINT ( 'NONE',  ( -55.00000000000000000, -2.775557561562891351E-14, 106.0000000000000000 ) ) ;
#15762 = DIRECTION ( 'NONE',  ( -1.000000000000000000, -0.000000000000000000, 0.000000000000000000 ) ) ;
#15763 = DIRECTION ( 'NONE',  ( 0.000000000000000000, 0.000000000000000000, 1.000000000000000000 ) ) ;
#15764 = CIRCLE ( 'NONE', #20356, 20.00000000000000355 ) ;
#15765 = CIRCLE ( 'NONE', #23868, 20.00000000000000711 ) ;
#15766 = DIRECTION ( 'NONE',  ( -1.000000000000000000, 0.000000000000000000, 0.000000000000000000 ) ) ;
#15767 = CARTESIAN_POINT ( 'NONE',  ( -34.97545270896703329, -113.2308352781851397, 8.909774454178448266 ) ) ;
#15768 = CARTESIAN_POINT ( 'NONE',  ( -34.50000000000000000, -115.9929510916434481, 12.50851088611648265 ) ) ;
#15769 = DIRECTION ( 'NONE',  ( 1.000000000000000000, -4.524158825347490025E-15, -1.174092375852883357E-15 ) ) ;
#15770 = AXIS2_PLACEMENT_3D ( 'NONE', #11156, #27202, #8618 ) ;
#15771 = DIRECTION ( 'NONE',  ( -1.000000000000000000, -0.000000000000000000, -0.000000000000000000 ) ) ;
#15772 = DIRECTION ( 'NONE',  ( -1.000000000000000000, -0.000000000000000000, -0.000000000000000000 ) ) ;
#15773 = DIRECTION ( 'NONE',  ( 0.000000000000000000, 0.8443279255020164076, -0.5358267949789945472 ) ) ;
#15774 = EDGE_CURVE ( 'NONE', #540, #20427, #29336, .T. ) ;
#15775 = CARTESIAN_POINT ( 'NONE',  ( 0.000000000000000000, 18.48663108841356717, 3.384281271888136988 ) ) ;
#15776 = CARTESIAN_POINT ( 'NONE',  ( 4.000000000000000000, 4.627536653468036720E-16, -45.00000000000000000 ) ) ;
#15777 = EDGE_LOOP ( 'NONE', ( #26986, #34757 ) ) ;
#15778 = CARTESIAN_POINT ( 'NONE',  ( -39.99999999999999289, -114.0592624029313242, 9.246475545821549957 ) ) ;
#15779 = CARTESIAN_POINT ( 'NONE',  ( 0.000000000000000000, -19.60123832284022782, 3.973846525876367330 ) ) ;
#15780 = DIRECTION ( 'NONE',  ( 0.000000000000000000, 0.000000000000000000, 1.000000000000000000 ) ) ;
#15781 = ORIENTED_EDGE ( 'NONE', *, *, #33075, .F. ) ;
#15782 = EDGE_LOOP ( 'NONE', ( #9472, #12444, #11154, #35488 ) ) ;
#15783 =( LENGTH_UNIT ( ) NAMED_UNIT ( * ) SI_UNIT ( .MILLI., .METRE. ) );
#15784 = FACE_OUTER_BOUND ( 'NONE', #2386, .T. ) ;
#15785 = ORIENTED_EDGE ( 'NONE', *, *, #12015, .T. ) ;
#15786 = ADVANCED_FACE ( 'NONE', ( #12591 ), #35275, .T. ) ;
#15787 = ORIENTED_EDGE ( 'NONE', *, *, #29757, .T. ) ;
#15788 = EDGE_LOOP ( 'NONE', ( #30447, #6057, #16544, #7494 ) ) ;
#15789 = CIRCLE ( 'NONE', #10655, 4.000000000000000000 ) ;
#15790 = DIRECTION ( 'NONE',  ( -1.000000000000000000, 0.000000000000000000, 0.000000000000000000 ) ) ;
#15791 = AXIS2_PLACEMENT_3D ( 'NONE', #12164, #6938, #20066 ) ;
#15792 = DIRECTION ( 'NONE',  ( -1.000000000000000000, 0.000000000000000000, 0.000000000000000000 ) ) ;
#15793 = CARTESIAN_POINT ( 'NONE',  ( 49.10000000000000853, -1.390489286212659437E-14, 110.0000000000000000 ) ) ;
#15794 = CIRCLE ( 'NONE', #4915, 1.000000000000000888 ) ;
#15795 = CYLINDRICAL_SURFACE ( 'NONE', #6974, 7.499999999999992895 ) ;
#15796 = VERTEX_POINT ( 'NONE', #26811 ) ;
#15797 = ORIENTED_EDGE ( 'NONE', *, *, #10595, .T. ) ;
#15798 = CARTESIAN_POINT ( 'NONE',  ( -35.50000000000000711, -113.1256619669233885, 1.895633585076891947 ) ) ;
#15799 = CIRCLE ( 'NONE', #881, 11.00000000000000000 ) ;
#15800 = CYLINDRICAL_SURFACE ( 'NONE', #34110, 3.799999999999999822 ) ;
#15801 = CARTESIAN_POINT ( 'NONE',  ( 0.000000000000000000, 5.667686777402359155, -46.64153600743598105 ) ) ;
#15802 = EDGE_LOOP ( 'NONE', ( #21486, #2980, #13612, #14366 ) ) ;
#15803 = DIRECTION ( 'NONE',  ( 0.000000000000000000, -1.000000000000000000, 1.067522139062650474E-15 ) ) ;
#15804 = EDGE_CURVE ( 'NONE', #6257, #52, #21131, .T. ) ;
#15805 = VECTOR ( 'NONE', #21448, 1000.000000000000000 ) ;
#15806 = CARTESIAN_POINT ( 'NONE',  ( -34.50000000000000000, -112.0154707866092707, 0.9357013553229778235 ) ) ;
#15807 = CARTESIAN_POINT ( 'NONE',  ( -34.54793860109200665, -114.9929510916434339, 13.00730889637958221 ) ) ;
#15808 = FACE_OUTER_BOUND ( 'NONE', #29078, .T. ) ;
#15809 = CARTESIAN_POINT ( 'NONE',  ( -37.99839555572501837, -114.9929510916434339, 12.65937477241748965 ) ) ;
#15810 = LINE ( 'NONE', #35465, #23161 ) ;
#15811 = CARTESIAN_POINT ( 'NONE',  ( -34.50000000000000000, -114.3464919575557843, 9.568884482464163455 ) ) ;
#15812 = CYLINDRICAL_SURFACE ( 'NONE', #21063, 17.49900000000000233 ) ;
#15813 = CARTESIAN_POINT ( 'NONE',  ( 8.000000000000000000, -14.87816164169111310, -4.342730381190021305 ) ) ;
#15814 = ORIENTED_EDGE ( 'NONE', *, *, #28519, .T. ) ;
#15815 = DIRECTION ( 'NONE',  ( 1.110223024625156540E-16, 1.000000000000000000, 0.000000000000000000 ) ) ;
#15816 = CARTESIAN_POINT ( 'NONE',  ( -34.49999999999998579, -25.27980021920989984, 89.21410161513769310 ) ) ;
#15817 = EDGE_CURVE ( 'NONE', #21198, #28224, #20562, .T. ) ;
#15818 = AXIS2_PLACEMENT_3D ( 'NONE', #25992, #12124, #3679 ) ;
#15819 = EDGE_LOOP ( 'NONE', ( #24240, #7937, #11482, #29526 ) ) ;
#15820 = EDGE_CURVE ( 'NONE', #26535, #23109, #25187, .T. ) ;
#15821 = CARTESIAN_POINT ( 'NONE',  ( -37.99999897736218202, -114.9929510916434339, 12.62466071271732915 ) ) ;
#15822 = EDGE_LOOP ( 'NONE', ( #20612, #13789, #27763, #1602 ) ) ;
#15823 = EDGE_CURVE ( 'NONE', #28885, #23250, #13475, .T. ) ;
#15824 = CARTESIAN_POINT ( 'NONE',  ( -39.16322519054179452, -116.0794154965774823, 2.066024454178448710 ) ) ;
#15825 = DIRECTION ( 'NONE',  ( 0.000000000000000000, 0.000000000000000000, -1.000000000000000000 ) ) ;
#15826 = CIRCLE ( 'NONE', #3211, 20.00000000000000355 ) ;
#15827 = ORIENTED_EDGE ( 'NONE', *, *, #6641, .T. ) ;
#15828 = ORIENTED_EDGE ( 'NONE', *, *, #32651, .T. ) ;
#15829 = DIRECTION ( 'NONE',  ( -1.000000000000000000, 0.000000000000000000, 0.000000000000000000 ) ) ;
#15830 = EDGE_CURVE ( 'NONE', #24024, #22936, #30044, .T. ) ;
#15831 = ORIENTED_EDGE ( 'NONE', *, *, #19560, .F. ) ;
#15832 = CARTESIAN_POINT ( 'NONE',  ( -34.83677480945819838, -111.9205845034225462, 4.316024454178448266 ) ) ;
#15833 = ADVANCED_FACE ( 'NONE', ( #8756 ), #2688, .T. ) ;
#15834 = CIRCLE ( 'NONE', #323, 52.00000000000000711 ) ;
#15835 = APPLICATION_CONTEXT ( 'automotive_design' ) ;
#15836 = CARTESIAN_POINT ( 'NONE',  ( 0.000000000000000000, -2.710505431213761085E-17, -20.99999999999999645 ) ) ;
#15837 = DIRECTION ( 'NONE',  ( -1.000000000000000000, 0.000000000000000000, 0.000000000000000000 ) ) ;
#15838 = ORIENTED_EDGE ( 'NONE', *, *, #15289, .T. ) ;
#15839 = ORIENTED_EDGE ( 'NONE', *, *, #8025, .F. ) ;
#15840 = CARTESIAN_POINT ( 'NONE',  ( 7.999999999999992895, 46.19362259308833529, 8.585149169758651055 ) ) ;
#15841 =( LENGTH_UNIT ( ) NAMED_UNIT ( * ) SI_UNIT ( .MILLI., .METRE. ) );
#15842 = DIRECTION ( 'NONE',  ( -1.000000000000000000, 0.000000000000000000, 0.000000000000000000 ) ) ;
#15843 = ORIENTED_EDGE ( 'NONE', *, *, #11481, .F. ) ;
#15844 = ORIENTED_EDGE ( 'NONE', *, *, #448, .F. ) ;
#15845 = CARTESIAN_POINT ( 'NONE',  ( -34.50000000000000000, -112.0066700803175763, -2.372276521656937920 ) ) ;
#15846 = CIRCLE ( 'NONE', #31384, 13.99999999999999645 ) ;
#15847 = CARTESIAN_POINT ( 'NONE',  ( 7.999999999999992895, -30.93515269692138503, 36.04401931830242489 ) ) ;
#15848 = VERTEX_POINT ( 'NONE', #5726 ) ;
#15849 = CARTESIAN_POINT ( 'NONE',  ( -35.50000000000000711, -114.9922651054798308, 10.46846006712531008 ) ) ;
#15850 = VECTOR ( 'NONE', #25271, 1000.000000000000000 ) ;
#15851 = EDGE_CURVE ( 'NONE', #8283, #11310, #13697, .T. ) ;
#15852 = AXIS2_PLACEMENT_3D ( 'NONE', #5923, #3234, #12386 ) ;
#15853 = AXIS2_PLACEMENT_3D ( 'NONE', #6580, #23692, #28561 ) ;
#15854 = CARTESIAN_POINT ( 'NONE',  ( -34.50000000000000000, -113.9929510916434339, 10.51175824272318415 ) ) ;
#15855 = EDGE_CURVE ( 'NONE', #13276, #23525, #22095, .T. ) ;
#15856 = DIRECTION ( 'NONE',  ( 1.000000000000000000, -5.339440136655842133E-16, -1.047965281155519420E-16 ) ) ;
#15857 = LINE ( 'NONE', #27228, #18540 ) ;
#15858 = CARTESIAN_POINT ( 'NONE',  ( -37.75185693410092824, -113.9929510916434339, 13.05539834812634759 ) ) ;
#15859 = CIRCLE ( 'NONE', #22187, 52.00000000000000711 ) ;
#15860 = CARTESIAN_POINT ( 'NONE',  ( -36.07812499999994316, -115.9929510916434481, 13.11852480586264846 ) ) ;
#15861 = AXIS2_PLACEMENT_3D ( 'NONE', #33627, #23001, #4127 ) ;
#15862 = CARTESIAN_POINT ( 'NONE',  ( -4.000000000000000000, 0.000000000000000000, 55.00000000000000000 ) ) ;
#15863 = LINE ( 'NONE', #34993, #278 ) ;
#15864 = EDGE_CURVE ( 'NONE', #17076, #2951, #5631, .T. ) ;
#15865 = EDGE_CURVE ( 'NONE', #2544, #32647, #29794, .T. ) ;
#15866 = VERTEX_POINT ( 'NONE', #13994 ) ;
#15867 = EDGE_CURVE ( 'NONE', #20005, #27414, #16150, .T. ) ;
#15868 = DIRECTION ( 'NONE',  ( 0.000000000000000000, -1.000000000000000000, 0.000000000000000000 ) ) ;
#15869 = LINE ( 'NONE', #7957, #7061 ) ;
#15870 = CARTESIAN_POINT ( 'NONE',  ( 1.599999999999990319, 0.000000000000000000, 0.000000000000000000 ) ) ;
#15871 = EDGE_LOOP ( 'NONE', ( #32132, #22205, #34006, #7933 ) ) ;
#15872 = DIRECTION ( 'NONE',  ( 0.000000000000000000, 0.9510565162951545304, -0.3090169943749447867 ) ) ;
#15873 = VECTOR ( 'NONE', #23051, 1000.000000000000114 ) ;
#15874 = CARTESIAN_POINT ( 'NONE',  ( -35.50000000000000711, -112.0577668799241309, 1.173706424699810569 ) ) ;
#15875 = DIRECTION ( 'NONE',  ( 0.1305261922200510738, -0.9914448613738104932, 1.248897716083276957E-31 ) ) ;
#15876 = CARTESIAN_POINT ( 'NONE',  ( -35.50000000000000711, -114.9929510916434339, 10.55026311463432087 ) ) ;
#15877 = CARTESIAN_POINT ( 'NONE',  ( 0.000000000000000000, 0.000000000000000000, -40.00000000000000711 ) ) ;
#15878 = STYLED_ITEM ( 'NONE', ( #32979 ), #22133 ) ;
#15879 = CIRCLE ( 'NONE', #29705, 4.000000000000014211 ) ;
#15880 = EDGE_CURVE ( 'NONE', #30332, #1954, #22877, .T. ) ;
#15881 = ORIENTED_EDGE ( 'NONE', *, *, #18882, .F. ) ;
#15882 = CIRCLE ( 'NONE', #7256, 4.799999999999998934 ) ;
#15883 = CYLINDRICAL_SURFACE ( 'NONE', #13619, 4.000000000000003553 ) ;
#15884 = CARTESIAN_POINT ( 'NONE',  ( -35.50000000000000000, -114.1807644833817648, -2.624782352598442614 ) ) ;
#15885 = ORIENTED_EDGE ( 'NONE', *, *, #14417, .F. ) ;
#15886 = ORIENTED_EDGE ( 'NONE', *, *, #21552, .F. ) ;
#15887 = CIRCLE ( 'NONE', #25104, 20.00000000000000355 ) ;
#15888 = CARTESIAN_POINT ( 'NONE',  ( -38.97545270896704039, -113.1123104723225197, 2.347274454178448710 ) ) ;
#15889 = AXIS2_PLACEMENT_3D ( 'NONE', #9786, #7079, #18054 ) ;
#15890 = CIRCLE ( 'NONE', #7267, 15.49899999999998457 ) ;
#15891 = CARTESIAN_POINT ( 'NONE',  ( 7.999999999999992895, -46.87740477351715640, 16.82754413119429415 ) ) ;
#15892 = ORIENTED_EDGE ( 'NONE', *, *, #19777, .F. ) ;
#15893 = ORIENTED_EDGE ( 'NONE', *, *, #21844, .T. ) ;
#15894 = CARTESIAN_POINT ( 'NONE',  ( -34.50000000000000000, -114.8057644833805853, -0.6247823525984269599 ) ) ;
#15895 = DIRECTION ( 'NONE',  ( -1.000000000000000000, -0.000000000000000000, -0.000000000000000000 ) ) ;
#15896 = EDGE_CURVE ( 'NONE', #27135, #5839, #24457, .T. ) ;
#15897 = CARTESIAN_POINT ( 'NONE',  ( 0.000000000000000000, -2.710505431213761085E-17, 38.90000000000000568 ) ) ;
#15898 = AXIS2_PLACEMENT_3D ( 'NONE', #22632, #25370, #6091 ) ;
#15899 = VECTOR ( 'NONE', #30809, 1000.000000000000000 ) ;
#15900 = CARTESIAN_POINT ( 'NONE',  ( -38.00000000000000711, -114.9929510916434339, 12.17846912687782179 ) ) ;
#15901 = EDGE_CURVE ( 'NONE', #33477, #5642, #34967, .T. ) ;
#15902 = CARTESIAN_POINT ( 'NONE',  ( 0.000000000000000000, 0.000000000000000000, 0.000000000000000000 ) ) ;
#15903 = DIRECTION ( 'NONE',  ( -1.000000000000000000, 0.000000000000000000, -0.000000000000000000 ) ) ;
#15904 = CARTESIAN_POINT ( 'NONE',  ( -34.50000000000000000, -112.8511839106603247, -1.611965039240275122 ) ) ;
#15905 = COLOUR_RGB ( '', 0.08235294, 0.09019608, 0.10196078) ;
#15906 = CIRCLE ( 'NONE', #17059, 52.00000000000000711 ) ;
#15907 = DIRECTION ( 'NONE',  ( 0.000000000000000000, 0.000000000000000000, 1.000000000000000000 ) ) ;
#15908 = AXIS2_PLACEMENT_3D ( 'NONE', #28306, #4189, #6507 ) ;
#15909 = VECTOR ( 'NONE', #35211, 1000.000000000000000 ) ;
#15910 = EDGE_CURVE ( 'NONE', #21654, #28712, #24039, .T. ) ;
#15911 = CARTESIAN_POINT ( 'NONE',  ( 8.000000000000000000, 9.471478019455355835, -14.71414642875945411 ) ) ;
#15913 = ORIENTED_EDGE ( 'NONE', *, *, #19414, .T. ) ;
#15912 = VECTOR ( 'NONE', #32907, 1000.000000000000000 ) ;
#15914 = CARTESIAN_POINT ( 'NONE',  ( -37.49414064056232831, -115.9929510916434481, 13.11852578240983291 ) ) ;
#15915 = DIRECTION ( 'NONE',  ( 1.000000000000000000, 1.734723475976807094E-16, 0.000000000000000000 ) ) ;
#15916 = ADVANCED_FACE ( 'NONE', ( #137, #33094 ), #311, .F. ) ;
#15917 = DIRECTION ( 'NONE',  ( 0.000000000000000000, -0.8660254037844444808, 0.4999999999999898415 ) ) ;
#15918 = CARTESIAN_POINT ( 'NONE',  ( -9.999999999999994671, 0.000000000000000000, 0.000000000000000000 ) ) ;
#15919 = VERTEX_POINT ( 'NONE', #16860 ) ;
#15920 = CARTESIAN_POINT ( 'NONE',  ( 7.999999999999992895, 0.000000000000000000, 0.000000000000000000 ) ) ;
#15921 = CARTESIAN_POINT ( 'NONE',  ( 0.000000000000000000, 19.83898331853685448, 9.508666619816713350 ) ) ;
#15922 = CARTESIAN_POINT ( 'NONE',  ( 8.000000000000000000, -16.59870953437678409, -3.253005020244019718 ) ) ;
#15923 = DIRECTION ( 'NONE',  ( 1.000000000000000000, 0.000000000000000000, 0.000000000000000000 ) ) ;
#15924 = CARTESIAN_POINT ( 'NONE',  ( 7.999999999999992895, 44.61570720899095477, -14.73072383765580717 ) ) ;
#15925 = DIRECTION ( 'NONE',  ( 0.000000000000000000, 0.000000000000000000, 1.000000000000000000 ) ) ;
#15926 = ORIENTED_EDGE ( 'NONE', *, *, #2267, .F. ) ;
#15927 = AXIS2_PLACEMENT_3D ( 'NONE', #24265, #2843, #5188 ) ;
#15928 = VERTEX_POINT ( 'NONE', #32733 ) ;
#15929 = CARTESIAN_POINT ( 'NONE',  ( 50.00005079999998969, 0.000000000000000000, 0.000000000000000000 ) ) ;
#15930 = AXIS2_PLACEMENT_3D ( 'NONE', #11405, #28147, #19656 ) ;
#15931 = FACE_OUTER_BOUND ( 'NONE', #11036, .T. ) ;
#15932 = FACE_OUTER_BOUND ( 'NONE', #9827, .T. ) ;
#15933 = ORIENTED_EDGE ( 'NONE', *, *, #19377, .F. ) ;
#15934 = CARTESIAN_POINT ( 'NONE',  ( -35.02454729103298803, -113.1123104723225197, 8.402725545821549957 ) ) ;
#15935 = VERTEX_POINT ( 'NONE', #27697 ) ;
#15936 =( NAMED_UNIT ( * ) SI_UNIT ( $, .STERADIAN. ) SOLID_ANGLE_UNIT ( ) );
#15937 = EDGE_LOOP ( 'NONE', ( #9397, #25757, #30220, #12536 ) ) ;
#15938 = ORIENTED_EDGE ( 'NONE', *, *, #26013, .T. ) ;
#15939 = CIRCLE ( 'NONE', #3884, 52.00000000000000711 ) ;
#15940 = CARTESIAN_POINT ( 'NONE',  ( 8.000000000000000000, 0.000000000000000000, 0.000000000000000000 ) ) ;
#15941 = CIRCLE ( 'NONE', #33704, 10.99999999999999822 ) ;
#15942 = VECTOR ( 'NONE', #16720, 1000.000000000000000 ) ;
#15943 = ADVANCED_FACE ( 'NONE', ( #24987 ), #11304, .T. ) ;
#15944 = DIRECTION ( 'NONE',  ( -1.000000000000000000, 0.000000000000000000, 0.000000000000000000 ) ) ;
#15945 = ORIENTED_EDGE ( 'NONE', *, *, #28455, .F. ) ;
#15946 = EDGE_LOOP ( 'NONE', ( #29203, #14426 ) ) ;
#15947 = ADVANCED_FACE ( 'NONE', ( #10777 ), #27862, .T. ) ;
#15948 = DIRECTION ( 'NONE',  ( 0.000000000000000000, 0.9510565162951521989, 0.3090169943749515036 ) ) ;
#15949 = DIRECTION ( 'NONE',  ( 0.000000000000000000, 0.000000000000000000, 1.000000000000000000 ) ) ;
#15950 = CARTESIAN_POINT ( 'NONE',  ( 0.000000000000000000, -2.710505431213761085E-17, 29.09999999999999787 ) ) ;
#15951 = AXIS2_PLACEMENT_3D ( 'NONE', #22732, #14815, #30848 ) ;
#15952 = CARTESIAN_POINT ( 'NONE',  ( 8.000000000000000000, 18.62763138773855687, 10.49404041845541968 ) ) ;
#15953 = DIRECTION ( 'NONE',  ( -0.000000000000000000, -0.000000000000000000, -1.000000000000000000 ) ) ;
#15954 = AXIS2_PLACEMENT_3D ( 'NONE', #8037, #24612, #29654 ) ;
#15955 = CARTESIAN_POINT ( 'NONE',  ( -38.37230871539094323, -112.5438815906447729, 6.941024454178449155 ) ) ;
#15956 = CARTESIAN_POINT ( 'NONE',  ( -35.07817881376918479, -115.9929510916434481, 13.81802396319203474 ) ) ;
#15957 = DIRECTION ( 'NONE',  ( 1.000000000000000000, -0.000000000000000000, -0.000000000000000000 ) ) ;
#15958 = AXIS2_PLACEMENT_3D ( 'NONE', #21213, #7882, #5026 ) ;
#15959 = DIRECTION ( 'NONE',  ( -1.000000000000000000, 0.000000000000000000, 0.000000000000000000 ) ) ;
#15960 = AXIS2_PLACEMENT_3D ( 'NONE', #6592, #1384, #22977 ) ;
#15961 = CARTESIAN_POINT ( 'NONE',  ( 5.400000000000071410, 0.9999999999999662492, 53.00000000000000711 ) ) ;
#15962 = CARTESIAN_POINT ( 'NONE',  ( 0.000000000000000000, -16.71027810728550733, -2.620268201066114688 ) ) ;
#15963 = DIRECTION ( 'NONE',  ( 1.000000000000000000, -4.524158825347490025E-15, -1.174092375852883357E-15 ) ) ;
#15964 = CARTESIAN_POINT ( 'NONE',  ( 0.000000000000000000, 16.71027810728549667, 2.620268201066223934 ) ) ;
#15965 = ORIENTED_EDGE ( 'NONE', *, *, #32177, .T. ) ;
#15966 = CARTESIAN_POINT ( 'NONE',  ( -38.30190309005061522, -111.0245472910330022, 9.527725545821551734 ) ) ;
#15967 = AXIS2_PLACEMENT_3D ( 'NONE', #34551, #17960, #9516 ) ;
#15968 = CARTESIAN_POINT ( 'NONE',  ( -39.49999999999999289, -12.31102132296306451, 91.23752798680880005 ) ) ;
#15969 = DIRECTION ( 'NONE',  ( -1.000000000000000000, 0.000000000000000000, 0.000000000000000000 ) ) ;
#15970 = VERTEX_POINT ( 'NONE', #494 ) ;
#15971 = VERTEX_POINT ( 'NONE', #11473 ) ;
#15972 = CARTESIAN_POINT ( 'NONE',  ( 8.000000000000007105, 11.27190672109280811, -0.3151488735047974776 ) ) ;
#15973 = CARTESIAN_POINT ( 'NONE',  ( 7.999999999999992895, -46.87740477351715640, -3.172455868805712509 ) ) ;
#15974 = ORIENTED_EDGE ( 'NONE', *, *, #12631, .T. ) ;
#15975 = ORIENTED_EDGE ( 'NONE', *, *, #32911, .T. ) ;
#15976 = CARTESIAN_POINT ( 'NONE',  ( 0.000000000000000000, -41.20225022064621356, -23.63323037071446464 ) ) ;
#15977 = CARTESIAN_POINT ( 'NONE',  ( 0.000000000000000000, -15.17386234660395417, 15.92965478239613830 ) ) ;
#15978 = AXIS2_PLACEMENT_3D ( 'NONE', #26109, #7010, #12060 ) ;
#15979 = CARTESIAN_POINT ( 'NONE',  ( -34.49999999999998579, -25.98076211353322051, 84.99999999999994316 ) ) ;
#15980 = DIRECTION ( 'NONE',  ( -1.000000000000000000, 0.000000000000000000, 0.000000000000000000 ) ) ;
#15981 = VERTEX_POINT ( 'NONE', #21739 ) ;
#15982 = ORIENTED_EDGE ( 'NONE', *, *, #23790, .T. ) ;
#15983 = CARTESIAN_POINT ( 'NONE',  ( -35.50000000000000711, -112.0140978167138712, 0.6252176474015680441 ) ) ;
#15984 = ADVANCED_FACE ( 'NONE', ( #22613 ), #4106, .T. ) ;
#15985 = DIRECTION ( 'NONE',  ( 0.000000000000000000, 0.000000000000000000, 1.000000000000000000 ) ) ;
#15986 = DIRECTION ( 'NONE',  ( 0.000000000000000000, 0.000000000000000000, 1.000000000000000000 ) ) ;
#15987 = ORIENTED_EDGE ( 'NONE', *, *, #11009, .F. ) ;
#15988 = CIRCLE ( 'NONE', #5106, 11.00000000000001066 ) ;
#15989 = DIRECTION ( 'NONE',  ( 0.000000000000000000, 0.5877852522924682521, 0.8090169943749511150 ) ) ;
#15990 = CARTESIAN_POINT ( 'NONE',  ( -34.50000000000000000, -115.9630435732166518, -0.9469505670456015434 ) ) ;
#15991 = CARTESIAN_POINT ( 'NONE',  ( -38.81062062679291103, -114.9929510916434339, 13.37409560816442067 ) ) ;
#15992 = DIRECTION ( 'NONE',  ( 0.000000000000000000, 0.000000000000000000, 1.000000000000000000 ) ) ;
#15993 = CARTESIAN_POINT ( 'NONE',  ( -35.50000000000000000, -113.9929510916434339, 10.52826033068511435 ) ) ;
#15994 = CARTESIAN_POINT ( 'NONE',  ( 4.000000000000003553, -15.17386234660395417, 15.92965478239613830 ) ) ;
#15995 = ADVANCED_FACE ( 'NONE', ( #28391 ), #6421, .T. ) ;
#15996 = CARTESIAN_POINT ( 'NONE',  ( -34.50000000000000000, -114.9929510916434339, 10.55026311463432087 ) ) ;
#15997 = CARTESIAN_POINT ( 'NONE',  ( 5.400000000000085620, -1.000000000000049516, 53.00000000000000711 ) ) ;
#15998 = CARTESIAN_POINT ( 'NONE',  ( -38.00000000000000711, -114.9929510916434339, 12.50851088611646311 ) ) ;
#15999 = SURFACE_STYLE_FILL_AREA ( #10271 ) ;
#16000 = VERTEX_POINT ( 'NONE', #17567 ) ;
#16001 = CARTESIAN_POINT ( 'NONE',  ( 4.000000000000000000, 4.898587196589412829E-16, -50.00000000000000000 ) ) ;
#16002 = DIRECTION ( 'NONE',  ( -1.000000000000000000, 0.000000000000000000, -0.000000000000000000 ) ) ;
#16003 = VERTEX_POINT ( 'NONE', #1035 ) ;
#16004 = CARTESIAN_POINT ( 'NONE',  ( -38.00000000000000711, -114.9929510916434339, 12.44250253426874941 ) ) ;
#16005 = ORIENTED_EDGE ( 'NONE', *, *, #4307, .F. ) ;
#16006 = CARTESIAN_POINT ( 'NONE',  ( -35.00000000000000000, -114.0592624029313242, 7.503524454178449155 ) ) ;
#16007 = CARTESIAN_POINT ( 'NONE',  ( 7.999999999999992895, -5.667686777401384823, -46.64153600743608763 ) ) ;
#16008 = VERTEX_POINT ( 'NONE', #17389 ) ;
#16009 = AXIS2_PLACEMENT_3D ( 'NONE', #23118, #23844, #4240 ) ;
#16010 = VERTEX_POINT ( 'NONE', #28576 ) ;
#16011 = CARTESIAN_POINT ( 'NONE',  ( 7.999999999999992895, 0.000000000000000000, 3.000000000000002665 ) ) ;
#16012 = DIRECTION ( 'NONE',  ( -0.000000000000000000, 0.000000000000000000, -1.000000000000000000 ) ) ;
#16013 = EDGE_LOOP ( 'NONE', ( #5745, #28484, #7531, #27721 ) ) ;
#16014 = CARTESIAN_POINT ( 'NONE',  ( -36.23083527818512550, -116.0245472910329880, 7.784774454178451819 ) ) ;
#16015 = DIRECTION ( 'NONE',  ( -1.000000000000000000, 0.000000000000000000, -0.000000000000000000 ) ) ;
#16016 = DIRECTION ( 'NONE',  ( -1.000000000000000000, -0.000000000000000000, 0.000000000000000000 ) ) ;
#16017 = ORIENTED_EDGE ( 'NONE', *, *, #10831, .T. ) ;
#16018 = EDGE_LOOP ( 'NONE', ( #33695, #18644, #32, #23070 ) ) ;
#16019 = DIRECTION ( 'NONE',  ( -1.000000000000000000, 0.000000000000000000, 0.000000000000000000 ) ) ;
#16020 =( NAMED_UNIT ( * ) SI_UNIT ( $, .STERADIAN. ) SOLID_ANGLE_UNIT ( ) );
#16021 = DIRECTION ( 'NONE',  ( 0.000000000000000000, 0.000000000000000000, -1.000000000000000000 ) ) ;
#16022 = ORIENTED_EDGE ( 'NONE', *, *, #23090, .F. ) ;
#16023 = ORIENTED_EDGE ( 'NONE', *, *, #12416, .F. ) ;
#16024 = CARTESIAN_POINT ( 'NONE',  ( -34.50000000000000000, -111.1014359431343905, 1.472195201997948510 ) ) ;
#16025 = EDGE_CURVE ( 'NONE', #5335, #35590, #31505, .T. ) ;
#16026 = EDGE_CURVE ( 'NONE', #8613, #933, #454, .T. ) ;
#16027 = AXIS2_PLACEMENT_3D ( 'NONE', #991, #25125, #798 ) ;
#16028 = CARTESIAN_POINT ( 'NONE',  ( -9.999999999999994671, 0.000000000000000000, 0.000000000000000000 ) ) ;
#16029 = ORIENTED_EDGE ( 'NONE', *, *, #5122, .F. ) ;
#16030 = CARTESIAN_POINT ( 'NONE',  ( -35.50000000000000711, -114.9929501463477663, 10.50247632894551231 ) ) ;
#16031 = CIRCLE ( 'NONE', #21236, 3.799999999999999822 ) ;
#16032 = CARTESIAN_POINT ( 'NONE',  ( -34.50000000000000000, -113.9186338266397058, 10.49738657667399266 ) ) ;
#16033 = DIRECTION ( 'NONE',  ( 1.000000000000000000, -0.000000000000000000, -0.000000000000000000 ) ) ;
#16034 = FACE_OUTER_BOUND ( 'NONE', #5715, .T. ) ;
#16035 = ADVANCED_FACE ( 'NONE', ( #23336 ), #25521, .T. ) ;
#16036 = CARTESIAN_POINT ( 'NONE',  ( -34.50000000000000000, -113.9929510916434339, 10.50625754673586876 ) ) ;
#16037 = CARTESIAN_POINT ( 'NONE',  ( -36.99999999999988631, -115.9929510916434481, 13.11852480586264846 ) ) ;
#16038 = CARTESIAN_POINT ( 'NONE',  ( 0.000000000000000000, 0.000000000000000000, 60.90000000000001279 ) ) ;
#16039 = FACE_OUTER_BOUND ( 'NONE', #404, .T. ) ;
#16040 = EDGE_LOOP ( 'NONE', ( #6814, #9382, #1731, #24544 ) ) ;
#16041 = CARTESIAN_POINT ( 'NONE',  ( -4.872650870659766653, 0.4273491293403325897, -0.8000000000000009326 ) ) ;
#16042 = DIRECTION ( 'NONE',  ( 0.000000000000000000, 0.000000000000000000, 1.000000000000000000 ) ) ;
#16043 = CARTESIAN_POINT ( 'NONE',  ( 115.0000000000000000, 81.48267994499606459, 30.15054357219658954 ) ) ;
#16044 = EDGE_LOOP ( 'NONE', ( #2379, #23076, #4314, #12214 ) ) ;
#16045 = CARTESIAN_POINT ( 'NONE',  ( 7.999999999999992895, 0.000000000000000000, 0.000000000000000000 ) ) ;
#16046 = APPLICATION_CONTEXT ( 'automotive_design' ) ;
#16047 = CARTESIAN_POINT ( 'NONE',  ( -35.50000000000000711, -115.3362660311619692, -1.573728109101206085 ) ) ;
#16048 = DIRECTION ( 'NONE',  ( 0.000000000000000000, 0.8660254037844363761, 0.5000000000000037748 ) ) ;
#16049 = AXIS2_PLACEMENT_3D ( 'NONE', #27306, #18478, #26965 ) ;
#16050 = CARTESIAN_POINT ( 'NONE',  ( -35.50000000000000711, -114.9902084924877954, 10.43071793783961176 ) ) ;
#16051 = LINE ( 'NONE', #10497, #11878 ) ;
#16052 = ADVANCED_FACE ( 'NONE', ( #31452 ), #33981, .F. ) ;
#16053 = VERTEX_POINT ( 'NONE', #835 ) ;
#16054 = CIRCLE ( 'NONE', #11471, 10.50000000000000178 ) ;
#16055 = CARTESIAN_POINT ( 'NONE',  ( 7.999999999999992895, 4.898587196589412829E-16, -4.000000000000000000 ) ) ;
#16056 = CARTESIAN_POINT ( 'NONE',  ( -35.50000000000000000, -111.0140978167138570, 0.2502176474015764263 ) ) ;
#16057 = ORIENTED_EDGE ( 'NONE', *, *, #9242, .F. ) ;
#16058 = ORIENTED_EDGE ( 'NONE', *, *, #19802, .T. ) ;
#16059 = CARTESIAN_POINT ( 'NONE',  ( -37.99999999999998579, -113.9407375970686758, 8.253524454178448266 ) ) ;
#16060 = AXIS2_PLACEMENT_3D ( 'NONE', #35276, #29684, #4513 ) ;
#16061 = DIRECTION ( 'NONE',  ( -1.000000000000000000, 0.000000000000000000, 0.000000000000000000 ) ) ;
#16062 = VERTEX_POINT ( 'NONE', #20085 ) ;
#16063 = VERTEX_POINT ( 'NONE', #14507 ) ;
#16064 = CARTESIAN_POINT ( 'NONE',  ( -34.50000000000000000, -113.0140978167137860, -0.6247823525984055326 ) ) ;
#16065 = DIRECTION ( 'NONE',  ( -1.000000000000000000, 0.000000000000000000, -0.000000000000000000 ) ) ;
#16066 = ADVANCED_FACE ( 'NONE', ( #28048, #1212 ), #3393, .T. ) ;
#16067 = EDGE_CURVE ( 'NONE', #33383, #2175, #11818, .T. ) ;
#16068 = EDGE_CURVE ( 'NONE', #35590, #19983, #34337, .T. ) ;
#16069 = CARTESIAN_POINT ( 'NONE',  ( 8.000000000000000000, 0.000000000000000000, 0.000000000000000000 ) ) ;
#16070 = CARTESIAN_POINT ( 'NONE',  ( -50.00000000000000000, 0.000000000000000000, 64.00000000000000000 ) ) ;
#16071 = CARTESIAN_POINT ( 'NONE',  ( -37.99599240977853754, -114.9929510916434339, 12.68378527132499478 ) ) ;
#16072 = DIRECTION ( 'NONE',  ( -1.000000000000000000, -0.000000000000000000, -0.000000000000000000 ) ) ;
#16073 = CARTESIAN_POINT ( 'NONE',  ( 7.999999999999992895, 26.17370628620710349, -39.63700417846138890 ) ) ;
#16074 = EDGE_CURVE ( 'NONE', #34282, #19124, #9678, .T. ) ;
#16075 = CARTESIAN_POINT ( 'NONE',  ( -34.50000000000000000, -112.0140978167138712, 0.6252176474015680441 ) ) ;
#16076 = ADVANCED_FACE ( 'NONE', ( #31269 ), #33800, .T. ) ;
#16077 = CARTESIAN_POINT ( 'NONE',  ( 4.000000000000003553, 13.56094713063641777, -50.20060470671727870 ) ) ;
#16078 = VECTOR ( 'NONE', #24783, 1000.000000000000000 ) ;
#16079 = DIRECTION ( 'NONE',  ( 0.000000000000000000, 0.000000000000000000, 1.000000000000000000 ) ) ;
#16080 = VERTEX_POINT ( 'NONE', #12360 ) ;
#16081 = AXIS2_PLACEMENT_3D ( 'NONE', #28203, #6761, #3543 ) ;
#16082 = CARTESIAN_POINT ( 'NONE',  ( -38.00000000000000711, -114.9929510916434339, 12.57451923796417503 ) ) ;
#16083 = CARTESIAN_POINT ( 'NONE',  ( -37.52044295795950291, -115.9929510916434481, 13.11812344617477422 ) ) ;
#16084 = DIRECTION ( 'NONE',  ( 0.000000000000000000, -0.5000000000000068834, 0.8660254037844347108 ) ) ;
#16085 = FACE_BOUND ( 'NONE', #6490, .T. ) ;
#16086 = DIRECTION ( 'NONE',  ( 0.000000000000000000, 0.3420201433256693235, -0.9396926207859082059 ) ) ;
#16087 = CARTESIAN_POINT ( 'NONE',  ( -21.15833593587365513, -23.26666049839546702, 88.29903810567660116 ) ) ;
#16088 = ORIENTED_EDGE ( 'NONE', *, *, #31329, .T. ) ;
#16089 = DIRECTION ( 'NONE',  ( -1.000000000000000000, -1.836970198721029934E-16, -0.000000000000000000 ) ) ;
#16090 = FACE_BOUND ( 'NONE', #17120, .T. ) ;
#16091 = CARTESIAN_POINT ( 'NONE',  ( -9.999999999999994671, 0.000000000000000000, 0.000000000000000000 ) ) ;
#16092 = CYLINDRICAL_SURFACE ( 'NONE', #28779, 7.199999999999994849 ) ;
#16093 = DIRECTION ( 'NONE',  ( -1.000000000000000000, 0.000000000000000000, 0.000000000000000000 ) ) ;
#16094 = CARTESIAN_POINT ( 'NONE',  ( 8.000000000000007105, -10.15474465512038194, -9.637487275701211331 ) ) ;
#16095 = EDGE_CURVE ( 'NONE', #13700, #2418, #8516, .T. ) ;
#16096 = VERTEX_POINT ( 'NONE', #14874 ) ;
#16097 = ORIENTED_EDGE ( 'NONE', *, *, #26960, .T. ) ;
#16098 =( REPRESENTATION_RELATIONSHIP ('NONE','NONE', #26607, #2005 ) REPRESENTATION_RELATIONSHIP_WITH_TRANSFORMATION ( #34874 )SHAPE_REPRESENTATION_RELATIONSHIP( ) );
#16099 = CARTESIAN_POINT ( 'NONE',  ( 8.000000000000000000, 6.085920226791021292, 15.78165944574522861 ) ) ;
#16100 = LINE ( 'NONE', #30167, #9632 ) ;
#16101 = ADVANCED_FACE ( 'NONE', ( #34157 ), #9478, .F. ) ;
#16102 = DIRECTION ( 'NONE',  ( -0.000000000000000000, -0.7535859266250379829, -0.6573494133204068612 ) ) ;
#16103 = VERTEX_POINT ( 'NONE', #28752 ) ;
#16104 = VECTOR ( 'NONE', #12692, 1000.000000000000000 ) ;
#16105 = CARTESIAN_POINT ( 'NONE',  ( -35.62769128460905677, -112.5438815906447729, 6.808975545821550845 ) ) ;
#16106 = ORIENTED_EDGE ( 'NONE', *, *, #28201, .F. ) ;
#16107 = EDGE_CURVE ( 'NONE', #2044, #2939, #11047, .T. ) ;
#16108 = FILL_AREA_STYLE ('',( #32333 ) ) ;
#16109 = ORIENTED_EDGE ( 'NONE', *, *, #34135, .F. ) ;
#16110 = AXIS2_PLACEMENT_3D ( 'NONE', #17770, #3756, #22999 ) ;
#16111 = ORIENTED_EDGE ( 'NONE', *, *, #6207, .T. ) ;
#16112 = DIRECTION ( 'NONE',  ( -0.000000000000000000, 0.000000000000000000, -1.000000000000000000 ) ) ;
#16113 = EDGE_CURVE ( 'NONE', #31925, #2504, #2790, .T. ) ;
#16114 = EDGE_CURVE ( 'NONE', #27258, #375, #10017, .T. ) ;
#16115 = DIRECTION ( 'NONE',  ( 0.000000000000000000, 0.000000000000000000, 1.000000000000000000 ) ) ;
#16116 = ORIENTED_EDGE ( 'NONE', *, *, #16747, .F. ) ;
#16117 = VERTEX_POINT ( 'NONE', #10877 ) ;
#16118 = CARTESIAN_POINT ( 'NONE',  ( 0.000000000000000000, -2.710505431213761085E-17, -46.00000000000000000 ) ) ;
#16119 = CARTESIAN_POINT ( 'NONE',  ( 7.999999999999992895, 29.60891106212789126, 37.14118181634776050 ) ) ;
#16120 = DIRECTION ( 'NONE',  ( 0.000000000000000000, 0.1253332335642974860, 0.9921147013144787641 ) ) ;
#16121 = EDGE_CURVE ( 'NONE', #4059, #5839, #14264, .T. ) ;
#16122 = DIRECTION ( 'NONE',  ( -1.226634733346697831E-16, 0.2588190451025308425, -0.9659258262890655367 ) ) ;
#16123 = DIRECTION ( 'NONE',  ( 0.000000000000000000, 0.7071067811865392461, 0.7071067811865557884 ) ) ;
#16124 = VECTOR ( 'NONE', #18165, 1000.000000000000000 ) ;
#16125 = CARTESIAN_POINT ( 'NONE',  ( -37.76916472181487450, -111.9754527089670404, 5.534774454178449155 ) ) ;
#16126 = CARTESIAN_POINT ( 'NONE',  ( -37.69578139638701941, -115.9929510916434481, 14.10650203519847778 ) ) ;
#16127 = CARTESIAN_POINT ( 'NONE',  ( -55.00000000000000000, 19.99999999999998934, 110.0000000000000000 ) ) ;
#16128 = FACE_BOUND ( 'NONE', #32188, .T. ) ;
#16129 = DIRECTION ( 'NONE',  ( -1.000000000000000000, 0.000000000000000000, 0.000000000000000000 ) ) ;
#16130 = CARTESIAN_POINT ( 'NONE',  ( -0.1085714285714300953, -3.798448662927791819, -0.7999999999999951594 ) ) ;
#16131 = CARTESIAN_POINT ( 'NONE',  ( -34.49999999999998579, -23.14406523420367634, 74.41330312067054820 ) ) ;
#16132 = ORIENTED_EDGE ( 'NONE', *, *, #13227, .T. ) ;
#16133 = CIRCLE ( 'NONE', #9236, 20.00000000000000355 ) ;
#16134 = AXIS2_PLACEMENT_3D ( 'NONE', #31796, #31447, #28749 ) ;
#16135 = CARTESIAN_POINT ( 'NONE',  ( -35.62769128460905677, -112.5438815906447729, 3.808975545821551290 ) ) ;
#16136 = CIRCLE ( 'NONE', #7519, 20.00000000000000711 ) ;
#16137 = CARTESIAN_POINT ( 'NONE',  ( 7.999999999999992895, 22.43957647427220081, -41.27978878573601662 ) ) ;
#16138 = DIRECTION ( 'NONE',  ( 0.000000000000000000, 0.000000000000000000, 1.000000000000000000 ) ) ;
#16139 = CYLINDRICAL_SURFACE ( 'NONE', #25732, 4.000000000000000000 ) ;
#16140 = EDGE_CURVE ( 'NONE', #12434, #3084, #12561, .T. ) ;
#16141 = AXIS2_PLACEMENT_3D ( 'NONE', #2510, #24116, #18514 ) ;
#16142 = ORIENTED_EDGE ( 'NONE', *, *, #20399, .T. ) ;
#16143 = ORIENTED_EDGE ( 'NONE', *, *, #231, .T. ) ;
#16144 = EDGE_CURVE ( 'NONE', #33826, #27904, #7800, .T. ) ;
#16145 = CARTESIAN_POINT ( 'NONE',  ( 7.999999999999992895, -19.44205635905512608, -43.33776004284631256 ) ) ;
#16146 = DIRECTION ( 'NONE',  ( -1.000000000000000000, 0.000000000000000000, 0.000000000000000000 ) ) ;
#16147 = ORIENTED_EDGE ( 'NONE', *, *, #32640, .T. ) ;
#16148 = ORIENTED_EDGE ( 'NONE', *, *, #10570, .F. ) ;
#16149 = DIRECTION ( 'NONE',  ( -1.000000000000000000, 0.000000000000000000, 0.000000000000000000 ) ) ;
#16150 = LINE ( 'NONE', #16326, #10227 ) ;
#16151 = EDGE_CURVE ( 'NONE', #19983, #7838, #34992, .T. ) ;
#16152 = DIRECTION ( 'NONE',  ( 0.000000000000000000, 0.000000000000000000, -1.000000000000000000 ) ) ;
#16153 = CARTESIAN_POINT ( 'NONE',  ( -43.99999999999999289, -45.00000000000000000, 0.000000000000000000 ) ) ;
#16154 = ORIENTED_EDGE ( 'NONE', *, *, #16280, .F. ) ;
#16155 = ORIENTED_EDGE ( 'NONE', *, *, #27271, .F. ) ;
#16156 = CARTESIAN_POINT ( 'NONE',  ( -35.50000000000000711, -112.0221129971568104, -0.7553032835231431319 ) ) ;
#16157 = DIRECTION ( 'NONE',  ( 1.000000000000000000, 0.000000000000000000, 0.000000000000000000 ) ) ;
#16158 = DIRECTION ( 'NONE',  ( 0.000000000000000000, 0.000000000000000000, 1.000000000000000000 ) ) ;
#16159 = AXIS2_PLACEMENT_3D ( 'NONE', #6323, #11385, #23054 ) ;
#16160 = MECHANICAL_DESIGN_GEOMETRIC_PRESENTATION_REPRESENTATION (  '', ( #11578 ), #30002 ) ;
#16161 = ORIENTED_EDGE ( 'NONE', *, *, #28808, .T. ) ;
#16162 = AXIS2_PLACEMENT_3D ( 'NONE', #26276, #15086, #31141 ) ;
#16163 = DIRECTION ( 'NONE',  ( -1.000000000000000000, 0.000000000000000000, -0.000000000000000000 ) ) ;
#16164 = CARTESIAN_POINT ( 'NONE',  ( -34.50000000000000000, -112.0140978167138712, 0.5627176474015717078 ) ) ;
#16165 = CARTESIAN_POINT ( 'NONE',  ( -37.48437500000004263, -114.9929510916434339, 14.11852480586264846 ) ) ;
#16166 = DIRECTION ( 'NONE',  ( 0.000000000000000000, -1.000000000000000000, 0.000000000000000000 ) ) ;
#16167 = CARTESIAN_POINT ( 'NONE',  ( -35.50000000000000000, -113.9929510916434197, 10.50625754673586876 ) ) ;
#16168 = DIRECTION ( 'NONE',  ( -1.000000000000000000, 0.000000000000000000, 0.000000000000000000 ) ) ;
#16169 = CARTESIAN_POINT ( 'NONE',  ( -34.50000000000000000, -114.9929510916434339, 10.72628538622835670 ) ) ;
#16170 = DIRECTION ( 'NONE',  ( 1.000000000000000000, 1.734723475976807094E-16, 0.000000000000000000 ) ) ;
#16171 = CARTESIAN_POINT ( 'NONE',  ( 50.00000000000000000, -25.98076211353320275, 84.99999999999992895 ) ) ;
#16172 = SURFACE_STYLE_USAGE ( .BOTH. , #21234 ) ;
#16173 = ORIENTED_EDGE ( 'NONE', *, *, #25143, .F. ) ;
#16174 = DIRECTION ( 'NONE',  ( 0.000000000000000000, 0.000000000000000000, 1.000000000000000000 ) ) ;
#16175 = CARTESIAN_POINT ( 'NONE',  ( 0.000000000000000000, -11.27190672109260028, 4.484851126495120077 ) ) ;
#16176 = ORIENTED_EDGE ( 'NONE', *, *, #28205, .F. ) ;
#16177 = CARTESIAN_POINT ( 'NONE',  ( -36.12500000000014211, -114.9929510916434339, 13.11852480586264669 ) ) ;
#16178 = ORIENTED_EDGE ( 'NONE', *, *, #4206, .F. ) ;
#16179 = CARTESIAN_POINT ( 'NONE',  ( -36.94073759706868287, -112.0000000000000142, 8.628524454178448266 ) ) ;
#16180 = DIRECTION ( 'NONE',  ( 0.000000000000000000, -0.2538061376417690140, -0.9672551082808337197 ) ) ;
#16181 = VERTEX_POINT ( 'NONE', #24558 ) ;
#16182 = ORIENTED_EDGE ( 'NONE', *, *, #12174, .T. ) ;
#16183 = ADVANCED_FACE ( 'NONE', ( #5468 ), #24735, .T. ) ;
#16184 = DIRECTION ( 'NONE',  ( 0.000000000000000000, 0.000000000000000000, 1.000000000000000000 ) ) ;
#16185 = DIRECTION ( 'NONE',  ( -1.000000000000000000, 0.000000000000000000, 0.000000000000000000 ) ) ;
#16186 = AXIS2_PLACEMENT_3D ( 'NONE', #30093, #5085, #35330 ) ;
#16187 = ORIENTED_EDGE ( 'NONE', *, *, #27086, .F. ) ;
#16188 = CARTESIAN_POINT ( 'NONE',  ( -36.94073759706868287, -116.9999999999999858, 2.871475545821551290 ) ) ;
#16189 = DIRECTION ( 'NONE',  ( -1.000000000000000000, 0.000000000000000000, 0.000000000000000000 ) ) ;
#16190 = DIRECTION ( 'NONE',  ( -1.783119874454246424E-31, -1.187911941725854497E-31, 1.000000000000000000 ) ) ;
#16191 = ORIENTED_EDGE ( 'NONE', *, *, #16574, .F. ) ;
#16192 = ORIENTED_EDGE ( 'NONE', *, *, #21430, .F. ) ;
#16193 = CARTESIAN_POINT ( 'NONE',  ( 70.00001200000001234, -21.98076211353320630, 85.52359877559823076 ) ) ;
#16194 =( NAMED_UNIT ( * ) PLANE_ANGLE_UNIT ( ) SI_UNIT ( $, .RADIAN. ) );
#16195 = CARTESIAN_POINT ( 'NONE',  ( 0.000000000000000000, 4.460989585140964664, 16.92083251265327348 ) ) ;
#16196 = VERTEX_POINT ( 'NONE', #29112 ) ;
#16197 = ORIENTED_EDGE ( 'NONE', *, *, #35060, .T. ) ;
#16198 =( GEOMETRIC_REPRESENTATION_CONTEXT ( 3 ) GLOBAL_UNCERTAINTY_ASSIGNED_CONTEXT ( ( #20769 ) ) GLOBAL_UNIT_ASSIGNED_CONTEXT ( ( #15190, #12702, #1358 ) ) REPRESENTATION_CONTEXT ( 'NONE', 'WORKASPACE' ) );
#16199 = CARTESIAN_POINT ( 'NONE',  ( -34.50000000000000000, -112.8832452823708792, -2.621568770093253953 ) ) ;
#16200 = CARTESIAN_POINT ( 'NONE',  ( 8.000000000000007105, 13.42368113696688958, -3.975523202427861058 ) ) ;
#16201 = ORIENTED_EDGE ( 'NONE', *, *, #1344, .F. ) ;
#16202 = CARTESIAN_POINT ( 'NONE',  ( -35.50000000000000711, -114.9929510916434339, 10.85830208992344303 ) ) ;
#16203 = CARTESIAN_POINT ( 'NONE',  ( -34.50000000000000000, -113.9929510916434339, 12.39849696637031684 ) ) ;
#16204 = DIRECTION ( 'NONE',  ( -1.000000000000000000, 0.000000000000000000, 0.000000000000000000 ) ) ;
#16205 = DIRECTION ( 'NONE',  ( 0.000000000000000000, 0.000000000000000000, 1.000000000000000000 ) ) ;
#16206 = AXIS2_PLACEMENT_3D ( 'NONE', #28759, #4112, #18653 ) ;
#16207 = AXIS2_PLACEMENT_3D ( 'NONE', #802, #12323, #8902 ) ;
#16208 = CARTESIAN_POINT ( 'NONE',  ( -37.99839555572501837, -113.9929510916434339, 12.65937477241749143 ) ) ;
#16209 = CARTESIAN_POINT ( 'NONE',  ( -36.24999999999983658, -115.9929510916434481, 13.11852480586264846 ) ) ;
#16210 = PLANE ( 'NONE',  #6687 ) ;
#16211 = FACE_OUTER_BOUND ( 'NONE', #16377, .T. ) ;
#16212 = VERTEX_POINT ( 'NONE', #26411 ) ;
#16213 = CARTESIAN_POINT ( 'NONE',  ( 0.000000000000000000, 0.000000000000000000, 0.000000000000000000 ) ) ;
#16214 = CYLINDRICAL_SURFACE ( 'NONE', #21424, 15.49899999999998457 ) ;
#16215 = DIRECTION ( 'NONE',  ( -1.000000000000000000, -1.836970198721029934E-16, -0.000000000000000000 ) ) ;
#16216 = ORIENTED_EDGE ( 'NONE', *, *, #29747, .F. ) ;
#16217 = AXIS2_PLACEMENT_3D ( 'NONE', #33374, #14448, #6189 ) ;
#16218 = CARTESIAN_POINT ( 'NONE',  ( 0.000000000000000000, -2.710505431213761085E-17, 30.00000000000000000 ) ) ;
#16219 = VERTEX_POINT ( 'NONE', #21839 ) ;
#16220 = EDGE_CURVE ( 'NONE', #9695, #32501, #24068, .T. ) ;
#16221 = CARTESIAN_POINT ( 'NONE',  ( -35.50000000000000000, -113.4742757288593964, 0.9301473394660054739 ) ) ;
#16222 = CARTESIAN_POINT ( 'NONE',  ( 0.000000000000000000, 6.085920226791238008, -15.78165944574512203 ) ) ;
#16223 = ADVANCED_FACE ( 'NONE', ( #1746 ), #34515, .T. ) ;
#16224 = AXIS2_PLACEMENT_3D ( 'NONE', #8038, #19020, #5354 ) ;
#16225 = CARTESIAN_POINT ( 'NONE',  ( -35.50000000000000711, -114.9929510916434339, 10.51175824272318415 ) ) ;
#16226 = DIRECTION ( 'NONE',  ( -1.000000000000000000, 0.000000000000000000, 0.000000000000000000 ) ) ;
#16227 = ORIENTED_EDGE ( 'NONE', *, *, #16268, .F. ) ;
#16228 = DIRECTION ( 'NONE',  ( 1.000000000000000000, -5.339440136655842133E-16, -1.047965281155519420E-16 ) ) ;
#16229 = VECTOR ( 'NONE', #8001, 1000.000000000000000 ) ;
#16230 = CARTESIAN_POINT ( 'NONE',  ( -35.50000000000000000, -111.0360125565790383, 1.176611260687384419 ) ) ;
#16231 = ORIENTED_EDGE ( 'NONE', *, *, #21194, .F. ) ;
#16232 = VERTEX_POINT ( 'NONE', #10692 ) ;
#16233 = CARTESIAN_POINT ( 'NONE',  ( -37.88768952767750164, -115.9754527089670262, 1.972274454178448710 ) ) ;
#16234 = EDGE_CURVE ( 'NONE', #9078, #33007, #13753, .T. ) ;
#16235 = AXIS2_PLACEMENT_3D ( 'NONE', #17718, #1345, #10342 ) ;
#16236 = CYLINDRICAL_SURFACE ( 'NONE', #30196, 3.999999999999998224 ) ;
#16237 = ORIENTED_EDGE ( 'NONE', *, *, #29725, .F. ) ;
#16238 = ORIENTED_EDGE ( 'NONE', *, *, #17174, .F. ) ;
#16239 = EDGE_CURVE ( 'NONE', #28676, #32250, #18107, .T. ) ;
#16240 = CARTESIAN_POINT ( 'NONE',  ( -34.50000000000000000, -113.0140978167139991, -0.6247823525984269599 ) ) ;
#16241 = CARTESIAN_POINT ( 'NONE',  ( 1.799999999999996048, 0.000000000000000000, 0.000000000000000000 ) ) ;
#16242 = CARTESIAN_POINT ( 'NONE',  ( 4.000000000000000000, 4.898587196589412829E-16, 65.00000000000000000 ) ) ;
#16243 = CYLINDRICAL_SURFACE ( 'NONE', #4201, 8.000000000000001776 ) ;
#16244 = AXIS2_PLACEMENT_3D ( 'NONE', #26159, #12478, #23267 ) ;
#16245 = CARTESIAN_POINT ( 'NONE',  ( -35.50000000000000000, -113.9929510916434339, 10.85830208992344303 ) ) ;
#16246 = CIRCLE ( 'NONE', #8773, 4.000000000000000000 ) ;
#16247 = CARTESIAN_POINT ( 'NONE',  ( 70.00000000000001421, 55.12602127901487847, 78.31438535856030114 ) ) ;
#16248 = CARTESIAN_POINT ( 'NONE',  ( 8.000000000000000000, -14.80634052301628145, 8.177498406287162069 ) ) ;
#16249 = CARTESIAN_POINT ( 'NONE',  ( -34.50000000000000000, -112.0154707866092707, 0.9357013553229778235 ) ) ;
#16250 = EDGE_CURVE ( 'NONE', #24147, #14794, #33248, .T. ) ;
#16251 = CARTESIAN_POINT ( 'NONE',  ( -36.31249999999994316, -115.9929510916434481, 14.11852480586265024 ) ) ;
#16252 = CARTESIAN_POINT ( 'NONE',  ( 0.000000000000000000, 0.000000000000000000, -55.89999999999999858 ) ) ;
#16253 = VECTOR ( 'NONE', #7902, 1000.000000000000000 ) ;
#16254 = PLANE ( 'NONE',  #4293 ) ;
#16255 = EDGE_LOOP ( 'NONE', ( #9871, #2562, #13469, #3213 ) ) ;
#16256 = CARTESIAN_POINT ( 'NONE',  ( -38.00000000000000711, -115.9929510916434481, 10.50625754673587053 ) ) ;
#16257 = DIRECTION ( 'NONE',  ( 0.000000000000000000, 0.000000000000000000, 1.000000000000000000 ) ) ;
#16258 = FILL_AREA_STYLE ('',( #2978 ) ) ;
#16259 = DIRECTION ( 'NONE',  ( 0.000000000000000000, 0.000000000000000000, -1.000000000000000000 ) ) ;
#16260 = CARTESIAN_POINT ( 'NONE',  ( 4.000000000000000000, 4.627536653468036720E-16, 55.00000000000000000 ) ) ;
#16261 = ORIENTED_EDGE ( 'NONE', *, *, #25743, .F. ) ;
#16262 = FACE_BOUND ( 'NONE', #6165, .T. ) ;
#16263 = CARTESIAN_POINT ( 'NONE',  ( 0.000000000000000000, -2.710505431213761085E-17, -54.99999999999999289 ) ) ;
#16264 = EDGE_CURVE ( 'NONE', #11433, #27701, #34696, .T. ) ;
#16265 = LINE ( 'NONE', #13591, #32013 ) ;
#16266 = CARTESIAN_POINT ( 'NONE',  ( 8.000000000000000000, 0.000000000000000000, 0.000000000000000000 ) ) ;
#16267 = EDGE_CURVE ( 'NONE', #25177, #12635, #24376, .T. ) ;
#16268 = EDGE_CURVE ( 'NONE', #35594, #34977, #471, .T. ) ;
#16269 = DIRECTION ( 'NONE',  ( -1.000000000000000000, 0.000000000000000000, 0.000000000000000000 ) ) ;
#16270 = DIRECTION ( 'NONE',  ( 1.000000000000000000, 1.836970198721029934E-16, 0.000000000000000000 ) ) ;
#16271 = VERTEX_POINT ( 'NONE', #5300 ) ;
#16272 = VECTOR ( 'NONE', #25712, 1000.000000000000000 ) ;
#16273 = EDGE_LOOP ( 'NONE', ( #21419, #32463, #23836, #25805 ) ) ;
#16274 = CIRCLE ( 'NONE', #9378, 4.872650870659778199 ) ;
#16275 = CARTESIAN_POINT ( 'NONE',  ( 8.000000000000000000, -8.128228055638727412, -16.94522934049221519 ) ) ;
#16276 = CARTESIAN_POINT ( 'NONE',  ( -9.999999999999994671, 0.000000000000000000, 0.000000000000000000 ) ) ;
#16277 = CARTESIAN_POINT ( 'NONE',  ( 5.400000000000071410, 0.9999999999999662492, -52.50000000000000000 ) ) ;
#16278 = ORIENTED_EDGE ( 'NONE', *, *, #8841, .F. ) ;
#16279 = CARTESIAN_POINT ( 'NONE',  ( -39.02454729103295961, -113.2308352781851539, 7.840225545821551734 ) ) ;
#16280 = EDGE_CURVE ( 'NONE', #24774, #7064, #2231, .T. ) ;
#16281 = ORIENTED_EDGE ( 'NONE', *, *, #18394, .F. ) ;
#16282 = EDGE_CURVE ( 'NONE', #20113, #14995, #21185, .T. ) ;
#16283 = ORIENTED_EDGE ( 'NONE', *, *, #19016, .F. ) ;
#16284 = ORIENTED_EDGE ( 'NONE', *, *, #24342, .F. ) ;
#16285 = DIRECTION ( 'NONE',  ( 0.000000000000000000, 0.000000000000000000, -1.000000000000000000 ) ) ;
#16286 = CIRCLE ( 'NONE', #773, 20.00000000000000711 ) ;
#16287 = AXIS2_PLACEMENT_3D ( 'NONE', #22112, #16533, #8775 ) ;
#16288 = DIRECTION ( 'NONE',  ( -1.000000000000000000, 0.000000000000000000, 0.000000000000000000 ) ) ;
#16289 = VERTEX_POINT ( 'NONE', #16612 ) ;
#16290 = ORIENTED_EDGE ( 'NONE', *, *, #5046, .F. ) ;
#16291 = CARTESIAN_POINT ( 'NONE',  ( -3.799999999999999822, 4.382607293638566128E-16, -45.89999999999999858 ) ) ;
#16292 = DIRECTION ( 'NONE',  ( 0.000000000000000000, 0.000000000000000000, 1.000000000000000000 ) ) ;
#16293 = CARTESIAN_POINT ( 'NONE',  ( 55.00000000000000000, 10.00000000000000888, 120.0000000000000000 ) ) ;
#16294 = EDGE_CURVE ( 'NONE', #22225, #21964, #13917, .T. ) ;
#16295 = CIRCLE ( 'NONE', #20897, 47.49900000000001654 ) ;
#16296 = FACE_OUTER_BOUND ( 'NONE', #10232, .T. ) ;
#16297 = DIRECTION ( 'NONE',  ( 0.000000000000000000, 0.000000000000000000, -1.000000000000000000 ) ) ;
#16298 = PRODUCT_RELATED_PRODUCT_CATEGORY ( 'part', '', ( #31654 ) ) ;
#16299 = CARTESIAN_POINT ( 'NONE',  ( -49.99999999999999289, -25.98076211353320275, 78.99999999999992895 ) ) ;
#16300 = ADVANCED_FACE ( 'NONE', ( #27624 ), #20000, .T. ) ;
#16301 = CARTESIAN_POINT ( 'NONE',  ( -35.61121590948313553, -115.9929510916434481, 14.07058620477040733 ) ) ;
#16302 = DIRECTION ( 'NONE',  ( -1.000000000000000000, 0.000000000000000000, 0.000000000000000000 ) ) ;
#16303 = LINE ( 'NONE', #8387, #10169 ) ;
#16304 = CARTESIAN_POINT ( 'NONE',  ( -3.239593890920919428, -13.56862304811759579, -1.200000000000006617 ) ) ;
#16305 = DIRECTION ( 'NONE',  ( -1.000000000000000000, -1.836970198721029934E-16, 0.000000000000000000 ) ) ;
#16306 = APPLICATION_CONTEXT ( 'automotive_design' ) ;
#16307 = AXIS2_PLACEMENT_3D ( 'NONE', #34233, #29005, #26497 ) ;
#16308 = AXIS2_PLACEMENT_3D ( 'NONE', #4609, #4956, #23674 ) ;
#16309 = CARTESIAN_POINT ( 'NONE',  ( -49.99999999999999289, -25.98076211353320275, 92.99999999999991473 ) ) ;
#16310 = DIRECTION ( 'NONE',  ( 0.000000000000000000, 2.543449303551180694E-16, -1.000000000000000000 ) ) ;
#16311 = ORIENTED_EDGE ( 'NONE', *, *, #587, .F. ) ;
#16312 = EDGE_CURVE ( 'NONE', #21466, #22617, #35583, .T. ) ;
#16313 = EDGE_CURVE ( 'NONE', #13102, #33467, #3371, .T. ) ;
#16314 = CARTESIAN_POINT ( 'NONE',  ( -35.99999999999999289, -113.9407375970686758, 3.996475545821551734 ) ) ;
#16315 = CYLINDRICAL_SURFACE ( 'NONE', #15205, 20.00000000000000355 ) ;
#16316 = CYLINDRICAL_SURFACE ( 'NONE', #32007, 9.499000000000000554 ) ;
#16317 = DIRECTION ( 'NONE',  ( -1.000000000000000000, 0.000000000000000000, 0.000000000000000000 ) ) ;
#16318 = ORIENTED_EDGE ( 'NONE', *, *, #5044, .F. ) ;
#16319 = EDGE_LOOP ( 'NONE', ( #1572, #7222, #4624, #755 ) ) ;
#16320 = CARTESIAN_POINT ( 'NONE',  ( -34.49999999999998579, -14.67619866229190961, 76.74125644078588948 ) ) ;
#16321 = DIRECTION ( 'NONE',  ( -1.000000000000000000, -0.000000000000000000, -0.000000000000000000 ) ) ;
#16322 = ORIENTED_EDGE ( 'NONE', *, *, #6823, .F. ) ;
#16323 = VERTEX_POINT ( 'NONE', #6167 ) ;
#16324 = EDGE_CURVE ( 'NONE', #12726, #12194, #22186, .T. ) ;
#16325 = CYLINDRICAL_SURFACE ( 'NONE', #19825, 20.00000000000000355 ) ;
#16326 = CARTESIAN_POINT ( 'NONE',  ( 4.000000000000003553, -13.61301047812905907, -3.268936481846298925 ) ) ;
#16327 = DIRECTION ( 'NONE',  ( 1.000000000000000000, 7.285838599102589797E-17, -5.551115123125782702E-17 ) ) ;
#16328 = CARTESIAN_POINT ( 'NONE',  ( 0.000000000000000000, 0.000000000000000000, -33.50000000000000711 ) ) ;
#16329 = ORIENTED_EDGE ( 'NONE', *, *, #24199, .T. ) ;
#16330 = ORIENTED_EDGE ( 'NONE', *, *, #34208, .F. ) ;
#16331 = CIRCLE ( 'NONE', #234, 4.000000000000000000 ) ;
#16332 = CIRCLE ( 'NONE', #31875, 4.800000000000000711 ) ;
#16333 = DIRECTION ( 'NONE',  ( -1.000000000000000000, 0.000000000000000000, 0.000000000000000000 ) ) ;
#16334 = DIRECTION ( 'NONE',  ( 0.000000000000000000, -0.8443279255020087470, -0.5358267949790065376 ) ) ;
#16335 = ORIENTED_EDGE ( 'NONE', *, *, #31731, .F. ) ;
#16336 = FACE_OUTER_BOUND ( 'NONE', #21986, .T. ) ;
#16337 = EDGE_CURVE ( 'NONE', #15107, #11039, #16780, .T. ) ;
#16338 = AXIS2_PLACEMENT_3D ( 'NONE', #3237, #27555, #2894 ) ;
#16339 = CARTESIAN_POINT ( 'NONE',  ( -34.50000000000000000, -112.0269151300720409, -0.7876962586524208776 ) ) ;
#16340 = ADVANCED_FACE ( 'NONE', ( #3658 ), #27792, .T. ) ;
#16341 = CARTESIAN_POINT ( 'NONE',  ( -38.69949915733018742, -114.9929510916434339, 13.54034599209165712 ) ) ;
#16342 = EDGE_CURVE ( 'NONE', #26461, #23662, #3128, .T. ) ;
#16343 = DIRECTION ( 'NONE',  ( 0.000000000000000000, 0.000000000000000000, -1.000000000000000000 ) ) ;
#16344 = CARTESIAN_POINT ( 'NONE',  ( -37.99999897736218202, -114.9929510916434339, 12.62466071271732915 ) ) ;
#16345 = DIRECTION ( 'NONE',  ( -1.000000000000000000, -0.000000000000000000, 0.000000000000000000 ) ) ;
#16346 = CARTESIAN_POINT ( 'NONE',  ( -34.50000000000000000, -114.9929510916434339, 12.57451923796416082 ) ) ;
#16347 = CARTESIAN_POINT ( 'NONE',  ( -50.00000000000000000, -2.726571689596996976E-14, 114.0000000000000000 ) ) ;
#16348 = FACE_OUTER_BOUND ( 'NONE', #24233, .T. ) ;
#16349 = SURFACE_SIDE_STYLE ('',( #30062 ) ) ;
#16350 = DIRECTION ( 'NONE',  ( -1.000000000000000000, 0.000000000000000000, 0.000000000000000000 ) ) ;
#16351 = DIRECTION ( 'NONE',  ( 1.000000000000000000, 0.000000000000000000, 0.000000000000000000 ) ) ;
#16352 = CARTESIAN_POINT ( 'NONE',  ( 8.000000000000007105, 0.000000000000000000, 0.000000000000000000 ) ) ;
#16353 = VERTEX_POINT ( 'NONE', #25261 ) ;
#16354 = DIRECTION ( 'NONE',  ( 0.000000000000000000, 0.000000000000000000, 1.000000000000000000 ) ) ;
#16355 = ORIENTED_EDGE ( 'NONE', *, *, #21648, .T. ) ;
#16356 = EDGE_CURVE ( 'NONE', #12193, #16096, #17138, .T. ) ;
#16357 = CARTESIAN_POINT ( 'NONE',  ( -34.97545270896703329, -113.2308352781851539, 7.409774454178451819 ) ) ;
#16358 = EDGE_CURVE ( 'NONE', #10989, #29853, #6229, .T. ) ;
#16359 = FACE_BOUND ( 'NONE', #34027, .T. ) ;
#16360 = ORIENTED_EDGE ( 'NONE', *, *, #26464, .F. ) ;
#16361 = ORIENTED_EDGE ( 'NONE', *, *, #25729, .F. ) ;
#16362 = AXIS2_PLACEMENT_3D ( 'NONE', #15209, #1557, #9119 ) ;
#16363 = CARTESIAN_POINT ( 'NONE',  ( -4.000000000000000000, 0.000000000000000000, -32.00000000000000000 ) ) ;
#16364 = AXIS2_PLACEMENT_3D ( 'NONE', #16710, #333, #11329 ) ;
#16365 = DIRECTION ( 'NONE',  ( 1.000000000000000000, 0.000000000000000000, -0.000000000000000000 ) ) ;
#16366 = ORIENTED_EDGE ( 'NONE', *, *, #10550, .F. ) ;
#16367 = CARTESIAN_POINT ( 'NONE',  ( -37.05926240293131713, -111.0000000000000284, 3.621475545821551734 ) ) ;
#16368 = AXIS2_PLACEMENT_3D ( 'NONE', #12932, #34545, #23916 ) ;
#16369 = CARTESIAN_POINT ( 'NONE',  ( 8.000000000000000000, 0.000000000000000000, 0.000000000000000000 ) ) ;
#16370 = DIRECTION ( 'NONE',  ( -1.000000000000000000, -0.000000000000000000, -0.000000000000000000 ) ) ;
#16371 = ORIENTED_EDGE ( 'NONE', *, *, #6168, .F. ) ;
#16372 = ORIENTED_EDGE ( 'NONE', *, *, #3416, .F. ) ;
#16373 = FACE_OUTER_BOUND ( 'NONE', #6141, .T. ) ;
#16374 = CARTESIAN_POINT ( 'NONE',  ( 0.000000000000000000, 51.85248208264518155, 3.914090171286368935 ) ) ;
#16376 = ORIENTED_EDGE ( 'NONE', *, *, #16342, .T. ) ;
#16375 = AXIS2_PLACEMENT_3D ( 'NONE', #32096, #21090, #24172 ) ;
#16377 = EDGE_LOOP ( 'NONE', ( #5025, #9694, #27580, #9710 ) ) ;
#16378 = CARTESIAN_POINT ( 'NONE',  ( -34.50000000000000000, -114.5974311500472567, -2.624782352598442614 ) ) ;
#16379 = CARTESIAN_POINT ( 'NONE',  ( -4.000000000000000000, -2.710505431213761085E-17, 54.99999999999999289 ) ) ;
#16380 = VERTEX_POINT ( 'NONE', #22012 ) ;
#16381 = CARTESIAN_POINT ( 'NONE',  ( -35.50000000000000711, -114.6604609523327838, 9.751889438017201428 ) ) ;
#16382 = EDGE_CURVE ( 'NONE', #30241, #6690, #30831, .T. ) ;
#16383 = CLOSED_SHELL ( 'NONE', ( #24545, #29918, #24065, #33900, #24255, #19593, #6889, #14779, #5526, #18108, #24210, #8605, #27571, #29183, #11842, #22226, #34707, #28660, #35101, #32015, #27196, #35365, #19850, #31699, #10884, #24513, #17335 ) ) ;
#16384 = EDGE_CURVE ( 'NONE', #14413, #28288, #20008, .T. ) ;
#16385 = CARTESIAN_POINT ( 'NONE',  ( -35.98977351030467986, -113.9929510916434339, 14.11852173794918563 ) ) ;
#16386 = CIRCLE ( 'NONE', #17538, 20.00000000000000711 ) ;
#16387 = CARTESIAN_POINT ( 'NONE',  ( 8.000000000000000000, 1.693188892523745936, 15.40623615209872632 ) ) ;
#16388 = CYLINDRICAL_SURFACE ( 'NONE', #11638, 4.000000000000000000 ) ;
#16389 = CARTESIAN_POINT ( 'NONE',  ( -34.50000000000000000, -113.9929510916436470, 10.50625754673586876 ) ) ;
#16390 = CARTESIAN_POINT ( 'NONE',  ( -10.00000000000000178, 0.000000000000000000, 0.000000000000000000 ) ) ;
#16391 = AXIS2_PLACEMENT_3D ( 'NONE', #17332, #34098, #11955 ) ;
#16392 = CARTESIAN_POINT ( 'NONE',  ( -35.50000000000000711, -114.1302255537607095, 9.515717283514957714 ) ) ;
#16393 = LINE ( 'NONE', #33669, #28539 ) ;
#16394 = VECTOR ( 'NONE', #25344, 1000.000000000000000 ) ;
#16395 = CARTESIAN_POINT ( 'NONE',  ( 0.000000000000000000, 2.912696353505820124, 21.80633394113451473 ) ) ;
#16396 = ORIENTED_EDGE ( 'NONE', *, *, #12179, .T. ) ;
#16397 = CARTESIAN_POINT ( 'NONE',  ( 8.000000000000000000, -8.931325931664478190, -16.53603053422218494 ) ) ;
#16398 = DIRECTION ( 'NONE',  ( -1.836970198721029934E-16, 1.000000000000000000, 0.000000000000000000 ) ) ;
#16399 = CARTESIAN_POINT ( 'NONE',  ( 7.999999999999992895, -12.30077720129063934, -50.52416135122095397 ) ) ;
#16400 = VECTOR ( 'NONE', #15640, 1000.000000000000000 ) ;
#16401 = ORIENTED_EDGE ( 'NONE', *, *, #14172, .F. ) ;
#16402 = DIRECTION ( 'NONE',  ( 0.000000000000000000, 0.000000000000000000, 1.000000000000000000 ) ) ;
#16403 = ORIENTED_EDGE ( 'NONE', *, *, #13652, .T. ) ;
#16404 = CARTESIAN_POINT ( 'NONE',  ( -35.50000000000000000, -113.0140978167138712, 0.8752176474013583229 ) ) ;
#16405 = CARTESIAN_POINT ( 'NONE',  ( 55.00000000000000000, -25.98076211353320275, 84.99999999999994316 ) ) ;
#16406 = CARTESIAN_POINT ( 'NONE',  ( -37.74901162816869515, -114.6652019342044042, 5.066024454178449155 ) ) ;
#16407 = CARTESIAN_POINT ( 'NONE',  ( -35.50025087934803736, -114.9929510916434339, 12.63488142334835196 ) ) ;
#16408 = DIRECTION ( 'NONE',  ( 0.000000000000000000, 0.000000000000000000, -1.000000000000000000 ) ) ;
#16409 = ORIENTED_EDGE ( 'NONE', *, *, #24490, .F. ) ;
#16410 = PRESENTATION_STYLE_ASSIGNMENT (( #25249 ) ) ;
#16411 = CIRCLE ( 'NONE', #13556, 4.000000000000000000 ) ;
#16412 = CARTESIAN_POINT ( 'NONE',  ( -35.50000000000000000, -111.0278007905855588, 1.116632271043183078 ) ) ;
#16413 = ORIENTED_EDGE ( 'NONE', *, *, #8140, .F. ) ;
#16414 = ORIENTED_EDGE ( 'NONE', *, *, #3294, .F. ) ;
#16415 = CARTESIAN_POINT ( 'NONE',  ( -36.94073759706868287, -112.0000000000000142, 7.128524454178449155 ) ) ;
#16416 = AXIS2_PLACEMENT_3D ( 'NONE', #28501, #26343, #34260 ) ;
#16417 = AXIS2_PLACEMENT_3D ( 'NONE', #19238, #5582, #33294 ) ;
#16418 = DIRECTION ( 'NONE',  ( -1.783119874454246424E-31, -1.187911941725854497E-31, 1.000000000000000000 ) ) ;
#16419 = ORIENTED_EDGE ( 'NONE', *, *, #11013, .F. ) ;
#16420 = EDGE_LOOP ( 'NONE', ( #27486, #9655, #29977, #16510 ) ) ;
#16421 = CARTESIAN_POINT ( 'NONE',  ( -34.50000000000000000, -113.0140978167139991, -0.6091573525984278481 ) ) ;
#16422 = AXIS2_PLACEMENT_3D ( 'NONE', #22706, #14428, #27620 ) ;
#16423 = CARTESIAN_POINT ( 'NONE',  ( 65.00000000000001421, -31.33892132276156062, 83.40622150580404082 ) ) ;
#16424 = DIRECTION ( 'NONE',  ( -1.000000000000000000, 0.000000000000000000, 0.000000000000000000 ) ) ;
#16425 = CARTESIAN_POINT ( 'NONE',  ( -42.49999999999999289, -26.68172400785662290, 89.21410161513769310 ) ) ;
#16426 = AXIS2_PLACEMENT_3D ( 'NONE', #5405, #16881, #21942 ) ;
#16427 = ADVANCED_FACE ( 'NONE', ( #14261 ), #25440, .T. ) ;
#16428 = CARTESIAN_POINT ( 'NONE',  ( -35.50000000000000000, -113.9929510916434339, 10.50625754673609258 ) ) ;
#16429 = FACE_OUTER_BOUND ( 'NONE', #19165, .T. ) ;
#16430 = CARTESIAN_POINT ( 'NONE',  ( 3.799999999999999822, 0.000000000000000000, -40.89999999999999858 ) ) ;
#16431 = CARTESIAN_POINT ( 'NONE',  ( -34.50000000000000000, -111.0141129414446652, 0.9205922128478062350 ) ) ;
#16432 = CARTESIAN_POINT ( 'NONE',  ( -35.50000000000000000, -114.2600084737790809, 8.524153227862690585 ) ) ;
#16433 = UNCERTAINTY_MEASURE_WITH_UNIT (LENGTH_MEASURE( 1.000000000000000082E-05 ), #31754, 'distance_accuracy_value', 'NONE');
#16434 = DIRECTION ( 'NONE',  ( 1.000000000000000000, -4.336808689941997226E-15, -1.084202172485499306E-15 ) ) ;
#16435 = CARTESIAN_POINT ( 'NONE',  ( 7.999999999999992895, -43.55304910509386218, -28.41006711800031326 ) ) ;
#16436 = AXIS2_PLACEMENT_3D ( 'NONE', #7961, #5632, #32987 ) ;
#16437 = PLANE ( 'NONE',  #8277 ) ;
#16438 = ORIENTED_EDGE ( 'NONE', *, *, #17748, .T. ) ;
#16439 = ADVANCED_FACE ( 'NONE', ( #11569 ), #406, .F. ) ;
#16440 = CARTESIAN_POINT ( 'NONE',  ( -38.00000000000000711, -115.9929510916434481, 12.57451923796417681 ) ) ;
#16441 = CARTESIAN_POINT ( 'NONE',  ( -42.49999999999999289, -12.06135120645816272, 83.49999999999992895 ) ) ;
#16442 = CARTESIAN_POINT ( 'NONE',  ( 7.999999999999992895, 22.82995208772687334, 41.06517797613670950 ) ) ;
#16443 = CARTESIAN_POINT ( 'NONE',  ( 7.999999999999992895, -36.05989434073592292, -30.12041790338657066 ) ) ;
#16444 = ITEM_DEFINED_TRANSFORMATION ( 'NONE', 'NONE', #16707,  #21307 ) ;
#16445 = AXIS2_PLACEMENT_3D ( 'NONE', #15328, #31377, #9233 ) ;
#16446 = CIRCLE ( 'NONE', #11301, 4.000000000000000000 ) ;
#16447 = DIRECTION ( 'NONE',  ( -1.000000000000000000, 0.000000000000000000, 0.000000000000000000 ) ) ;
#16448 = ORIENTED_EDGE ( 'NONE', *, *, #30333, .F. ) ;
#16449 = AXIS2_PLACEMENT_3D ( 'NONE', #3683, #6723, #31213 ) ;
#16450 = CYLINDRICAL_SURFACE ( 'NONE', #17042, 3.999999999999993339 ) ;
#16451 = DIRECTION ( 'NONE',  ( 0.000000000000000000, 0.8090169943749491166, -0.5877852522924710277 ) ) ;
#16452 = CARTESIAN_POINT ( 'NONE',  ( 8.000000000000000000, 0.9861715913087641949, 17.47118961583602115 ) ) ;
#16453 = CARTESIAN_POINT ( 'NONE',  ( 55.00000000000000000, 0.000000000000000000, -5.000000000000011546 ) ) ;
#16454 = ITEM_DEFINED_TRANSFORMATION ( 'NONE', 'NONE', #18437,  #21307 ) ;
#16455 = CARTESIAN_POINT ( 'NONE',  ( 46.00000000000000000, 0.000000000000000000, -11.00000000000000000 ) ) ;
#16456 = DIRECTION ( 'NONE',  ( -1.000000000000000000, 0.000000000000000000, 0.000000000000000000 ) ) ;
#16457 = CIRCLE ( 'NONE', #12436, 0.6000000000000029754 ) ;
#16458 = EDGE_LOOP ( 'NONE', ( #28260, #35393, #21061, #26895 ) ) ;
#16459 = PLANE ( 'NONE',  #11829 ) ;
#16460 = DIRECTION ( 'NONE',  ( -0.000000000000000000, 0.000000000000000000, -1.000000000000000000 ) ) ;
#16461 = CARTESIAN_POINT ( 'NONE',  ( 8.000000000000000000, 6.085920226791238008, -15.78165944574512203 ) ) ;
#16462 = ORIENTED_EDGE ( 'NONE', *, *, #33430, .F. ) ;
#16463 = CARTESIAN_POINT ( 'NONE',  ( -36.11231047232249125, -115.9754527089670262, 5.777725545821551734 ) ) ;
#16464 = ORIENTED_EDGE ( 'NONE', *, *, #13407, .T. ) ;
#16465 = VECTOR ( 'NONE', #8434, 999.9999999999998863 ) ;
#16466 = VERTEX_POINT ( 'NONE', #19650 ) ;
#16467 = ORIENTED_EDGE ( 'NONE', *, *, #2072, .T. ) ;
#16468 = DIRECTION ( 'NONE',  ( 1.000000000000000000, -0.000000000000000000, -0.000000000000000000 ) ) ;
#16469 = VECTOR ( 'NONE', #9735, 1000.000000000000000 ) ;
#16470 = AXIS2_PLACEMENT_3D ( 'NONE', #254, #2448, #2815 ) ;
#16471 = CARTESIAN_POINT ( 'NONE',  ( 8.000000000000007105, 0.000000000000000000, 0.000000000000000000 ) ) ;
#16472 = EDGE_LOOP ( 'NONE', ( #16946, #8624, #16518, #5928, #4174 ) ) ;
#16473 = VECTOR ( 'NONE', #5457, 1000.000000000000000 ) ;
#16474 = EDGE_CURVE ( 'NONE', #26137, #19399, #22537, .T. ) ;
#16475 = LINE ( 'NONE', #35595, #16078 ) ;
#16476 = DIRECTION ( 'NONE',  ( -1.000000000000000000, -1.836970198721029934E-16, -0.000000000000000000 ) ) ;
#16477 = EDGE_CURVE ( 'NONE', #5366, #33371, #24645, .T. ) ;
#16478 = CARTESIAN_POINT ( 'NONE',  ( 0.000000000000000000, 50.95304419620839553, -10.38206564895607897 ) ) ;
#16479 = AXIS2_PLACEMENT_3D ( 'NONE', #27281, #2623, #252 ) ;
#16480 = FACE_BOUND ( 'NONE', #7881, .T. ) ;
#16481 = CARTESIAN_POINT ( 'NONE',  ( 0.000000000000000000, 7.162210897275723021, 51.50439529848832620 ) ) ;
#16482 =( BOUNDED_CURVE ( )  B_SPLINE_CURVE ( 2, ( #17613, #1248, #31138, #20304, #12231, #11687, #6640, #6292, #23022, #3604, #31312, #28971, #34022, #28622, #23385, #6466, #33649, #25568, #12047, #8982, #17435, #28793, #19948, #17792, #14737, #4319, #4142, #28438, #3782, #704, #25749, #17258, #31661, #15084, #25921, #30959, #3972, #1079, #22844, #9348, #23205, #885, #26096, #34197, #9524, #28262, #20486, #11867, #34384, #14552, #1427, #12405, #33841, #9166, #20130, #31499, #22658, #6822, #9705, #20663, #6993, #17968, #15265, #32549, #34558, #1969, #18152, #7883, #35104, #21383, #34925, #4849, #21551, #34735, #24286, #29514, #2164, #2339, #26637, #12944, #23744 ),
 .UNSPECIFIED., .F., .T. ) 
 B_SPLINE_CURVE_WITH_KNOTS ( ( 3, 2, 2, 2, 2, 2, 2, 2, 2, 2, 2, 2, 2, 2, 2, 2, 2, 2, 2, 2, 2, 2, 2, 2, 2, 2, 2, 2, 2, 2, 2, 2, 2, 2, 2, 2, 2, 2, 2, 2, 3 ),
 ( 0.000000000000000000, 0.02500000000000000139, 0.05000000000000000278, 0.07499999999999999722, 0.1000000000000000056, 0.1250000000000000000, 0.1499999999999999944, 0.1749999999999999889, 0.2000000000000000111, 0.2250000000000000056, 0.2500000000000000000, 0.2750000000000000222, 0.2999999999999999889, 0.3250000000000000111, 0.3499999999999999778, 0.3750000000000000000, 0.4000000000000000222, 0.4249999999999999889, 0.4500000000000000111, 0.4749999999999999778, 0.5000000000000000000, 0.5250000000000000222, 0.5500000000000000444, 0.5749999999999999556, 0.5999999999999999778, 0.6250000000000000000, 0.6500000000000000222, 0.6750000000000000444, 0.6999999999999999556, 0.7249999999999999778, 0.7500000000000000000, 0.7750000000000000222, 0.8000000000000000444, 0.8249999999999999556, 0.8499999999999999778, 0.8750000000000000000, 0.9000000000000000222, 0.9250000000000000444, 0.9499999999999999556, 0.9749999999999999778, 1.000000000000000000 ),
 .UNSPECIFIED. ) 
 CURVE ( )  GEOMETRIC_REPRESENTATION_ITEM ( )  RATIONAL_B_SPLINE_CURVE ( ( 1.000000000000000000, 0.9238795325112867385, 1.000000000000000000, 0.9238795325112867385, 1.000000000000000000, 0.9238795325112867385, 1.000000000000000000, 0.9238795325112867385, 1.000000000000000000, 0.9238795325112867385, 1.000000000000000000, 0.9238795325112867385, 1.000000000000000000, 0.9238795325112867385, 1.000000000000000000, 0.9238795325112867385, 1.000000000000000000, 0.9238795325112867385, 1.000000000000000000, 0.9238795325112867385, 1.000000000000000000, 0.9238795325112867385, 1.000000000000000000, 0.9238795325112867385, 1.000000000000000000, 0.9238795325112867385, 1.000000000000000000, 0.9238795325112867385, 1.000000000000000000, 0.9238795325112867385, 1.000000000000000000, 0.9238795325112867385, 1.000000000000000000, 0.9238795325112867385, 1.000000000000000000, 0.9238795325112867385, 1.000000000000000000, 0.9238795325112867385, 1.000000000000000000, 0.9238795325112867385, 1.000000000000000000, 0.9238795325112867385, 1.000000000000000000, 0.9238795325112867385, 1.000000000000000000, 0.9238795325112867385, 1.000000000000000000, 0.9238795325112867385, 1.000000000000000000, 0.9238795325112867385, 1.000000000000000000, 0.9238795325112867385, 1.000000000000000000, 0.9238795325112867385, 1.000000000000000000, 0.9238795325112867385, 1.000000000000000000, 0.9238795325112867385, 1.000000000000000000, 0.9238795325112867385, 1.000000000000000000, 0.9238795325112867385, 1.000000000000000000, 0.9238795325112867385, 1.000000000000000000, 0.9238795325112867385, 1.000000000000000000, 0.9238795325112867385, 1.000000000000000000, 0.9238795325112867385, 1.000000000000000000, 0.9238795325112867385, 1.000000000000000000, 0.9238795325112867385, 1.000000000000000000, 0.9238795325112867385, 1.000000000000000000, 0.9238795325112867385, 1.000000000000000000, 0.9238795325112867385, 1.000000000000000000 ) ) 
 REPRESENTATION_ITEM ( '' )  );
#16483 = DIRECTION ( 'NONE',  ( -1.000000000000000000, 0.000000000000000000, 0.000000000000000000 ) ) ;
#16484 = EDGE_CURVE ( 'NONE', #52, #24250, #22710, .T. ) ;
#16485 = CARTESIAN_POINT ( 'NONE',  ( -38.99879592093640213, -115.9929510916434481, 12.67985367974111277 ) ) ;
#16486 = CARTESIAN_POINT ( 'NONE',  ( 4.000000000000003553, 49.65209126885763169, 15.44894276735568539 ) ) ;
#16487 = EDGE_CURVE ( 'NONE', #2787, #21509, #29844, .T. ) ;
#16488 = DIRECTION ( 'NONE',  ( -1.000000000000000000, 0.000000000000000000, 0.000000000000000000 ) ) ;
#16489 = CIRCLE ( 'NONE', #8425, 19.99999999999999645 ) ;
#16490 = CARTESIAN_POINT ( 'NONE',  ( -2.000000000000001332, -3.278627369596165408E-16, -4.725000000000016520 ) ) ;
#16491 = CARTESIAN_POINT ( 'NONE',  ( 0.000000000000000000, 0.000000000000000000, -50.00000000000000000 ) ) ;
#16492 = CIRCLE ( 'NONE', #11347, 4.000000000000000000 ) ;
#16493 = CARTESIAN_POINT ( 'NONE',  ( -34.49999999999998579, -14.67619866229204284, 93.25874355921412473 ) ) ;
#16494 = DIRECTION ( 'NONE',  ( 0.000000000000000000, -6.938893903907203726E-17, -1.000000000000000000 ) ) ;
#16495 = ORIENTED_EDGE ( 'NONE', *, *, #3094, .F. ) ;
#16496 = CARTESIAN_POINT ( 'NONE',  ( -35.99999999999999289, -113.9407375970686758, 2.496475545821551290 ) ) ;
#16497 = AXIS2_PLACEMENT_3D ( 'NONE', #25714, #1221, #33991 ) ;
#16498 = DIRECTION ( 'NONE',  ( -1.000000000000000000, 0.000000000000000000, 0.000000000000000000 ) ) ;
#16499 = CARTESIAN_POINT ( 'NONE',  ( 8.000000000000000000, -14.80634052301617309, -8.177498406287382338 ) ) ;
#16500 = CIRCLE ( 'NONE', #34937, 4.800000000000000711 ) ;
#16501 = CARTESIAN_POINT ( 'NONE',  ( 50.00005079999998969, 0.000000000000000000, 0.000000000000000000 ) ) ;
#16502 = ORIENTED_EDGE ( 'NONE', *, *, #6251, .T. ) ;
#16503 = ORIENTED_EDGE ( 'NONE', *, *, #33687, .T. ) ;
#16504 = CIRCLE ( 'NONE', #5608, 19.99999999999998579 ) ;
#16505 = DIRECTION ( 'NONE',  ( 0.000000000000000000, 0.000000000000000000, -1.000000000000000000 ) ) ;
#16506 = CARTESIAN_POINT ( 'NONE',  ( -50.00000000000000000, 1.347111479062088405E-15, -11.00000000000000000 ) ) ;
#16507 = ORIENTED_EDGE ( 'NONE', *, *, #24763, .T. ) ;
#16508 = AXIS2_PLACEMENT_3D ( 'NONE', #35382, #10710, #7818 ) ;
#16509 = AXIS2_PLACEMENT_3D ( 'NONE', #24234, #21162, #12897 ) ;
#16510 = ORIENTED_EDGE ( 'NONE', *, *, #6696, .T. ) ;
#16511 = VECTOR ( 'NONE', #17477, 1000.000000000000000 ) ;
#16512 = ADVANCED_FACE ( 'NONE', ( #34070 ), #33274, .T. ) ;
#16513 = DIRECTION ( 'NONE',  ( 1.000000000000000000, -5.339440136655842133E-16, -1.047965281155519420E-16 ) ) ;
#16514 = CARTESIAN_POINT ( 'NONE',  ( 0.000000000000000000, 0.000000000000000000, 0.000000000000000000 ) ) ;
#16515 = CARTESIAN_POINT ( 'NONE',  ( -45.99999999999999289, -2.710505431213684048E-17, -1.540743955509788682E-30 ) ) ;
#16516 = DIRECTION ( 'NONE',  ( 0.000000000000000000, 0.000000000000000000, 1.000000000000000000 ) ) ;
#16517 = AXIS2_PLACEMENT_3D ( 'NONE', #35567, #10528, #16257 ) ;
#16518 = ORIENTED_EDGE ( 'NONE', *, *, #6123, .T. ) ;
#16519 = ORIENTED_EDGE ( 'NONE', *, *, #31720, .T. ) ;
#16520 = AXIS2_PLACEMENT_3D ( 'NONE', #13926, #17314, #22906 ) ;
#16521 = EDGE_CURVE ( 'NONE', #25573, #16289, #31363, .T. ) ;
#16522 = CARTESIAN_POINT ( 'NONE',  ( 0.000000000000000000, -18.62763138773852134, 2.494040418455287345 ) ) ;
#16523 = EDGE_CURVE ( 'NONE', #29235, #19887, #9701, .T. ) ;
#16524 = EDGE_CURVE ( 'NONE', #34014, #30169, #32710, .T. ) ;
#16525 = PLANE ( 'NONE',  #2893 ) ;
#16526 = VERTEX_POINT ( 'NONE', #12099 ) ;
#16527 = DIRECTION ( 'NONE',  ( 0.000000000000000000, -0.3420201433256758738, 0.9396926207859057634 ) ) ;
#16528 = VECTOR ( 'NONE', #12589, 1000.000000000000114 ) ;
#16529 = CARTESIAN_POINT ( 'NONE',  ( -34.50000000000000000, -112.0140978167138712, 0.3752176474015640473 ) ) ;
#16530 = AXIS2_PLACEMENT_3D ( 'NONE', #22140, #24681, #14383 ) ;
#16531 = CARTESIAN_POINT ( 'NONE',  ( -37.51022648969539119, -114.9929510916434339, 14.11852173794918386 ) ) ;
#16532 = CARTESIAN_POINT ( 'NONE',  ( -35.50000000000000000, -113.9929510916433912, 10.50625754673588474 ) ) ;
#16533 = DIRECTION ( 'NONE',  ( -1.000000000000000000, 0.000000000000000000, 0.000000000000000000 ) ) ;
#16534 = ADVANCED_FACE ( 'NONE', ( #9396 ), #20154, .F. ) ;
#16535 = CARTESIAN_POINT ( 'NONE',  ( -35.75562914091914024, -114.9929510916434339, 14.09929883582542409 ) ) ;
#16536 = DIRECTION ( 'NONE',  ( 0.000000000000000000, 0.000000000000000000, -1.000000000000000000 ) ) ;
#16537 = VECTOR ( 'NONE', #22568, 1000.000000000000000 ) ;
#16538 = ADVANCED_FACE ( 'NONE', ( #31054 ), #30706, .T. ) ;
#16539 = PLANE ( 'NONE',  #6894 ) ;
#16540 = CARTESIAN_POINT ( 'NONE',  ( 0.000000000000000000, 0.000000000000000000, 0.000000000000000000 ) ) ;
#16541 = EDGE_CURVE ( 'NONE', #6172, #3694, #16610, .T. ) ;
#16542 = FACE_OUTER_BOUND ( 'NONE', #31049, .T. ) ;
#16543 = DIRECTION ( 'NONE',  ( 1.000000000000000000, -5.339440136655842133E-16, -1.047965281155519420E-16 ) ) ;
#16544 = ORIENTED_EDGE ( 'NONE', *, *, #23861, .T. ) ;
#16545 = LINE ( 'NONE', #8087, #18150 ) ;
#16546 = EDGE_LOOP ( 'NONE', ( #26351, #22609, #13257, #2643 ) ) ;
#16547 = CARTESIAN_POINT ( 'NONE',  ( -34.00000000000000000, -114.0592624029313242, 4.503524454178447378 ) ) ;
#16548 = FACE_BOUND ( 'NONE', #28385, .T. ) ;
#16549 = AXIS2_PLACEMENT_3D ( 'NONE', #12663, #20564, #34627 ) ;
#16550 = ORIENTED_EDGE ( 'NONE', *, *, #14980, .F. ) ;
#16551 = VERTEX_POINT ( 'NONE', #6553 ) ;
#16552 = DIRECTION ( 'NONE',  ( -1.000000000000000000, -0.000000000000000000, 0.000000000000000000 ) ) ;
#16553 = FACE_BOUND ( 'NONE', #3513, .T. ) ;
#16554 = EDGE_LOOP ( 'NONE', ( #35145, #33144, #1512, #26414 ) ) ;
#16555 = CARTESIAN_POINT ( 'NONE',  ( -36.94073759706866156, -111.0000000000000284, 8.628524454178448266 ) ) ;
#16556 = CIRCLE ( 'NONE', #30953, 52.00000000000000711 ) ;
#16557 = VECTOR ( 'NONE', #16685, 1000.000000000000000 ) ;
#16558 = EDGE_CURVE ( 'NONE', #10643, #31978, #11606, .T. ) ;
#16559 = DIRECTION ( 'NONE',  ( -1.000000000000000000, 0.000000000000000000, 0.000000000000000000 ) ) ;
#16560 = DIRECTION ( 'NONE',  ( 1.000000000000000000, -0.000000000000000000, -0.000000000000000000 ) ) ;
#16561 = ORIENTED_EDGE ( 'NONE', *, *, #33902, .F. ) ;
#16563 = ORIENTED_EDGE ( 'NONE', *, *, #31321, .F. ) ;
#16562 = EDGE_CURVE ( 'NONE', #18057, #30963, #25662, .T. ) ;
#16564 = CARTESIAN_POINT ( 'NONE',  ( 1.799999999999996492, -2.775557561562891351E-16, -4.000000000000014211 ) ) ;
#16565 = VECTOR ( 'NONE', #14377, 1000.000000000000000 ) ;
#16566 = SURFACE_SIDE_STYLE ('',( #32961 ) ) ;
#16567 = DIRECTION ( 'NONE',  ( -1.000000000000000000, 0.000000000000000000, -0.000000000000000000 ) ) ;
#16568 = ORIENTED_EDGE ( 'NONE', *, *, #14483, .T. ) ;
#16569 = ORIENTED_EDGE ( 'NONE', *, *, #23143, .T. ) ;
#16570 = CARTESIAN_POINT ( 'NONE',  ( -35.50000000000000000, -112.1946304249441795, 2.703640693953100804 ) ) ;
#16571 = EDGE_CURVE ( 'NONE', #876, #4835, #17160, .T. ) ;
#16572 = DIRECTION ( 'NONE',  ( 0.000000000000000000, 0.000000000000000000, 1.000000000000000000 ) ) ;
#16573 = ORIENTED_EDGE ( 'NONE', *, *, #9946, .F. ) ;
#16574 = EDGE_CURVE ( 'NONE', #26937, #15547, #3399, .T. ) ;
#16575 = CARTESIAN_POINT ( 'NONE',  ( -37.46093750000000711, -114.9929510916434339, 13.11852480586264669 ) ) ;
#16576 = CARTESIAN_POINT ( 'NONE',  ( -35.51674767832922441, -113.9929510916434339, 14.04194344061634325 ) ) ;
#16577 = CARTESIAN_POINT ( 'NONE',  ( 0.000000000000000000, -8.053585752061602321, -46.81126742072033409 ) ) ;
#16578 = VECTOR ( 'NONE', #20432, 1000.000000000000000 ) ;
#16579 = DIRECTION ( 'NONE',  ( 0.000000000000000000, 0.000000000000000000, -1.000000000000000000 ) ) ;
#16580 = CARTESIAN_POINT ( 'NONE',  ( -34.50000000000000000, -113.9929510916433344, 10.50625754673586876 ) ) ;
#16581 = CARTESIAN_POINT ( 'NONE',  ( -39.49999999999999289, -1.387778780781445676E-14, 110.0000000000000000 ) ) ;
#16582 = CARTESIAN_POINT ( 'NONE',  ( -38.00000000000000711, -115.9929510916434481, 10.85830208992306822 ) ) ;
#16583 = CARTESIAN_POINT ( 'NONE',  ( -26.99999999999999289, 3.122849337825751800E-15, 0.000000000000000000 ) ) ;
#16584 = AXIS2_PLACEMENT_3D ( 'NONE', #13394, #31620, #23704 ) ;
#16585 = DIRECTION ( 'NONE',  ( -1.000000000000000000, 0.000000000000000000, 0.000000000000000000 ) ) ;
#16586 = VERTEX_POINT ( 'NONE', #12148 ) ;
#16587 = EDGE_LOOP ( 'NONE', ( #7317, #7925, #25622, #11670 ) ) ;
#16588 = CARTESIAN_POINT ( 'NONE',  ( 65.00000000000001421, -25.98076211353320986, 77.99999999999992895 ) ) ;
#16589 = DIRECTION ( 'NONE',  ( 0.000000000000000000, 1.000000000000000000, 3.497202527569241525E-15 ) ) ;
#16590 = ORIENTED_EDGE ( 'NONE', *, *, #24958, .T. ) ;
#16591 = DIRECTION ( 'NONE',  ( 0.000000000000000000, -0.9980267284282723361, 0.06279051952930260472 ) ) ;
#16592 = VERTEX_POINT ( 'NONE', #27832 ) ;
#16593 = CARTESIAN_POINT ( 'NONE',  ( -35.50000000000000711, -115.1770117227680998, -1.611965039240062181 ) ) ;
#16594 = DIRECTION ( 'NONE',  ( 1.000000000000000000, 0.000000000000000000, 0.000000000000000000 ) ) ;
#16595 = CARTESIAN_POINT ( 'NONE',  ( -37.35495115944176092, -112.9754527089670688, 5.534774454178449155 ) ) ;
#16596 = CARTESIAN_POINT ( 'NONE',  ( 0.000000000000000000, 0.000000000000000000, 0.000000000000000000 ) ) ;
#16597 = EDGE_CURVE ( 'NONE', #33309, #1785, #4600, .T. ) ;
#16598 = ORIENTED_EDGE ( 'NONE', *, *, #10778, .F. ) ;
#16599 = EDGE_CURVE ( 'NONE', #8972, #20300, #1098, .T. ) ;
#16600 = CYLINDRICAL_SURFACE ( 'NONE', #7289, 1.000000000000000888 ) ;
#16601 = CARTESIAN_POINT ( 'NONE',  ( -35.50000000000000000, -117.0140978167138854, -0.5622823525984408377 ) ) ;
#16602 = ORIENTED_EDGE ( 'NONE', *, *, #15044, .F. ) ;
#16603 = VERTEX_POINT ( 'NONE', #15537 ) ;
#16604 = CARTESIAN_POINT ( 'NONE',  ( -36.23083527818512550, -116.0245472910329880, 7.784774454178451819 ) ) ;
#16605 = AXIS2_PLACEMENT_3D ( 'NONE', #6303, #3268, #28451 ) ;
#16606 = PRESENTATION_STYLE_ASSIGNMENT (( #19813 ) ) ;
#16607 = DIRECTION ( 'NONE',  ( -1.000000000000000000, 0.000000000000000000, 0.000000000000000000 ) ) ;
#16608 = ORIENTED_EDGE ( 'NONE', *, *, #27778, .F. ) ;
#16609 = ORIENTED_EDGE ( 'NONE', *, *, #15865, .F. ) ;
#16610 = CIRCLE ( 'NONE', #5126, 14.00000000000000000 ) ;
#16611 = CARTESIAN_POINT ( 'NONE',  ( -34.50000000000000000, -112.0140978167138712, 0.3752176474015640473 ) ) ;
#16612 = CARTESIAN_POINT ( 'NONE',  ( 0.000000000000000000, 16.92083251265334098, -4.460989585140788805 ) ) ;
#16613 = FACE_OUTER_BOUND ( 'NONE', #2154, .T. ) ;
#16614 = CARTESIAN_POINT ( 'NONE',  ( -35.50000000000000000, -113.9929510916434339, 12.57451923796416260 ) ) ;
#16615 = FACE_OUTER_BOUND ( 'NONE', #7569, .T. ) ;
#16616 = EDGE_CURVE ( 'NONE', #1882, #17302, #32140, .T. ) ;
#16617 = LINE ( 'NONE', #3489, #6148 ) ;
#16618 = CARTESIAN_POINT ( 'NONE',  ( -34.50000000000000000, -111.0140978167138570, 0.2502176474015764263 ) ) ;
#16619 = CARTESIAN_POINT ( 'NONE',  ( -37.62254989966453422, -115.9929510916434481, 14.11371147303758278 ) ) ;
#16620 = CARTESIAN_POINT ( 'NONE',  ( 8.000000000000000000, 19.77827456857338007, 2.969824084036535528 ) ) ;
#16621 = CARTESIAN_POINT ( 'NONE',  ( -10.00000000000000178, 0.000000000000000000, 0.000000000000000000 ) ) ;
#16622 = DIRECTION ( 'NONE',  ( 0.000000000000000000, 0.000000000000000000, 1.000000000000000000 ) ) ;
#16623 = ORIENTED_EDGE ( 'NONE', *, *, #5919, .T. ) ;
#16624 = AXIS2_PLACEMENT_3D ( 'NONE', #2652, #29479, #2307 ) ;
#16625 = CARTESIAN_POINT ( 'NONE',  ( -35.50000000000000711, -114.1489256397697289, 9.518467544735724317 ) ) ;
#16626 = FACE_OUTER_BOUND ( 'NONE', #28458, .T. ) ;
#16627 = DIRECTION ( 'NONE',  ( 0.000000000000000000, 0.3090169943749477288, -0.9510565162951534202 ) ) ;
#16628 = ORIENTED_EDGE ( 'NONE', *, *, #14341, .F. ) ;
#16629 = VECTOR ( 'NONE', #8156, 1000.000000000000000 ) ;
#16630 = DIRECTION ( 'NONE',  ( 0.000000000000000000, 0.000000000000000000, -1.000000000000000000 ) ) ;
#16631 = DIRECTION ( 'NONE',  ( 0.000000000000000000, 0.000000000000000000, 1.000000000000000000 ) ) ;
#16632 = CARTESIAN_POINT ( 'NONE',  ( 3.872983346207489852, 0.9999999999999522604, 65.00000000000000000 ) ) ;
#16633 = CARTESIAN_POINT ( 'NONE',  ( 8.000000000000000000, 0.000000000000000000, 0.000000000000000000 ) ) ;
#16634 = CONTEXT_DEPENDENT_SHAPE_REPRESENTATION ( #456, #3483 ) ;
#16635 = CIRCLE ( 'NONE', #24697, 5.000000000000004441 ) ;
#16636 = DIRECTION ( 'NONE',  ( -1.000000000000000000, 0.000000000000000000, 0.000000000000000000 ) ) ;
#16637 = CARTESIAN_POINT ( 'NONE',  ( 3.799999999999999822, -2.710505431213761085E-17, -21.89999999999999858 ) ) ;
#16638 = ORIENTED_EDGE ( 'NONE', *, *, #22179, .T. ) ;
#16639 = EDGE_CURVE ( 'NONE', #13171, #3344, #10875, .T. ) ;
#16640 = DIRECTION ( 'NONE',  ( -1.000000000000000000, -0.000000000000000000, 0.000000000000000000 ) ) ;
#16641 = CARTESIAN_POINT ( 'NONE',  ( -4.000000000000000000, 0.000000000000000000, 65.00000000000000000 ) ) ;
#16642 = DIRECTION ( 'NONE',  ( -1.000000000000000000, -0.000000000000000000, 0.000000000000000000 ) ) ;
#16643 = VERTEX_POINT ( 'NONE', #20939 ) ;
#16644 = CARTESIAN_POINT ( 'NONE',  ( -36.33479806579560289, -113.2509883718313262, 5.308975545821551734 ) ) ;
#16645 = ORIENTED_EDGE ( 'NONE', *, *, #232, .T. ) ;
#16646 = ORIENTED_EDGE ( 'NONE', *, *, #1285, .F. ) ;
#16647 = VERTEX_POINT ( 'NONE', #12322 ) ;
#16648 = CARTESIAN_POINT ( 'NONE',  ( 8.000000000000007105, 0.000000000000000000, 0.000000000000000000 ) ) ;
#16649 = CIRCLE ( 'NONE', #27038, 52.00000000000000711 ) ;
#16650 = ADVANCED_FACE ( 'NONE', ( #31406 ), #23485, .T. ) ;
#16651 = DIRECTION ( 'NONE',  ( 0.000000000000000000, 0.000000000000000000, 1.000000000000000000 ) ) ;
#16652 = CARTESIAN_POINT ( 'NONE',  ( -35.50000000000000711, -114.0743172650041686, 9.508870970061893857 ) ) ;
#16653 = CARTESIAN_POINT ( 'NONE',  ( 7.999999999999992895, 0.000000000000000000, 0.000000000000000000 ) ) ;
#16654 = AXIS2_PLACEMENT_3D ( 'NONE', #1019, #30723, #28738 ) ;
#16655 = CARTESIAN_POINT ( 'NONE',  ( -35.51674767832921731, -114.9929510916434339, 14.04194344061634503 ) ) ;
#16656 = CARTESIAN_POINT ( 'NONE',  ( 3.872983346207489852, 0.9999999999999522604, -52.49999999999999289 ) ) ;
#16657 = AXIS2_PLACEMENT_3D ( 'NONE', #26647, #1978, #7542 ) ;
#16658 = CARTESIAN_POINT ( 'NONE',  ( 50.00005079999998969, 0.000000000000000000, 4.000000000000000000 ) ) ;
#16659 = CARTESIAN_POINT ( 'NONE',  ( 0.000000000000000000, 11.19999565274264519, -10.71350075272062519 ) ) ;
#16660 = CARTESIAN_POINT ( 'NONE',  ( 0.000000000000000000, -2.123073309834833111, -47.45152853935339010 ) ) ;
#16661 = CARTESIAN_POINT ( 'NONE',  ( -39.00000000000000000, -115.9929510916434481, 12.57451923796417681 ) ) ;
#16662 = CARTESIAN_POINT ( 'NONE',  ( 0.000000000000000000, 0.000000000000000000, 0.000000000000000000 ) ) ;
#16663 = CARTESIAN_POINT ( 'NONE',  ( 46.00000000000000000, -25.98076211353320275, 84.99999999999992895 ) ) ;
#16664 = DIRECTION ( 'NONE',  ( 0.000000000000000000, 0.000000000000000000, 1.000000000000000000 ) ) ;
#16665 = LINE ( 'NONE', #642, #20381 ) ;
#16666 = DIRECTION ( 'NONE',  ( -1.174092375852890260E-15, 4.222049128630259891E-16, 1.000000000000000000 ) ) ;
#16667 = DIRECTION ( 'NONE',  ( 0.000000000000000000, 0.000000000000000000, 1.000000000000000000 ) ) ;
#16668 = ORIENTED_EDGE ( 'NONE', *, *, #27778, .T. ) ;
#16669 = AXIS2_PLACEMENT_3D ( 'NONE', #10345, #29613, #21133 ) ;
#16670 = CARTESIAN_POINT ( 'NONE',  ( -36.94073759706868287, -115.9999999999999858, 8.871475545821551734 ) ) ;
#16671 = FACE_OUTER_BOUND ( 'NONE', #33928, .T. ) ;
#16672 = PLANE ( 'NONE',  #30847 ) ;
#16673 = DIRECTION ( 'NONE',  ( -1.000000000000000000, 0.000000000000000000, 0.000000000000000000 ) ) ;
#16674 = EDGE_LOOP ( 'NONE', ( #33476, #34884, #1326, #25946, #24066 ) ) ;
#16675 = VECTOR ( 'NONE', #21407, 1000.000000000000000 ) ;
#16676 = ORIENTED_EDGE ( 'NONE', *, *, #13962, .T. ) ;
#16677 = EDGE_CURVE ( 'NONE', #35493, #31626, #34478, .T. ) ;
#16678 = CARTESIAN_POINT ( 'NONE',  ( 9.714451465470119729E-14, 0.9999999999999870104, -44.50000000000000000 ) ) ;
#16679 = CARTESIAN_POINT ( 'NONE',  ( 8.000000000000000000, 0.000000000000000000, 0.000000000000000000 ) ) ;
#16680 = VERTEX_POINT ( 'NONE', #23293 ) ;
#16681 = ADVANCED_FACE ( 'NONE', ( #9623 ), #31586, .T. ) ;
#16682 = EDGE_LOOP ( 'NONE', ( #16502, #29598, #7524, #8746 ) ) ;
#16683 = CIRCLE ( 'NONE', #1177, 22.00000000000000000 ) ;
#16684 = AXIS2_PLACEMENT_3D ( 'NONE', #20880, #31881, #351 ) ;
#16685 = DIRECTION ( 'NONE',  ( -1.000000000000000000, 0.000000000000000000, 0.000000000000000000 ) ) ;
#16686 = DIRECTION ( 'NONE',  ( 0.000000000000000000, 0.000000000000000000, -1.000000000000000000 ) ) ;
#16687 = EDGE_CURVE ( 'NONE', #19047, #11680, #23501, .T. ) ;
#16688 = APPLICATION_PROTOCOL_DEFINITION ( 'draft international standard', 'automotive_design', 1998, #8695 ) ;
#16689 = LINE ( 'NONE', #10956, #25981 ) ;
#16690 = ORIENTED_EDGE ( 'NONE', *, *, #1316, .F. ) ;
#16691 = VERTEX_POINT ( 'NONE', #4416 ) ;
#16692 = CARTESIAN_POINT ( 'NONE',  ( 7.999999999999992895, 0.000000000000000000, 0.000000000000000000 ) ) ;
#16693 = AXIS2_PLACEMENT_3D ( 'NONE', #16786, #8331, #30838 ) ;
#16694 = LINE ( 'NONE', #14002, #31623 ) ;
#16695 = ORIENTED_EDGE ( 'NONE', *, *, #33921, .T. ) ;
#16696 = LINE ( 'NONE', #28229, #27610 ) ;
#16697 = CARTESIAN_POINT ( 'NONE',  ( -34.50000000000000000, -112.0140978167138712, 0.0002176474015661141945 ) ) ;
#16698 = CARTESIAN_POINT ( 'NONE',  ( -37.88878409051687868, -114.9929510916434339, 14.07058620477052102 ) ) ;
#16699 = CARTESIAN_POINT ( 'NONE',  ( -35.50000000000000000, -113.9929510916434339, 10.50763272073269405 ) ) ;
#16700 = DIRECTION ( 'NONE',  ( -1.000000000000000000, 0.000000000000000000, 0.000000000000000000 ) ) ;
#16701 = VECTOR ( 'NONE', #25827, 1000.000000000000000 ) ;
#16702 = CARTESIAN_POINT ( 'NONE',  ( -34.50000000000000000, -114.9929510916434339, 12.59102132592610523 ) ) ;
#16703 = DIRECTION ( 'NONE',  ( 1.000000000000000000, 0.000000000000000000, 0.000000000000000000 ) ) ;
#16704 = ORIENTED_EDGE ( 'NONE', *, *, #11450, .T. ) ;
#16705 = EDGE_CURVE ( 'NONE', #19242, #31652, #34833, .T. ) ;
#16706 = DIRECTION ( 'NONE',  ( -1.000000000000000000, 4.524158825347490025E-15, 1.174092375852883357E-15 ) ) ;
#16707 = AXIS2_PLACEMENT_3D ( 'NONE', #13828, #17040, #8239 ) ;
#16708 = CARTESIAN_POINT ( 'NONE',  ( 7.999999999999992895, 11.90021268425554624, 45.45261810511217959 ) ) ;
#16709 = CARTESIAN_POINT ( 'NONE',  ( 0.000000000000000000, 0.000000000000000000, -53.39999999999999858 ) ) ;
#16710 = CARTESIAN_POINT ( 'NONE',  ( 8.000000000000000000, 0.000000000000000000, 0.000000000000000000 ) ) ;
#16711 = ORIENTED_EDGE ( 'NONE', *, *, #10818, .T. ) ;
#16712 = FACE_OUTER_BOUND ( 'NONE', #206, .T. ) ;
#16713 = VERTEX_POINT ( 'NONE', #32123 ) ;
#16714 = CARTESIAN_POINT ( 'NONE',  ( -40.02454729103296671, -115.1833782841879525, 3.659774454178448710 ) ) ;
#16715 = DIRECTION ( 'NONE',  ( 1.000000000000000000, -5.339440136655842133E-16, -1.047965281155519420E-16 ) ) ;
#16716 = CARTESIAN_POINT ( 'NONE',  ( -35.50000000000000711, -113.1807644833805426, -1.624782352598427959 ) ) ;
#16717 = ORIENTED_EDGE ( 'NONE', *, *, #35432, .T. ) ;
#16718 = ORIENTED_EDGE ( 'NONE', *, *, #14738, .F. ) ;
#16719 = EDGE_CURVE ( 'NONE', #33549, #28168, #12688, .T. ) ;
#16720 = DIRECTION ( 'NONE',  ( 1.000000000000000000, -0.000000000000000000, -0.000000000000000000 ) ) ;
#16721 = FACE_OUTER_BOUND ( 'NONE', #23628, .T. ) ;
#16722 = EDGE_CURVE ( 'NONE', #26283, #14544, #14290, .T. ) ;
#16723 = EDGE_CURVE ( 'NONE', #3468, #11685, #10304, .T. ) ;
#16724 = ORIENTED_EDGE ( 'NONE', *, *, #17852, .F. ) ;
#16725 = CARTESIAN_POINT ( 'NONE',  ( -35.00000000000000000, -114.0592624029316369, 9.003524454178483793 ) ) ;
#16726 = CARTESIAN_POINT ( 'NONE',  ( 8.000000000000007105, 9.604183132802424083, -5.908880290975567995 ) ) ;
#16727 = EDGE_LOOP ( 'NONE', ( #13441, #16284, #4981, #30471 ) ) ;
#16728 = VERTEX_POINT ( 'NONE', #9975 ) ;
#16729 = DIRECTION ( 'NONE',  ( 0.000000000000000000, 0.000000000000000000, 1.000000000000000000 ) ) ;
#16730 = ADVANCED_FACE ( 'NONE', ( #18251 ), #29255, .T. ) ;
#16731 = VECTOR ( 'NONE', #25717, 1000.000000000000000 ) ;
#16732 = AXIS2_PLACEMENT_3D ( 'NONE', #23389, #9708, #17970 ) ;
#16733 = EDGE_CURVE ( 'NONE', #2158, #32986, #6739, .T. ) ;
#16734 = CARTESIAN_POINT ( 'NONE',  ( -34.49999999999998579, -1.387778780781445676E-14, 106.0000000000000000 ) ) ;
#16735 = VERTEX_POINT ( 'NONE', #6918 ) ;
#16736 = ORIENTED_EDGE ( 'NONE', *, *, #24272, .F. ) ;
#16737 = CARTESIAN_POINT ( 'NONE',  ( -34.50000000000000000, -117.0140978167138854, 0.8752176474015623819 ) ) ;
#16738 = PRODUCT_DEFINITION_SHAPE ( 'NONE', 'NONE',  #35640 ) ;
#16739 = DIRECTION ( 'NONE',  ( -1.000000000000000000, 5.339440136655842133E-16, 1.047965281155519420E-16 ) ) ;
#16740 = ORIENTED_EDGE ( 'NONE', *, *, #23566, .F. ) ;
#16741 = CARTESIAN_POINT ( 'NONE',  ( -35.51597953369718397, -114.9929510916434339, 12.74811950270164473 ) ) ;
#16742 = CARTESIAN_POINT ( 'NONE',  ( -37.24999999999992184, -113.9929510916434339, 14.11852480586265024 ) ) ;
#16743 = CARTESIAN_POINT ( 'NONE',  ( 0.000000000000000000, -2.710505431213761085E-17, -30.90000000000000568 ) ) ;
#16744 = DIRECTION ( 'NONE',  ( 0.000000000000000000, 0.000000000000000000, -1.000000000000000000 ) ) ;
#16745 = CARTESIAN_POINT ( 'NONE',  ( -34.50000000000000000, -113.9929510916434339, 10.85830208992344303 ) ) ;
#16746 = CARTESIAN_POINT ( 'NONE',  ( -38.92341863475394348, -114.9929510916434339, 13.10177712753322155 ) ) ;
#16747 = EDGE_CURVE ( 'NONE', #7350, #33826, #30403, .T. ) ;
#16748 = CARTESIAN_POINT ( 'NONE',  ( -38.00000000000000711, -115.9929510916434481, 11.91443571948719615 ) ) ;
#16749 = DIRECTION ( 'NONE',  ( 0.000000000000000000, 0.000000000000000000, -1.000000000000000000 ) ) ;
#16750 = LINE ( 'NONE', #32803, #30206 ) ;
#16751 = ORIENTED_EDGE ( 'NONE', *, *, #23119, .F. ) ;
#16752 = EDGE_CURVE ( 'NONE', #17047, #16735, #7417, .T. ) ;
#16753 = ORIENTED_EDGE ( 'NONE', *, *, #27515, .T. ) ;
#16754 = ADVANCED_FACE ( 'NONE', ( #28889 ), #26186, .T. ) ;
#16755 =( GEOMETRIC_REPRESENTATION_CONTEXT ( 3 ) GLOBAL_UNCERTAINTY_ASSIGNED_CONTEXT ( ( #13644 ) ) GLOBAL_UNIT_ASSIGNED_CONTEXT ( ( #23439, #20712, #29015 ) ) REPRESENTATION_CONTEXT ( 'NONE', 'WORKASPACE' ) );
#16756 = DIRECTION ( 'NONE',  ( 0.000000000000000000, 0.000000000000000000, -1.000000000000000000 ) ) ;
#16757 = AXIS2_PLACEMENT_3D ( 'NONE', #1387, #17219, #12011 ) ;
#16758 = DIRECTION ( 'NONE',  ( -1.000000000000000000, 0.000000000000000000, -0.000000000000000000 ) ) ;
#16759 = ORIENTED_EDGE ( 'NONE', *, *, #1169, .F. ) ;
#16760 = DIRECTION ( 'NONE',  ( -1.000000000000000000, -0.000000000000000000, 0.000000000000000000 ) ) ;
#16761 = EDGE_LOOP ( 'NONE', ( #20864, #27345, #4544, #307 ) ) ;
#16762 = CARTESIAN_POINT ( 'NONE',  ( -35.50000000000000711, -115.8878449012421754, -1.128496220799388494 ) ) ;
#16763 = DIRECTION ( 'NONE',  ( 0.000000000000000000, -0.6845471059286951654, 0.7289686274214054462 ) ) ;
#16764 = CARTESIAN_POINT ( 'NONE',  ( -37.97545270896701908, -113.5265240346955977, 8.347274454178448266 ) ) ;
#16765 = ADVANCED_FACE ( 'NONE', ( #19305 ), #22017, .T. ) ;
#16766 = ADVANCED_FACE ( 'NONE', ( #29963, #24377, #27261 ), #32660, .T. ) ;
#16767 = CARTESIAN_POINT ( 'NONE',  ( -55.00000000000000000, 0.000000000000000000, 64.00000000000000000 ) ) ;
#16768 = VERTEX_POINT ( 'NONE', #7801 ) ;
#16769 = CARTESIAN_POINT ( 'NONE',  ( 8.000000000000007105, -5.363026430117032284, -9.919332006307277183 ) ) ;
#16770 = CARTESIAN_POINT ( 'NONE',  ( -35.50000000000000711, -113.0106174888879877, 1.881901162060937827 ) ) ;
#16771 = ORIENTED_EDGE ( 'NONE', *, *, #20399, .F. ) ;
#16772 = ORIENTED_EDGE ( 'NONE', *, *, #21195, .T. ) ;
#16773 = CARTESIAN_POINT ( 'NONE',  ( -38.45611840935523418, -115.3723087153909432, 5.066024454178449155 ) ) ;
#16774 = SURFACE_SIDE_STYLE ('',( #28133 ) ) ;
#16775 = EDGE_CURVE ( 'NONE', #14055, #5329, #18903, .T. ) ;
#16776 = CARTESIAN_POINT ( 'NONE',  ( 8.000000000000000000, 6.085920226791021292, 15.78165944574522861 ) ) ;
#16777 = ORIENTED_EDGE ( 'NONE', *, *, #6183, .F. ) ;
#16778 = EDGE_LOOP ( 'NONE', ( #3291, #26670, #2246, #21114 ) ) ;
#16779 = CARTESIAN_POINT ( 'NONE',  ( -34.50000000000000000, -115.0140978167137860, -0.6411448143358557950 ) ) ;
#16780 = LINE ( 'NONE', #33187, #23481 ) ;
#16781 = VECTOR ( 'NONE', #6600, 1000.000000000000000 ) ;
#16782 =( GEOMETRIC_REPRESENTATION_CONTEXT ( 3 ) GLOBAL_UNCERTAINTY_ASSIGNED_CONTEXT ( ( #20312 ) ) GLOBAL_UNIT_ASSIGNED_CONTEXT ( ( #8983, #8634, #2742 ) ) REPRESENTATION_CONTEXT ( 'NONE', 'WORKASPACE' ) );
#16783 = AXIS2_PLACEMENT_3D ( 'NONE', #16471, #2646, #21887 ) ;
#16784 = DIRECTION ( 'NONE',  ( 0.000000000000000000, 0.000000000000000000, 1.000000000000000000 ) ) ;
#16785 = CARTESIAN_POINT ( 'NONE',  ( -35.50000000000000000, -113.9929510916434339, 10.56126450660895699 ) ) ;
#16786 = CARTESIAN_POINT ( 'NONE',  ( 8.000000000000000000, -0.3212489022564151142, -16.91141623315864706 ) ) ;
#16787 = DIRECTION ( 'NONE',  ( -1.000000000000000000, -0.000000000000000000, -0.000000000000000000 ) ) ;
#16788 = CARTESIAN_POINT ( 'NONE',  ( -34.50000000000000000, -111.8727710936879589, 2.535339294948415922 ) ) ;
#16789 = EDGE_CURVE ( 'NONE', #32720, #35265, #18336, .T. ) ;
#16790 = CARTESIAN_POINT ( 'NONE',  ( -35.50000000000000000, -114.2114213871176958, 8.518137620934190579 ) ) ;
#16791 = CARTESIAN_POINT ( 'NONE',  ( 0.000000000000000000, 9.744342220504046637, -46.48873837489789196 ) ) ;
#16792 = AXIS2_PLACEMENT_3D ( 'NONE', #10358, #35380, #24926 ) ;
#16793 = ADVANCED_BREP_SHAPE_REPRESENTATION ( '', ( #10370, #21307 ), #30547 ) ;
#16794 = EDGE_CURVE ( 'NONE', #10255, #9519, #10511, .T. ) ;
#16795 = DIRECTION ( 'NONE',  ( -1.000000000000000000, 0.000000000000000000, 0.000000000000000000 ) ) ;
#16796 = VERTEX_POINT ( 'NONE', #21840 ) ;
#16797 = CYLINDRICAL_SURFACE ( 'NONE', #12523, 52.00000000000000711 ) ;
#16798 = FACE_OUTER_BOUND ( 'NONE', #1517, .T. ) ;
#16799 = DIRECTION ( 'NONE',  ( -1.000000000000000000, -0.000000000000000000, -0.000000000000000000 ) ) ;
#16800 = VERTEX_POINT ( 'NONE', #24736 ) ;
#16801 = DIRECTION ( 'NONE',  ( 0.000000000000000000, 0.000000000000000000, 1.000000000000000000 ) ) ;
#16802 = CYLINDRICAL_SURFACE ( 'NONE', #14105, 20.00000000000000355 ) ;
#16803 = CIRCLE ( 'NONE', #1297, 10.99999999999999645 ) ;
#16804 = DIRECTION ( 'NONE',  ( -1.000000000000000000, 0.000000000000000000, 0.000000000000000000 ) ) ;
#16805 = CARTESIAN_POINT ( 'NONE',  ( 7.999999999999992895, 35.20873326984081331, 31.88259874184044662 ) ) ;
#16806 = ADVANCED_FACE ( 'NONE', ( #13395 ), #27445, .T. ) ;
#16807 = ITEM_DEFINED_TRANSFORMATION ( 'NONE', 'NONE', #23645,  #21307 ) ;
#16808 = EDGE_CURVE ( 'NONE', #19005, #3555, #3969, .T. ) ;
#16809 = CARTESIAN_POINT ( 'NONE',  ( 0.000000000000000000, 0.000000000000000000, -55.00000000000000000 ) ) ;
#16810 = LINE ( 'NONE', #30863, #34885 ) ;
#16811 = ORIENTED_EDGE ( 'NONE', *, *, #8709, .T. ) ;
#16812 = DIRECTION ( 'NONE',  ( -1.000000000000000000, -0.000000000000000000, -0.000000000000000000 ) ) ;
#16813 = CARTESIAN_POINT ( 'NONE',  ( 8.000000000000000000, 0.000000000000000000, 0.000000000000000000 ) ) ;
#16814 = DIRECTION ( 'NONE',  ( 0.000000000000000000, 0.000000000000000000, -1.000000000000000000 ) ) ;
#16815 = ORIENTED_EDGE ( 'NONE', *, *, #30436, .F. ) ;
#16816 = CARTESIAN_POINT ( 'NONE',  ( -36.94073759706868287, -115.0000000000000000, 2.871475545821551290 ) ) ;
#16817 = ORIENTED_EDGE ( 'NONE', *, *, #14281, .T. ) ;
#16819 = ORIENTED_EDGE ( 'NONE', *, *, #16523, .F. ) ;
#16818 = CIRCLE ( 'NONE', #3043, 44.99999999999999289 ) ;
#16820 = ORIENTED_EDGE ( 'NONE', *, *, #21344, .T. ) ;
#16821 = DIRECTION ( 'NONE',  ( -1.000000000000000000, 1.734723475976807094E-16, 0.000000000000000000 ) ) ;
#16822 = CIRCLE ( 'NONE', #5908, 20.00000000000000355 ) ;
#16823 = AXIS2_PLACEMENT_3D ( 'NONE', #25280, #22736, #17152 ) ;
#16824 = DIRECTION ( 'NONE',  ( 0.000000000000000000, 0.000000000000000000, 1.000000000000000000 ) ) ;
#16825 = FACE_OUTER_BOUND ( 'NONE', #24600, .T. ) ;
#16826 = CIRCLE ( 'NONE', #4782, 0.04099999999999958539 ) ;
#16827 = CARTESIAN_POINT ( 'NONE',  ( 0.000000000000000000, 0.000000000000000000, 0.000000000000000000 ) ) ;
#16828 = CIRCLE ( 'NONE', #27222, 52.00000000000000711 ) ;
#16829 = DIRECTION ( 'NONE',  ( 0.000000000000000000, 0.6427876096865349220, 0.7660444431189816772 ) ) ;
#16830 = AXIS2_PLACEMENT_3D ( 'NONE', #6909, #20208, #3512 ) ;
#16831 = LINE ( 'NONE', #27668, #11378 ) ;
#16832 = CARTESIAN_POINT ( 'NONE',  ( -34.50000000000000000, -114.9922651054798308, 10.46846006712531008 ) ) ;
#16833 = CARTESIAN_POINT ( 'NONE',  ( 7.999999999999992895, 8.053585752062575764, -46.81126742072014224 ) ) ;
#16834 = EDGE_CURVE ( 'NONE', #1779, #41, #5654, .T. ) ;
#16835 = UNCERTAINTY_MEASURE_WITH_UNIT (LENGTH_MEASURE( 1.000000000000000082E-05 ), #29362, 'distance_accuracy_value', 'NONE');
#16836 = CARTESIAN_POINT ( 'NONE',  ( 50.00000000000000000, 20.00000000000001776, 120.0000000000000000 ) ) ;
#16837 = CARTESIAN_POINT ( 'NONE',  ( -35.90191880024782023, -115.9929510916434481, 14.11551573851449071 ) ) ;
#16838 = DIRECTION ( 'NONE',  ( 0.000000000000000000, 0.000000000000000000, -1.000000000000000000 ) ) ;
#16839 = DIRECTION ( 'NONE',  ( -1.000000000000000000, -0.000000000000000000, -0.000000000000000000 ) ) ;
#16840 = AXIS2_PLACEMENT_3D ( 'NONE', #19910, #19564, #20096 ) ;
#16841 = CARTESIAN_POINT ( 'NONE',  ( -3.799999999999999378, 1.782605128514165574E-14, -0.7999999999999996003 ) ) ;
#16842 = DIRECTION ( 'NONE',  ( -1.734723475976806848E-16, -0.8660254037844410391, 0.4999999999999958367 ) ) ;
#16843 = VECTOR ( 'NONE', #29887, 1000.000000000000000 ) ;
#16844 = CARTESIAN_POINT ( 'NONE',  ( 0.000000000000000000, 39.78933988720149273, -24.98727647984960853 ) ) ;
#16845 = ORIENTED_EDGE ( 'NONE', *, *, #11946, .T. ) ;
#16846 = CARTESIAN_POINT ( 'NONE',  ( -38.97545270896704039, -114.8876895276775087, 9.152725545821555286 ) ) ;
#16847 = CARTESIAN_POINT ( 'NONE',  ( 7.999999999999992895, -38.92705108641712286, -27.21837053747841395 ) ) ;
#16848 = LINE ( 'NONE', #22261, #15305 ) ;
#16849 = LINE ( 'NONE', #24977, #13004 ) ;
#16850 = ORIENTED_EDGE ( 'NONE', *, *, #34210, .T. ) ;
#16851 = ORIENTED_EDGE ( 'NONE', *, *, #24109, .T. ) ;
#16852 = UNCERTAINTY_MEASURE_WITH_UNIT (LENGTH_MEASURE( 1.000000000000000082E-05 ), #1291, 'distance_accuracy_value', 'NONE');
#16853 = VECTOR ( 'NONE', #31164, 1000.000000000000000 ) ;
#16854 = CARTESIAN_POINT ( 'NONE',  ( -46.00000000000000000, 0.000000000000000000, 70.00000000000000000 ) ) ;
#16855 = AXIS2_PLACEMENT_3D ( 'NONE', #14524, #17408, #31111 ) ;
#16856 = DIRECTION ( 'NONE',  ( 0.000000000000000000, 0.000000000000000000, 1.000000000000000000 ) ) ;
#16857 = ORIENTED_EDGE ( 'NONE', *, *, #9253, .F. ) ;
#16858 = ORIENTED_EDGE ( 'NONE', *, *, #831, .T. ) ;
#16859 = CYLINDRICAL_SURFACE ( 'NONE', #34801, 7.199999999999994849 ) ;
#16860 = CARTESIAN_POINT ( 'NONE',  ( 0.000000000000000000, -17.06000345190431844, -10.43821259704038695 ) ) ;
#16861 = DIRECTION ( 'NONE',  ( 1.000000000000000000, -0.000000000000000000, 0.000000000000000000 ) ) ;
#16862 = ORIENTED_EDGE ( 'NONE', *, *, #25355, .T. ) ;
#16863 = ORIENTED_EDGE ( 'NONE', *, *, #24154, .F. ) ;
#16864 = AXIS2_PLACEMENT_3D ( 'NONE', #7505, #28945, #24093 ) ;
#16865 = CARTESIAN_POINT ( 'NONE',  ( 3.799999999999999822, 0.000000000000000000, -55.89999999999999858 ) ) ;
#16866 = FACE_OUTER_BOUND ( 'NONE', #25242, .T. ) ;
#16867 = EDGE_LOOP ( 'NONE', ( #15651, #10100, #30250, #4847 ) ) ;
#16868 = DIRECTION ( 'NONE',  ( -1.000000000000000000, 0.000000000000000000, 0.000000000000000000 ) ) ;
#16869 = DIRECTION ( 'NONE',  ( -1.174092375852890260E-15, 4.222049128630259891E-16, 1.000000000000000000 ) ) ;
#16870 = CARTESIAN_POINT ( 'NONE',  ( 7.999999999999992895, 0.000000000000000000, 0.000000000000000000 ) ) ;
#16871 = VECTOR ( 'NONE', #5931, 1000.000000000000000 ) ;
#16872 = EDGE_CURVE ( 'NONE', #26146, #33209, #5304, .T. ) ;
#16873 = CARTESIAN_POINT ( 'NONE',  ( -39.00000000000000711, -114.9929510916434339, 11.21034663311206181 ) ) ;
#16874 = VECTOR ( 'NONE', #13064, 1000.000000000000000 ) ;
#16875 = FACE_OUTER_BOUND ( 'NONE', #28791, .T. ) ;
#16876 = FACE_OUTER_BOUND ( 'NONE', #24453, .T. ) ;
#16877 = CARTESIAN_POINT ( 'NONE',  ( -34.50000000000000000, -114.9929510916434339, 12.39849696637031506 ) ) ;
#16878 = DIRECTION ( 'NONE',  ( 0.000000000000000000, 0.000000000000000000, 1.000000000000000000 ) ) ;
#16879 = LINE ( 'NONE', #8255, #4638 ) ;
#16880 = FACE_OUTER_BOUND ( 'NONE', #31186, .T. ) ;
#16881 = DIRECTION ( 'NONE',  ( -1.000000000000000000, 0.000000000000000000, 0.000000000000000000 ) ) ;
#16882 = CARTESIAN_POINT ( 'NONE',  ( -1.000000000000014655, -4.808326913196006913, 0.000000000000000000 ) ) ;
#16883 = VERTEX_POINT ( 'NONE', #4946 ) ;
#16884 = FACE_OUTER_BOUND ( 'NONE', #29117, .T. ) ;
#16885 = EDGE_LOOP ( 'NONE', ( #25388, #2692, #19421, #18175 ) ) ;
#16886 = EDGE_CURVE ( 'NONE', #5380, #30763, #12014, .T. ) ;
#16887 = CARTESIAN_POINT ( 'NONE',  ( -39.16322519054179452, -116.0794154965774823, 8.066024454178448266 ) ) ;
#16888 = CARTESIAN_POINT ( 'NONE',  ( 1.519999999999993578, 0.000000000000000000, 0.000000000000000000 ) ) ;
#16889 = CARTESIAN_POINT ( 'NONE',  ( -35.50000000000000711, -114.6807644833805000, -1.624782352598427959 ) ) ;
#16890 = ORIENTED_EDGE ( 'NONE', *, *, #22855, .T. ) ;
#16891 = VERTEX_POINT ( 'NONE', #5131 ) ;
#16892 = CYLINDRICAL_SURFACE ( 'NONE', #9661, 4.000000000000000000 ) ;
#16893 = FACE_OUTER_BOUND ( 'NONE', #762, .T. ) ;
#16894 = ORIENTED_EDGE ( 'NONE', *, *, #13263, .F. ) ;
#16895 = DIRECTION ( 'NONE',  ( 1.000000000000000000, 0.000000000000000000, 0.000000000000000000 ) ) ;
#16896 = AXIS2_PLACEMENT_3D ( 'NONE', #34728, #31490, #14907 ) ;
#16897 = CARTESIAN_POINT ( 'NONE',  ( 29.99999999999999645, 10.58300524425836819, 3.000000000000002665 ) ) ;
#16898 = VECTOR ( 'NONE', #13332, 1000.000000000000000 ) ;
#16899 = ORIENTED_EDGE ( 'NONE', *, *, #29338, .F. ) ;
#16900 = EDGE_LOOP ( 'NONE', ( #4972, #7083, #4820, #33974 ) ) ;
#16901 = DIRECTION ( 'NONE',  ( -1.000000000000000000, 0.000000000000000000, 0.000000000000000000 ) ) ;
#16902 = EDGE_CURVE ( 'NONE', #30814, #5963, #8541, .T. ) ;
#16903 = DIRECTION ( 'NONE',  ( -1.000000000000000000, 0.000000000000000000, 0.000000000000000000 ) ) ;
#16904 = VERTEX_POINT ( 'NONE', #62 ) ;
#16905 = ORIENTED_EDGE ( 'NONE', *, *, #2302, .F. ) ;
#16906 = CARTESIAN_POINT ( 'NONE',  ( -35.50000000000000000, -111.1014359431343905, 1.472195201997948510 ) ) ;
#16907 = EDGE_LOOP ( 'NONE', ( #15337, #16097, #8719, #20793 ) ) ;
#16908 = CARTESIAN_POINT ( 'NONE',  ( -36.99999999999989342, -114.9929510916434339, 13.11852480586264669 ) ) ;
#16909 = EDGE_CURVE ( 'NONE', #9660, #13354, #10878, .T. ) ;
#16910 = CARTESIAN_POINT ( 'NONE',  ( -36.07812499999994316, -113.9929510916434339, 14.11852480586265024 ) ) ;
#16911 = EDGE_CURVE ( 'NONE', #7954, #30484, #19134, .T. ) ;
#16912 = CARTESIAN_POINT ( 'NONE',  ( 8.000000000000000000, 14.18878633068169925, -6.236773481717946765 ) ) ;
#16913 = CARTESIAN_POINT ( 'NONE',  ( 7.999999999999992895, 47.49120266317496686, -0.8606222198176971538 ) ) ;
#16914 = ADVANCED_FACE ( 'NONE', ( #16613 ), #24036, .F. ) ;
#16915 = CARTESIAN_POINT ( 'NONE',  ( -34.50120407906360498, -113.9929510916434339, 12.67985367974112343 ) ) ;
#16916 = CARTESIAN_POINT ( 'NONE',  ( -3.239593890920919428, -13.56862304811759579, -1.200000000000006617 ) ) ;
#16917 = CARTESIAN_POINT ( 'NONE',  ( -35.50000000000000711, -114.0650276068786582, 9.507762098804159123 ) ) ;
#16918 = CARTESIAN_POINT ( 'NONE',  ( 0.000000000000000000, 0.000000000000000000, 0.000000000000000000 ) ) ;
#16920 = AXIS2_PLACEMENT_3D ( 'NONE', #6415, #829, #29102 ) ;
#16919 = DIRECTION ( 'NONE',  ( 0.000000000000000000, 0.000000000000000000, 1.000000000000000000 ) ) ;
#16921 = AXIS2_PLACEMENT_3D ( 'NONE', #9329, #34538, #20285 ) ;
#16922 = ORIENTED_EDGE ( 'NONE', *, *, #14395, .F. ) ;
#16923 = VERTEX_POINT ( 'NONE', #18610 ) ;
#16924 = EDGE_CURVE ( 'NONE', #32382, #6142, #30455, .T. ) ;
#16925 = CARTESIAN_POINT ( 'NONE',  ( 0.000000000000000000, 0.5097555531873385615, 19.99350267651958291 ) ) ;
#16926 = DIRECTION ( 'NONE',  ( -1.000000000000000000, -0.000000000000000000, -0.000000000000000000 ) ) ;
#16927 = EDGE_CURVE ( 'NONE', #24505, #26571, #33533, .T. ) ;
#16928 = ORIENTED_EDGE ( 'NONE', *, *, #30333, .T. ) ;
#16929 = FACE_OUTER_BOUND ( 'NONE', #34555, .T. ) ;
#16930 = VERTEX_POINT ( 'NONE', #3130 ) ;
#16931 = CARTESIAN_POINT ( 'NONE',  ( -35.50000000000000000, -115.0140978167138712, -0.6247823525983134951 ) ) ;
#16932 = DIRECTION ( 'NONE',  ( 0.000000000000000000, 0.000000000000000000, -1.000000000000000000 ) ) ;
#16933 = CARTESIAN_POINT ( 'NONE',  ( -38.37230871539094323, -112.5438815906447729, 2.441024454178448710 ) ) ;
#16934 = VERTEX_POINT ( 'NONE', #25623 ) ;
#16935 = CARTESIAN_POINT ( 'NONE',  ( 5.400000000000085620, -1.000000000000049516, 45.00000000000000711 ) ) ;
#16936 = VECTOR ( 'NONE', #12660, 1000.000000000000000 ) ;
#16937 = VERTEX_POINT ( 'NONE', #409 ) ;
#16938 = DIRECTION ( 'NONE',  ( -1.000000000000000000, 0.000000000000000000, 0.000000000000000000 ) ) ;
#16939 = CARTESIAN_POINT ( 'NONE',  ( -35.50000000000000000, -117.0140978167138854, -0.1247823525984438492 ) ) ;
#16940 = VERTEX_POINT ( 'NONE', #11218 ) ;
#16941 = ORIENTED_EDGE ( 'NONE', *, *, #33855, .F. ) ;
#16942 = CARTESIAN_POINT ( 'NONE',  ( -35.02454729103298803, -114.8876895276775087, 6.097274454178449155 ) ) ;
#16943 = EDGE_CURVE ( 'NONE', #20295, #15482, #3310, .T. ) ;
#16944 = DIRECTION ( 'NONE',  ( 0.000000000000000000, -1.000000000000000000, 0.000000000000000000 ) ) ;
#16945 = ORIENTED_EDGE ( 'NONE', *, *, #1369, .F. ) ;
#16946 = ORIENTED_EDGE ( 'NONE', *, *, #16616, .T. ) ;
#16947 = CARTESIAN_POINT ( 'NONE',  ( -34.50000000000000000, -112.9876085932806262, 1.879154677457530065 ) ) ;
#16948 = DIRECTION ( 'NONE',  ( 1.783119874454246424E-31, 1.187911941725854497E-31, -1.000000000000000000 ) ) ;
#16949 = AXIS2_PLACEMENT_3D ( 'NONE', #20601, #1720, #4254 ) ;
#16950 = AXIS2_PLACEMENT_3D ( 'NONE', #27676, #24621, #13807 ) ;
#16951 = EDGE_CURVE ( 'NONE', #8832, #19841, #1692, .T. ) ;
#16952 = ORIENTED_EDGE ( 'NONE', *, *, #10440, .T. ) ;
#16953 = DIRECTION ( 'NONE',  ( -1.000000000000000000, 0.000000000000000000, 0.000000000000000000 ) ) ;
#16954 = VECTOR ( 'NONE', #23548, 1000.000000000000000 ) ;
#16955 = CIRCLE ( 'NONE', #4351, 4.000000000000000000 ) ;
#16956 = EDGE_CURVE ( 'NONE', #15169, #26218, #19822, .T. ) ;
#16957 = CARTESIAN_POINT ( 'NONE',  ( -35.51597953369717686, -113.9929510916434339, 12.74811950270164473 ) ) ;
#16958 = DIRECTION ( 'NONE',  ( 0.000000000000000000, -6.938893903907202493E-17, -1.000000000000000000 ) ) ;
#16959 = ADVANCED_FACE ( 'NONE', ( #6173 ), #31189, .T. ) ;
#16960 = DIRECTION ( 'NONE',  ( 1.000000000000000000, -0.000000000000000000, -0.000000000000000000 ) ) ;
#16961 = ADVANCED_FACE ( 'NONE', ( #14263 ), #24908, .T. ) ;
#16962 = CARTESIAN_POINT ( 'NONE',  ( -34.50000000000000000, -111.2304026862503719, 1.811733666967775713 ) ) ;
#16963 = CARTESIAN_POINT ( 'NONE',  ( -35.50000000000000000, -114.3049001878960240, 8.530677542735578101 ) ) ;
#16964 = CIRCLE ( 'NONE', #31376, 22.00000000000000000 ) ;
#16965 = CARTESIAN_POINT ( 'NONE',  ( 8.000000000000000000, 9.471478019455355835, -14.71414642875945411 ) ) ;
#16966 = DIRECTION ( 'NONE',  ( -1.000000000000000000, 0.000000000000000000, 0.000000000000000000 ) ) ;
#16967 = ORIENTED_EDGE ( 'NONE', *, *, #29728, .T. ) ;
#16968 = FACE_OUTER_BOUND ( 'NONE', #30734, .T. ) ;
#16969 = CARTESIAN_POINT ( 'NONE',  ( 0.000000000000000000, 13.61301047812919762, -3.268936481846202113 ) ) ;
#16970 = DIRECTION ( 'NONE',  ( 0.000000000000000000, 0.000000000000000000, -1.000000000000000000 ) ) ;
#16971 = EDGE_CURVE ( 'NONE', #31067, #28461, #2279, .T. ) ;
#16972 = ORIENTED_EDGE ( 'NONE', *, *, #35222, .F. ) ;
#16973 = FACE_OUTER_BOUND ( 'NONE', #12878, .T. ) ;
#16974 = DIRECTION ( 'NONE',  ( 1.000000000000000000, -0.000000000000000000, -0.000000000000000000 ) ) ;
#16975 = AXIS2_PLACEMENT_3D ( 'NONE', #34856, #29274, #32317 ) ;
#16976 = CARTESIAN_POINT ( 'NONE',  ( -35.50000000000000711, -113.1256619669233885, 1.895633585076891947 ) ) ;
#16977 = FACE_OUTER_BOUND ( 'NONE', #14716, .T. ) ;
#16978 = CARTESIAN_POINT ( 'NONE',  ( 0.000000000000000000, 0.000000000000000000, -0.7999999999999951594 ) ) ;
#16979 = CARTESIAN_POINT ( 'NONE',  ( 0.000000000000000000, 19.44205635905602847, -43.33776004284589334 ) ) ;
#16980 = AXIS2_PLACEMENT_3D ( 'NONE', #26155, #4033, #34452 ) ;
#16981 = AXIS2_PLACEMENT_3D ( 'NONE', #12172, #17021, #23145 ) ;
#16982 = VERTEX_POINT ( 'NONE', #33360 ) ;
#16983 = CIRCLE ( 'NONE', #3215, 20.00000000000000711 ) ;
#16984 = CARTESIAN_POINT ( 'NONE',  ( 7.999999999999992895, 47.32430374665963058, -21.55018039121478424 ) ) ;
#16985 = CARTESIAN_POINT ( 'NONE',  ( 0.000000000000000000, 9.433698091065187086, -1.111908866155128628 ) ) ;
#16986 = DIRECTION ( 'NONE',  ( 0.000000000000000000, 0.000000000000000000, 1.000000000000000000 ) ) ;
#16987 = ORIENTED_EDGE ( 'NONE', *, *, #2408, .T. ) ;
#16988 = CARTESIAN_POINT ( 'NONE',  ( -37.74901162816868805, -113.3347980657955958, 3.433975545821550845 ) ) ;
#16989 = ORIENTED_EDGE ( 'NONE', *, *, #27573, .T. ) ;
#16990 = EDGE_CURVE ( 'NONE', #24314, #27865, #24113, .T. ) ;
#16991 = VECTOR ( 'NONE', #17950, 1000.000000000000114 ) ;
#16992 = VERTEX_POINT ( 'NONE', #3486 ) ;
#16993 = ORIENTED_EDGE ( 'NONE', *, *, #4506, .T. ) ;
#16994 = LINE ( 'NONE', #273, #22355 ) ;
#16995 = APPLICATION_CONTEXT ( 'automotive_design' ) ;
#16996 = EDGE_CURVE ( 'NONE', #25438, #33987, #28137, .T. ) ;
#16997 = CARTESIAN_POINT ( 'NONE',  ( 7.999999999999992895, 0.000000000000000000, 0.000000000000000000 ) ) ;
#16998 = DIRECTION ( 'NONE',  ( 1.000000000000000000, -4.524158825347490025E-15, -1.174092375852883357E-15 ) ) ;
#16999 = CIRCLE ( 'NONE', #7809, 47.49900000000001654 ) ;
#17000 = CARTESIAN_POINT ( 'NONE',  ( -35.50000000000000711, -114.4026847875275337, 9.592046023459676718 ) ) ;
#17001 = DIRECTION ( 'NONE',  ( -1.000000000000000000, 0.000000000000000000, 0.000000000000000000 ) ) ;
#17002 = EDGE_CURVE ( 'NONE', #32244, #4537, #11741, .T. ) ;
#17003 = DIRECTION ( 'NONE',  ( -1.000000000000000000, 0.000000000000000000, 0.000000000000000000 ) ) ;
#17004 = ADVANCED_FACE ( 'NONE', ( #33896 ), #5994, .T. ) ;
#17005 = CIRCLE ( 'NONE', #1506, 20.00000000000000711 ) ;
#17006 = CARTESIAN_POINT ( 'NONE',  ( -34.50000000000000000, -114.1414532730574507, 9.517316564499758158 ) ) ;
#17007 = DIRECTION ( 'NONE',  ( -1.000000000000000000, 0.000000000000000000, -0.000000000000000000 ) ) ;
#17008 = CARTESIAN_POINT ( 'NONE',  ( -34.49999999999998579, -39.90017302060827831, 86.49999999999991473 ) ) ;
#17009 = CARTESIAN_POINT ( 'NONE',  ( -35.50000000000000000, -114.2356323198232673, 8.521029492159460261 ) ) ;
#17010 = CARTESIAN_POINT ( 'NONE',  ( -35.50000000000000711, -113.8159288351371714, 1.978028123174813802 ) ) ;
#17011 = LINE ( 'NONE', #1011, #3003 ) ;
#17012 = AXIS2_PLACEMENT_3D ( 'NONE', #33923, #14996, #20380 ) ;
#17013 = DIRECTION ( 'NONE',  ( 1.541976423090495140E-16, -1.000000000000000000, 0.000000000000000000 ) ) ;
#17014 = AXIS2_PLACEMENT_3D ( 'NONE', #11797, #20239, #472 ) ;
#17015 = CARTESIAN_POINT ( 'NONE',  ( 8.000000000000000000, -0.9861715913086367413, -17.47118961583605312 ) ) ;
#17016 = CARTESIAN_POINT ( 'NONE',  ( -36.49999999999999289, -11.52052244843579309, 115.1848168619253698 ) ) ;
#17017 = CARTESIAN_POINT ( 'NONE',  ( 0.000000000000000000, -46.87740477351715640, 16.82754413119429415 ) ) ;
#17018 = PLANE ( 'NONE',  #4046 ) ;
#17019 = ORIENTED_EDGE ( 'NONE', *, *, #13822, .T. ) ;
#17020 = CARTESIAN_POINT ( 'NONE',  ( -37.74901162816868805, -113.3347980657955958, 3.433975545821550845 ) ) ;
#17021 = DIRECTION ( 'NONE',  ( -1.000000000000000000, 0.000000000000000000, 0.000000000000000000 ) ) ;
#17022 = CARTESIAN_POINT ( 'NONE',  ( -39.49999999999999289, -14.17619866229204106, 93.62476896299857287 ) ) ;
#17023 = CARTESIAN_POINT ( 'NONE',  ( 0.000000000000000000, -13.61301047812919762, 3.268936481846118625 ) ) ;
#17024 = VERTEX_POINT ( 'NONE', #20181 ) ;
#17025 = ORIENTED_EDGE ( 'NONE', *, *, #18767, .F. ) ;
#17026 = CARTESIAN_POINT ( 'NONE',  ( -44.00000000000000000, 1.349783804395672066E-31, 0.000000000000000000 ) ) ;
#17027 = CIRCLE ( 'NONE', #5568, 2.999999999999988898 ) ;
#17028 = DIRECTION ( 'NONE',  ( 0.000000000000000000, 0.000000000000000000, -1.000000000000000000 ) ) ;
#17029 = VERTEX_POINT ( 'NONE', #14086 ) ;
#17030 = VERTEX_POINT ( 'NONE', #25081 ) ;
#17031 = CIRCLE ( 'NONE', #10735, 0.5000000000000004441 ) ;
#17032 = AXIS2_PLACEMENT_3D ( 'NONE', #27508, #21724, #30197 ) ;
#17033 = ADVANCED_FACE ( 'NONE', ( #19653 ), #9046, .T. ) ;
#17034 = AXIS2_PLACEMENT_3D ( 'NONE', #20377, #6369, #3868 ) ;
#17035 = EDGE_CURVE ( 'NONE', #7160, #14413, #2961, .T. ) ;
#17036 = FACE_OUTER_BOUND ( 'NONE', #25446, .T. ) ;
#17037 = VECTOR ( 'NONE', #11453, 1000.000000000000114 ) ;
#17038 = DIRECTION ( 'NONE',  ( 0.000000000000000000, 0.000000000000000000, 1.000000000000000000 ) ) ;
#17039 = AXIS2_PLACEMENT_3D ( 'NONE', #33516, #746, #24722 ) ;
#17040 = DIRECTION ( 'NONE',  ( -1.000000000000000000, 5.551115123125783935E-17, -2.591636264448891671E-18 ) ) ;
#17041 = FACE_OUTER_BOUND ( 'NONE', #7667, .T. ) ;
#17043 = EDGE_LOOP ( 'NONE', ( #35327, #5639 ) ) ;
#17042 = AXIS2_PLACEMENT_3D ( 'NONE', #21322, #18810, #21492 ) ;
#17044 = ORIENTED_EDGE ( 'NONE', *, *, #7697, .T. ) ;
#17045 = LINE ( 'NONE', #16865, #27232 ) ;
#17046 = DIRECTION ( 'NONE',  ( 0.000000000000000000, 0.000000000000000000, -1.000000000000000000 ) ) ;
#17047 = VERTEX_POINT ( 'NONE', #11573 ) ;
#17048 = CARTESIAN_POINT ( 'NONE',  ( 0.000000000000000000, -16.71027810728551799, 2.620268201065888203 ) ) ;
#17049 = AXIS2_PLACEMENT_3D ( 'NONE', #17411, #11838, #8957 ) ;
#17050 = CARTESIAN_POINT ( 'NONE',  ( -34.50000000000000000, -115.0140978167138428, -0.6247823525986679893 ) ) ;
#17051 = CARTESIAN_POINT ( 'NONE',  ( -3.799999999999999822, -2.710505431213761085E-17, -45.10000000000000142 ) ) ;
#17052 = CARTESIAN_POINT ( 'NONE',  ( -34.49999999999998579, -5.633167542791597704, 121.0048025873810218 ) ) ;
#17053 = CARTESIAN_POINT ( 'NONE',  ( -34.50000000000000000, -115.9929492010520846, 10.50058572605509966 ) ) ;
#17054 = DIRECTION ( 'NONE',  ( 1.000000000000000000, -5.339440136655842133E-16, 1.047965281155515476E-16 ) ) ;
#17055 = PLANE ( 'NONE',  #5395 ) ;
#17056 = CARTESIAN_POINT ( 'NONE',  ( -34.50000000000000000, -114.2114213871176958, 8.518137620934190579 ) ) ;
#17057 = CARTESIAN_POINT ( 'NONE',  ( -34.49999999999998579, -25.98076211353322051, 84.99999999999992895 ) ) ;
#17058 = AXIS2_PLACEMENT_3D ( 'NONE', #12068, #12251, #34580 ) ;
#17059 = AXIS2_PLACEMENT_3D ( 'NONE', #25502, #6575, #34317 ) ;
#17060 = DIRECTION ( 'NONE',  ( -1.783119874454246424E-31, -1.187911941725854497E-31, 1.000000000000000000 ) ) ;
#17061 = CIRCLE ( 'NONE', #13643, 8.000000000000007105 ) ;
#17062 = CARTESIAN_POINT ( 'NONE',  ( 0.000000000000000000, -2.710505431213761085E-17, 54.99999999999999289 ) ) ;
#17063 = DIRECTION ( 'NONE',  ( -1.000000000000000000, 0.000000000000000000, 0.000000000000000000 ) ) ;
#17064 = ORIENTED_EDGE ( 'NONE', *, *, #30673, .T. ) ;
#17065 = AXIS2_PLACEMENT_3D ( 'NONE', #20775, #9641, #17910 ) ;
#17066 = CARTESIAN_POINT ( 'NONE',  ( 1.479000000000008530, -3.480549182199860587E-16, -5.016000000000010672 ) ) ;
#17067 = ORIENTED_EDGE ( 'NONE', *, *, #5443, .F. ) ;
#17068 = CIRCLE ( 'NONE', #1652, 4.000000000000000000 ) ;
#17069 = CARTESIAN_POINT ( 'NONE',  ( -40.02454729103296671, -115.1833782841879525, 8.159774454178448266 ) ) ;
#17070 = CARTESIAN_POINT ( 'NONE',  ( -54.99999999999998579, -64.99999999999997158, 120.0000000000000000 ) ) ;
#17071 = CARTESIAN_POINT ( 'NONE',  ( -35.50000000000000711, -112.0140978167138712, -0.5622823525984296245 ) ) ;
#17072 = ORIENTED_EDGE ( 'NONE', *, *, #35203, .F. ) ;
#17073 = ORIENTED_EDGE ( 'NONE', *, *, #25303, .T. ) ;
#17074 = DIRECTION ( 'NONE',  ( -1.000000000000000000, -0.000000000000000000, 0.000000000000000000 ) ) ;
#17075 = CARTESIAN_POINT ( 'NONE',  ( 7.999999999999992895, 39.64889472655782043, -33.64468972902464827 ) ) ;
#17076 = VERTEX_POINT ( 'NONE', #8515 ) ;
#17077 = ADVANCED_FACE ( 'NONE', ( #22542 ), #30494, .T. ) ;
#17078 = CYLINDRICAL_SURFACE ( 'NONE', #7927, 4.999999999999990230 ) ;
#17079 = ORIENTED_EDGE ( 'NONE', *, *, #32873, .F. ) ;
#17080 = ORIENTED_EDGE ( 'NONE', *, *, #9664, .T. ) ;
#17081 = CARTESIAN_POINT ( 'NONE',  ( 8.000000000000000000, 0.000000000000000000, -1.000000000000000000 ) ) ;
#17082 = CIRCLE ( 'NONE', #21698, 22.00000000000000000 ) ;
#17083 = AXIS2_PLACEMENT_3D ( 'NONE', #3332, #28509, #8704 ) ;
#17084 = FACE_OUTER_BOUND ( 'NONE', #20581, .T. ) ;
#17085 = ORIENTED_EDGE ( 'NONE', *, *, #19643, .F. ) ;
#17086 = EDGE_LOOP ( 'NONE', ( #1392, #25636 ) ) ;
#17087 = CARTESIAN_POINT ( 'NONE',  ( -34.50000000000000000, -117.0140978167138854, -0.3122823525984416704 ) ) ;
#17088 = CIRCLE ( 'NONE', #21099, 11.00000000000001066 ) ;
#17089 = EDGE_CURVE ( 'NONE', #14069, #7962, #7052, .T. ) ;
#17090 = CARTESIAN_POINT ( 'NONE',  ( 4.000000000000003553, 50.95304419620839553, -10.38206564895607897 ) ) ;
#17091 = ORIENTED_EDGE ( 'NONE', *, *, #8909, .F. ) ;
#17092 = AXIS2_PLACEMENT_3D ( 'NONE', #16813, #17163, #6372 ) ;
#17093 = CARTESIAN_POINT ( 'NONE',  ( -36.31249999999995026, -114.9929510916434339, 13.11852480586264669 ) ) ;
#17094 = CARTESIAN_POINT ( 'NONE',  ( -38.25557080230232998, -113.9929510916434339, 13.92914543265419525 ) ) ;
#17095 = CARTESIAN_POINT ( 'NONE',  ( -34.49999999999998579, -20.32009476567217376, 72.19543654875880634 ) ) ;
#17096 = LINE ( 'NONE', #30972, #25463 ) ;
#17097 = CARTESIAN_POINT ( 'NONE',  ( -34.50000306791346816, -113.9929510916434339, 12.62875129555796150 ) ) ;
#17098 = CARTESIAN_POINT ( 'NONE',  ( -39.00000000000000711, -114.9929510916434339, 10.85830208992306822 ) ) ;
#17099 = CARTESIAN_POINT ( 'NONE',  ( -35.83891589277640577, -114.9929510916434339, 13.09299768411358222 ) ) ;
#17100 = AXIS2_PLACEMENT_3D ( 'NONE', #25275, #11583, #22913 ) ;
#17101 = LINE ( 'NONE', #8823, #14720 ) ;
#17102 = CYLINDRICAL_SURFACE ( 'NONE', #25034, 4.000000000000000000 ) ;
#17103 = AXIS2_PLACEMENT_3D ( 'NONE', #18171, #4869, #10269 ) ;
#17104 = EDGE_LOOP ( 'NONE', ( #9482, #17209 ) ) ;
#17105 = ORIENTED_EDGE ( 'NONE', *, *, #17350, .F. ) ;
#17106 = VECTOR ( 'NONE', #4332, 1000.000000000000000 ) ;
#17107 = CARTESIAN_POINT ( 'NONE',  ( 0.000000000000000000, -11.19999565274241782, -10.71350075272084545 ) ) ;
#17108 = CARTESIAN_POINT ( 'NONE',  ( -34.49999999999998579, -26.38406014851792847, 79.52301627764165914 ) ) ;
#17109 = CIRCLE ( 'NONE', #9082, 0.5000000000000004441 ) ;
#17110 = ORIENTED_EDGE ( 'NONE', *, *, #5137, .F. ) ;
#17111 = AXIS2_PLACEMENT_3D ( 'NONE', #18868, #15792, #10248 ) ;
#17112 = DIRECTION ( 'NONE',  ( -1.000000000000000000, 0.000000000000000000, -0.000000000000000000 ) ) ;
#17113 = ORIENTED_EDGE ( 'NONE', *, *, #7701, .T. ) ;
#17114 = CARTESIAN_POINT ( 'NONE',  ( -35.50000000000000000, -115.0140978167139707, -0.6247823525984387283 ) ) ;
#17115 = DIRECTION ( 'NONE',  ( -1.000000000000000000, -0.000000000000000000, -0.000000000000000000 ) ) ;
#17116 = CARTESIAN_POINT ( 'NONE',  ( -36.94073759706866156, -113.0000000000000000, 8.628524454178448266 ) ) ;
#17117 = ORIENTED_EDGE ( 'NONE', *, *, #8305, .F. ) ;
#17118 = AXIS2_PLACEMENT_3D ( 'NONE', #530, #28084, #3427 ) ;
#17119 = DIRECTION ( 'NONE',  ( -1.000000000000000000, -1.734723475976807094E-16, -0.000000000000000000 ) ) ;
#17120 = EDGE_LOOP ( 'NONE', ( #20390, #23012 ) ) ;
#17121 = EDGE_CURVE ( 'NONE', #2498, #9312, #25855, .T. ) ;
#17122 = CARTESIAN_POINT ( 'NONE',  ( -35.50000000000000000, -117.0140978167138854, -0.4997823525984417259 ) ) ;
#17123 = ORIENTED_EDGE ( 'NONE', *, *, #3455, .T. ) ;
#17124 = ORIENTED_EDGE ( 'NONE', *, *, #18754, .T. ) ;
#17125 = ADVANCED_FACE ( 'NONE', ( #34790 ), #28493, .T. ) ;
#17126 = CARTESIAN_POINT ( 'NONE',  ( -35.62769128460905677, -115.4561184093552413, 6.191024454178448266 ) ) ;
#17127 = SURFACE_SIDE_STYLE ('',( #25255 ) ) ;
#17128 = DIRECTION ( 'NONE',  ( -1.000000000000000000, 0.000000000000000000, 0.000000000000000000 ) ) ;
#17129 = VERTEX_POINT ( 'NONE', #25806 ) ;
#17130 = EDGE_LOOP ( 'NONE', ( #20152, #34062, #21950, #24822 ) ) ;
#17131 = CARTESIAN_POINT ( 'NONE',  ( -34.50000000000000000, -115.0140978167137860, -0.6247823525984395054 ) ) ;
#17132 = DIRECTION ( 'NONE',  ( 0.000000000000000000, 0.000000000000000000, -1.000000000000000000 ) ) ;
#17133 = VECTOR ( 'NONE', #18528, 1000.000000000000000 ) ;
#17134 = EDGE_CURVE ( 'NONE', #23024, #10424, #29297, .T. ) ;
#17135 = VERTEX_POINT ( 'NONE', #4567 ) ;
#17136 = ORIENTED_EDGE ( 'NONE', *, *, #17378, .T. ) ;
#17137 = CARTESIAN_POINT ( 'NONE',  ( 7.999999999999992895, 6.109652351742432153, -46.58570277113502556 ) ) ;
#17138 = CIRCLE ( 'NONE', #25808, 10.49999999999999645 ) ;
#17139 = CARTESIAN_POINT ( 'NONE',  ( -38.00000068757622529, -113.9929510916434339, 12.61439929482944855 ) ) ;
#17140 = CARTESIAN_POINT ( 'NONE',  ( 8.000000000000007105, -3.975523202427916125, -13.42368113696675636 ) ) ;
#17141 = CARTESIAN_POINT ( 'NONE',  ( 3.799999999999999822, 4.653657836759942730E-16, -33.50000000000000711 ) ) ;
#17142 = AXIS2_PLACEMENT_3D ( 'NONE', #21914, #30208, #18863 ) ;
#17143 = CARTESIAN_POINT ( 'NONE',  ( -34.50000000000000000, -111.0140978167138570, 0.8127176474015720409 ) ) ;
#17144 = CARTESIAN_POINT ( 'NONE',  ( -39.00000000000000000, -115.9929510916434481, 12.50851088611646311 ) ) ;
#17145 = DIRECTION ( 'NONE',  ( 0.000000000000000000, -0.5877852522924624790, -0.8090169943749551118 ) ) ;
#17146 = CARTESIAN_POINT ( 'NONE',  ( -42.49999999999999289, -39.95319397786859383, 75.20096189432314304 ) ) ;
#17147 = FACE_OUTER_BOUND ( 'NONE', #26271, .T. ) ;
#17148 = CARTESIAN_POINT ( 'NONE',  ( -42.49999999999999289, -25.98076211353322051, 84.99999999999992895 ) ) ;
#17149 = CARTESIAN_POINT ( 'NONE',  ( 0.000000000000000000, 5.400000000000113154, 0.000000000000000000 ) ) ;
#17150 = EDGE_CURVE ( 'NONE', #1603, #13726, #16031, .T. ) ;
#17151 = ORIENTED_EDGE ( 'NONE', *, *, #33395, .F. ) ;
#17152 = DIRECTION ( 'NONE',  ( 0.000000000000000000, 0.3420201433256695456, -0.9396926207859079838 ) ) ;
#17153 = DIRECTION ( 'NONE',  ( 1.000000000000000000, 0.000000000000000000, 0.000000000000000000 ) ) ;
#17154 = LINE ( 'NONE', #33733, #2767 ) ;
#17155 = DIRECTION ( 'NONE',  ( 1.000000000000000000, 0.000000000000000000, 0.000000000000000000 ) ) ;
#17156 = AXIS2_PLACEMENT_3D ( 'NONE', #23, #18745, #7587 ) ;
#17157 = FACE_OUTER_BOUND ( 'NONE', #31553, .T. ) ;
#17158 = CARTESIAN_POINT ( 'NONE',  ( 50.00005079999998969, 0.000000000000000000, 0.000000000000000000 ) ) ;
#17159 = ORIENTED_EDGE ( 'NONE', *, *, #16474, .F. ) ;
#17160 = CIRCLE ( 'NONE', #33862, 19.99999999999998579 ) ;
#17161 = DIRECTION ( 'NONE',  ( -1.000000000000000000, 0.000000000000000000, -0.000000000000000000 ) ) ;
#17162 = ADVANCED_FACE ( 'NONE', ( #15502 ), #4375, .T. ) ;
#17163 = DIRECTION ( 'NONE',  ( -1.000000000000000000, 0.000000000000000000, 0.000000000000000000 ) ) ;
#17164 = DIRECTION ( 'NONE',  ( -1.000000000000000000, -0.000000000000000000, -0.000000000000000000 ) ) ;
#17165 = ORIENTED_EDGE ( 'NONE', *, *, #11527, .T. ) ;
#17166 = EDGE_CURVE ( 'NONE', #25611, #16603, #21796, .T. ) ;
#17167 = CARTESIAN_POINT ( 'NONE',  ( -37.05926240293131713, -113.0000000000000000, 6.621475545821551734 ) ) ;
#17168 = EDGE_CURVE ( 'NONE', #21050, #23209, #17184, .T. ) ;
#17169 = ORIENTED_EDGE ( 'NONE', *, *, #11906, .F. ) ;
#17170 = VERTEX_POINT ( 'NONE', #15322 ) ;
#17171 = CIRCLE ( 'NONE', #10288, 8.000000000000007105 ) ;
#17172 = EDGE_LOOP ( 'NONE', ( #23734, #19893 ) ) ;
#17173 = LINE ( 'NONE', #8720, #25254 ) ;
#17174 = EDGE_CURVE ( 'NONE', #26508, #17425, #13191, .T. ) ;
#17175 = CARTESIAN_POINT ( 'NONE',  ( -35.50000000000000711, -115.0795240838853886, -1.623175561345890472 ) ) ;
#17176 = EDGE_CURVE ( 'NONE', #15252, #620, #23526, .T. ) ;
#17177 = CARTESIAN_POINT ( 'NONE',  ( -1.498621416870348888, -3.455569164145799535E-16, -4.980000000000017302 ) ) ;
#17178 = CARTESIAN_POINT ( 'NONE',  ( -35.50000000000000711, -114.9912366357066986, 10.44580456020104720 ) ) ;
#17179 = CARTESIAN_POINT ( 'NONE',  ( 8.000000000000000000, 13.60411018104336023, -12.96676809804134400 ) ) ;
#17180 = AXIS2_PLACEMENT_3D ( 'NONE', #20051, #6389, #16829 ) ;
#17181 = CARTESIAN_POINT ( 'NONE',  ( 0.000000000000000000, -2.710505431213761085E-17, -21.89999999999999858 ) ) ;
#17182 = CARTESIAN_POINT ( 'NONE',  ( -34.50000000000000000, -114.9927795562974069, 10.48735431211914815 ) ) ;
#17183 = DIRECTION ( 'NONE',  ( -1.000000000000000000, -1.836970198721029934E-16, -0.000000000000000000 ) ) ;
#17184 = CIRCLE ( 'NONE', #35070, 5.016000000000010672 ) ;
#17185 = DIRECTION ( 'NONE',  ( -1.000000000000000000, 0.000000000000000000, 0.000000000000000000 ) ) ;
#17186 = VECTOR ( 'NONE', #27597, 1000.000000000000000 ) ;
#17187 = CARTESIAN_POINT ( 'NONE',  ( -35.50000000000000000, -114.2675000158779710, 8.525177020294046670 ) ) ;
#17188 = CARTESIAN_POINT ( 'NONE',  ( -35.50000000000000711, -112.5103839485166333, -1.498529437127682495 ) ) ;
#17189 = EDGE_CURVE ( 'NONE', #19003, #1732, #26416, .T. ) ;
#17190 = DIRECTION ( 'NONE',  ( -1.000000000000000000, 0.000000000000000000, 0.000000000000000000 ) ) ;
#17191 = DIRECTION ( 'NONE',  ( 0.000000000000000000, 0.000000000000000000, -1.000000000000000000 ) ) ;
#17192 = CARTESIAN_POINT ( 'NONE',  ( 0.000000000000000000, 5.363026430117337817, -9.919332006307165273 ) ) ;
#17193 = EDGE_CURVE ( 'NONE', #2106, #4854, #20723, .T. ) ;
#17194 = CARTESIAN_POINT ( 'NONE',  ( 0.000000000000000000, -19.74581912682874929, 48.10512059033386834 ) ) ;
#17195 = DIRECTION ( 'NONE',  ( 0.000000000000000000, 0.000000000000000000, 1.000000000000000000 ) ) ;
#17196 = VERTEX_POINT ( 'NONE', #18029 ) ;
#17197 = EDGE_CURVE ( 'NONE', #31889, #14055, #34446, .T. ) ;
#17198 = CARTESIAN_POINT ( 'NONE',  ( -38.02454729103295961, -113.6450488405582462, 9.340225545821551734 ) ) ;
#17199 = LINE ( 'NONE', #648, #27901 ) ;
#17200 = DIRECTION ( 'NONE',  ( -1.000000000000000000, 0.000000000000000000, 0.000000000000000000 ) ) ;
#17201 = ORIENTED_EDGE ( 'NONE', *, *, #14504, .F. ) ;
#17202 = EDGE_LOOP ( 'NONE', ( #30130, #23241, #11922, #16928, #31038 ) ) ;
#17203 = APPLICATION_CONTEXT ( 'automotive_design' ) ;
#17204 = LINE ( 'NONE', #11293, #32698 ) ;
#17205 = DIRECTION ( 'NONE',  ( -1.000000000000000000, 0.000000000000000000, -0.000000000000000000 ) ) ;
#17206 = ORIENTED_EDGE ( 'NONE', *, *, #24184, .T. ) ;
#17207 = EDGE_CURVE ( 'NONE', #24757, #10144, #4587, .T. ) ;
#17208 = CARTESIAN_POINT ( 'NONE',  ( -39.97545270896702618, -115.3019030900506152, 4.652725545821551734 ) ) ;
#17209 = ORIENTED_EDGE ( 'NONE', *, *, #16951, .F. ) ;
#17210 = EDGE_CURVE ( 'NONE', #33795, #9689, #26334, .T. ) ;
#17211 = CIRCLE ( 'NONE', #33320, 3.799999999999999822 ) ;
#17212 = CARTESIAN_POINT ( 'NONE',  ( 0.000000000000000000, 0.000000000000000000, -55.89999999999999858 ) ) ;
#17213 = DIRECTION ( 'NONE',  ( 0.000000000000000000, 0.000000000000000000, 1.000000000000000000 ) ) ;
#17214 = CIRCLE ( 'NONE', #6305, 52.00000000000000711 ) ;
#17215 = CARTESIAN_POINT ( 'NONE',  ( -34.50000000000000000, -112.0157046079661995, -0.6902086197697556713 ) ) ;
#17216 = CIRCLE ( 'NONE', #1153, 0.5000000000000004441 ) ;
#17217 = SHAPE_DEFINITION_REPRESENTATION ( #12697, #4547 ) ;
#17218 = EDGE_CURVE ( 'NONE', #9695, #9753, #1670, .T. ) ;
#17219 = DIRECTION ( 'NONE',  ( -1.000000000000000000, -0.000000000000000000, -0.000000000000000000 ) ) ;
#17220 = ORIENTED_EDGE ( 'NONE', *, *, #8396, .T. ) ;
#17221 = ORIENTED_EDGE ( 'NONE', *, *, #3178, .T. ) ;
#17222 = CARTESIAN_POINT ( 'NONE',  ( -36.49999999999999289, -10.15468310254180651, 112.5137715831613008 ) ) ;
#17223 = ORIENTED_EDGE ( 'NONE', *, *, #5381, .T. ) ;
#17224 = DIRECTION ( 'NONE',  ( 0.000000000000000000, -1.000000000000000000, 0.000000000000000000 ) ) ;
#17225 = CARTESIAN_POINT ( 'NONE',  ( -34.50000000000000000, -114.9932644833805426, -0.6247823525982824089 ) ) ;
#17226 = DIRECTION ( 'NONE',  ( 0.000000000000000000, 0.000000000000000000, -1.000000000000000000 ) ) ;
#17227 = DIRECTION ( 'NONE',  ( 1.000000000000000000, 0.000000000000000000, 0.000000000000000000 ) ) ;
#17228 = CARTESIAN_POINT ( 'NONE',  ( -34.50000000000000000, -114.2207110452431635, 8.519246492191951958 ) ) ;
#17229 = CIRCLE ( 'NONE', #16669, 19.99999999999998579 ) ;
#17230 = DIRECTION ( 'NONE',  ( 1.000000000000000000, -0.000000000000000000, 0.000000000000000000 ) ) ;
#17231 = CARTESIAN_POINT ( 'NONE',  ( 7.999999999999992895, 13.85708833599969303, 45.43276465116672114 ) ) ;
#17232 = CARTESIAN_POINT ( 'NONE',  ( -34.50000000000000000, -114.2899554544714960, 8.528375582263644006 ) ) ;
#17233 = DIRECTION ( 'NONE',  ( -1.000000000000000000, -0.000000000000000000, 0.000000000000000000 ) ) ;
#17234 = EDGE_CURVE ( 'NONE', #10152, #8438, #14879, .T. ) ;
#17235 = CARTESIAN_POINT ( 'NONE',  ( 8.000000000000000000, 0.000000000000000000, 0.000000000000000000 ) ) ;
#17236 = LINE ( 'NONE', #9328, #10123 ) ;
#17237 = CARTESIAN_POINT ( 'NONE',  ( 4.000000000000000000, 4.898587196589412829E-16, -55.00000000000000000 ) ) ;
#17238 = EDGE_CURVE ( 'NONE', #17029, #21809, #34616, .T. ) ;
#17239 = ORIENTED_EDGE ( 'NONE', *, *, #22902, .T. ) ;
#17240 = DIRECTION ( 'NONE',  ( -1.000000000000000000, 0.000000000000000000, -0.000000000000000000 ) ) ;
#17241 = ORIENTED_EDGE ( 'NONE', *, *, #32117, .T. ) ;
#17242 = VECTOR ( 'NONE', #33213, 999.9999999999998863 ) ;
#17243 = AXIS2_PLACEMENT_3D ( 'NONE', #30602, #16895, #5937 ) ;
#17244 = CARTESIAN_POINT ( 'NONE',  ( -39.97545270896702618, -112.6980969099493990, 8.347274454178448266 ) ) ;
#17245 = CARTESIAN_POINT ( 'NONE',  ( 0.000000000000000000, -0.2227391519113268437, -46.98410307550732057 ) ) ;
#17246 = CARTESIAN_POINT ( 'NONE',  ( -35.50000000000000711, -112.3995503592287690, -1.424448457485529618 ) ) ;
#17247 = ORIENTED_EDGE ( 'NONE', *, *, #24071, .T. ) ;
#17248 = VERTEX_POINT ( 'NONE', #23077 ) ;
#17250 = CARTESIAN_POINT ( 'NONE',  ( 27.00000000000000000, -19.99999999999997868, 0.000000000000000000 ) ) ;
#17249 = PRODUCT_DEFINITION_SHAPE ( 'NONE', 'NONE',  #35628 ) ;
#17251 = DIRECTION ( 'NONE',  ( 1.000000000000000000, 1.734723475976807094E-16, 0.000000000000000000 ) ) ;
#17252 = ORIENTED_EDGE ( 'NONE', *, *, #29587, .F. ) ;
#17253 = EDGE_CURVE ( 'NONE', #33486, #29368, #31369, .T. ) ;
#17254 = ORIENTED_EDGE ( 'NONE', *, *, #18094, .F. ) ;
#17255 = DIRECTION ( 'NONE',  ( 0.000000000000000000, 0.000000000000000000, -1.000000000000000000 ) ) ;
#17256 = VERTEX_POINT ( 'NONE', #11006 ) ;
#17257 = ORIENTED_EDGE ( 'NONE', *, *, #17166, .F. ) ;
#17258 = CARTESIAN_POINT ( 'NONE',  ( -35.02454729103298092, -113.1123104723225055, 5.402725545821551734 ) ) ;
#17259 = AXIS2_PLACEMENT_3D ( 'NONE', #10881, #35028, #32303 ) ;
#17260 = DIRECTION ( 'NONE',  ( 0.000000000000000000, 0.000000000000000000, 1.000000000000000000 ) ) ;
#17261 = CYLINDRICAL_SURFACE ( 'NONE', #25369, 47.49900000000001654 ) ;
#17262 = ORIENTED_EDGE ( 'NONE', *, *, #26167, .F. ) ;
#17263 = ORIENTED_EDGE ( 'NONE', *, *, #31047, .F. ) ;
#17264 = AXIS2_PLACEMENT_3D ( 'NONE', #7679, #23540, #12382 ) ;
#17265 = CARTESIAN_POINT ( 'NONE',  ( -35.50000000000000000, -111.0140978167138570, 0.0002176474015660057743 ) ) ;
#17266 = DIRECTION ( 'NONE',  ( 0.000000000000000000, 0.000000000000000000, 1.000000000000000000 ) ) ;
#17267 = CIRCLE ( 'NONE', #25366, 4.000000000000000000 ) ;
#17268 = STYLED_ITEM ( 'NONE', ( #11434 ), #17621 ) ;
#17269 = ORIENTED_EDGE ( 'NONE', *, *, #7714, .T. ) ;
#17270 = CARTESIAN_POINT ( 'NONE',  ( -35.50000000000000711, -114.9929510916434339, 12.53051367006571581 ) ) ;
#17271 = CARTESIAN_POINT ( 'NONE',  ( -38.99999693208653895, -113.9929510916434339, 12.62875129555797749 ) ) ;
#17272 = CARTESIAN_POINT ( 'NONE',  ( 0.000000000000000000, 0.000000000000000000, -55.89999999999999858 ) ) ;
#17273 = DIRECTION ( 'NONE',  ( -1.000000000000000000, -1.734723475976807094E-16, 0.000000000000000000 ) ) ;
#17274 = CARTESIAN_POINT ( 'NONE',  ( -35.97545865737298953, -113.9929510916434339, 14.11837420659365527 ) ) ;
#17275 = DIRECTION ( 'NONE',  ( 0.000000000000000000, 0.000000000000000000, -1.000000000000000000 ) ) ;
#17276 = CARTESIAN_POINT ( 'NONE',  ( -35.49999931242378892, -114.9929510916434339, 12.61439929482945566 ) ) ;
#17277 = CARTESIAN_POINT ( 'NONE',  ( 0.000000000000000000, 0.000000000000000000, -55.89999999999999858 ) ) ;
#17278 = ORIENTED_EDGE ( 'NONE', *, *, #698, .F. ) ;
#17279 = CARTESIAN_POINT ( 'NONE',  ( -30.00000000000000355, 11.00000000000000000, 1.347111479062088405E-15 ) ) ;
#17280 = CARTESIAN_POINT ( 'NONE',  ( 0.000000000000000000, 0.000000000000000000, -52.50000000000000000 ) ) ;
#17281 = EDGE_CURVE ( 'NONE', #19897, #15074, #22949, .T. ) ;
#17282 = ORIENTED_EDGE ( 'NONE', *, *, #15820, .T. ) ;
#17283 = CARTESIAN_POINT ( 'NONE',  ( -35.50000000000000711, -114.9492820284331742, 10.20776876943783940 ) ) ;
#17284 = ORIENTED_EDGE ( 'NONE', *, *, #8792, .T. ) ;
#17285 = AXIS2_PLACEMENT_3D ( 'NONE', #21224, #25626, #17496 ) ;
#17286 = CARTESIAN_POINT ( 'NONE',  ( 8.000000000000000000, 16.71027810728552154, -2.620268201066000113 ) ) ;
#17287 = CARTESIAN_POINT ( 'NONE',  ( -9.999999999999994671, 0.000000000000000000, 0.000000000000000000 ) ) ;
#17288 = ORIENTED_EDGE ( 'NONE', *, *, #31301, .F. ) ;
#17289 = CARTESIAN_POINT ( 'NONE',  ( 0.000000000000000000, -17.50309955389642269, 43.60271849949356948 ) ) ;
#17290 = VERTEX_POINT ( 'NONE', #32264 ) ;
#17291 = CARTESIAN_POINT ( 'NONE',  ( -35.50000000000000000, -113.0140978167139991, -0.6091573525984278481 ) ) ;
#17292 = DIRECTION ( 'NONE',  ( -1.000000000000000000, 0.000000000000000000, 0.000000000000000000 ) ) ;
#17293 = CARTESIAN_POINT ( 'NONE',  ( -35.62769128460905677, -115.4561184093552413, 1.691024454178448710 ) ) ;
#17294 = CIRCLE ( 'NONE', #21339, 4.800000000000000711 ) ;
#17295 = MECHANICAL_DESIGN_GEOMETRIC_PRESENTATION_REPRESENTATION (  '', ( #23666 ), #27682 ) ;
#17296 = VERTEX_POINT ( 'NONE', #2391 ) ;
#17297 = VECTOR ( 'NONE', #18689, 1000.000000000000000 ) ;
#17298 = CARTESIAN_POINT ( 'NONE',  ( -37.76916472181487450, -111.9754527089670404, 5.534774454178449155 ) ) ;
#17299 = DIRECTION ( 'NONE',  ( -1.783119874454246424E-31, -1.187911941725854497E-31, 1.000000000000000000 ) ) ;
#17300 = CARTESIAN_POINT ( 'NONE',  ( -35.50000000000000000, -114.8474311500471572, -2.624782352598442614 ) ) ;
#17301 = ORIENTED_EDGE ( 'NONE', *, *, #31642, .T. ) ;
#17302 = VERTEX_POINT ( 'NONE', #34983 ) ;
#17303 = CARTESIAN_POINT ( 'NONE',  ( -10.00000000000000000, 0.000000000000000000, 0.000000000000000000 ) ) ;
#17304 = DIRECTION ( 'NONE',  ( -1.000000000000000000, 0.000000000000000000, 0.000000000000000000 ) ) ;
#17305 = ORIENTED_EDGE ( 'NONE', *, *, #9673, .F. ) ;
#17306 = ORIENTED_EDGE ( 'NONE', *, *, #4568, .F. ) ;
#17307 = CARTESIAN_POINT ( 'NONE',  ( -34.50000000000000000, -112.0157046079661995, -0.6902086197697556713 ) ) ;
#17308 = DIRECTION ( 'NONE',  ( -1.000000000000000000, 0.000000000000000000, 0.000000000000000000 ) ) ;
#17309 = ORIENTED_EDGE ( 'NONE', *, *, #4238, .T. ) ;
#17310 = ORIENTED_EDGE ( 'NONE', *, *, #18487, .F. ) ;
#17311 = CARTESIAN_POINT ( 'NONE',  ( 8.000000000000000000, 16.92083251265325572, 4.460989585141031277 ) ) ;
#17312 = CARTESIAN_POINT ( 'NONE',  ( -36.01562499999997158, -113.9929510916434339, 13.11852480586264846 ) ) ;
#17313 = DIRECTION ( 'NONE',  ( 0.000000000000000000, -1.000000000000000000, 0.000000000000000000 ) ) ;
#17314 = DIRECTION ( 'NONE',  ( -1.000000000000000000, -0.000000000000000000, 0.000000000000000000 ) ) ;
#17315 = CIRCLE ( 'NONE', #35168, 5.000000000000011546 ) ;
#17316 = CARTESIAN_POINT ( 'NONE',  ( -35.74814306589956203, -113.9929510916434339, 13.05539834812772781 ) ) ;
#17317 = CARTESIAN_POINT ( 'NONE',  ( -35.50000000000000000, -115.9929510916434481, 11.73841344789270202 ) ) ;
#17318 = DIRECTION ( 'NONE',  ( -1.000000000000000000, -0.000000000000000000, 0.000000000000000000 ) ) ;
#17319 = DIRECTION ( 'NONE',  ( -1.000000000000000000, 0.000000000000000000, 0.000000000000000000 ) ) ;
#17320 = EDGE_CURVE ( 'NONE', #31629, #17346, #20363, .T. ) ;
#17321 = EDGE_CURVE ( 'NONE', #4520, #4231, #6833, .T. ) ;
#17322 = FACE_OUTER_BOUND ( 'NONE', #3780, .T. ) ;
#17323 = CARTESIAN_POINT ( 'NONE',  ( 7.999999999999992895, 42.41764978026606059, -20.20639853260303198 ) ) ;
#17324 = DIRECTION ( 'NONE',  ( 0.000000000000000000, 0.9848077530122073542, 0.1736481776669339117 ) ) ;
#17325 = ORIENTED_EDGE ( 'NONE', *, *, #14115, .F. ) ;
#17326 = DIRECTION ( 'NONE',  ( -1.000000000000000000, 0.000000000000000000, 0.000000000000000000 ) ) ;
#17327 = DIRECTION ( 'NONE',  ( 0.000000000000000000, 0.000000000000000000, -1.000000000000000000 ) ) ;
#17328 = CARTESIAN_POINT ( 'NONE',  ( -35.50000000000000711, -113.3557509229967764, 1.923098431109107054 ) ) ;
#17329 = PLANE ( 'NONE',  #12672 ) ;
#17330 = CONTEXT_DEPENDENT_SHAPE_REPRESENTATION ( #32212, #32261 ) ;
#17331 = EDGE_CURVE ( 'NONE', #28676, #30827, #32168, .T. ) ;
#17332 = CARTESIAN_POINT ( 'NONE',  ( 0.000000000000000000, 0.000000000000000000, -65.00000000000000000 ) ) ;
#17333 = DIRECTION ( 'NONE',  ( -1.000000000000000000, 0.000000000000000000, 0.000000000000000000 ) ) ;
#17334 = ORIENTED_EDGE ( 'NONE', *, *, #24422, .F. ) ;
#17335 = ADVANCED_FACE ( 'NONE', ( #4154 ), #34399, .F. ) ;
#17336 = CARTESIAN_POINT ( 'NONE',  ( 8.000000000000000000, 14.71414642875954648, 9.471478019455206621 ) ) ;
#17337 = FACE_OUTER_BOUND ( 'NONE', #11190, .T. ) ;
#17338 = DIRECTION ( 'NONE',  ( -1.000000000000000000, -0.000000000000000000, 0.000000000000000000 ) ) ;
#17339 = ORIENTED_EDGE ( 'NONE', *, *, #10650, .F. ) ;
#17340 = ORIENTED_EDGE ( 'NONE', *, *, #5838, .T. ) ;
#17341 = CARTESIAN_POINT ( 'NONE',  ( -37.47347596530441649, -113.0245472910329880, 6.527725545821552622 ) ) ;
#17342 = EDGE_LOOP ( 'NONE', ( #1492, #13000 ) ) ;
#17343 = AXIS2_PLACEMENT_3D ( 'NONE', #11004, #32787, #13876 ) ;
#17344 = COLOUR_RGB ( '', 0.09019608, 0.27058824, 0.51372549) ;
#17345 = TOROIDAL_SURFACE ( 'NONE', #16235, 5.015999999999992909, 0.04099999999999925926 ) ;
#17346 = VERTEX_POINT ( 'NONE', #15274 ) ;
#17347 = EDGE_LOOP ( 'NONE', ( #19177, #810 ) ) ;
#17348 = FACE_OUTER_BOUND ( 'NONE', #1435, .T. ) ;
#17349 = CARTESIAN_POINT ( 'NONE',  ( -35.50000000000000711, -116.0140978167138712, -0.1247823525984439463 ) ) ;
#17350 = EDGE_CURVE ( 'NONE', #529, #19681, #17211, .T. ) ;
#17351 = FACE_BOUND ( 'NONE', #30572, .T. ) ;
#17352 = VECTOR ( 'NONE', #18405, 1000.000000000000000 ) ;
#17353 = CARTESIAN_POINT ( 'NONE',  ( -35.50000102263782509, -114.9929510916434339, 12.62466071271731316 ) ) ;
#17354 = CYLINDRICAL_SURFACE ( 'NONE', #26412, 17.49900000000000233 ) ;
#17355 = FACE_OUTER_BOUND ( 'NONE', #16319, .T. ) ;
#17356 = CARTESIAN_POINT ( 'NONE',  ( -34.50000000000000000, -114.1091535596544873, 9.513028657562415447 ) ) ;
#17357 = DIRECTION ( 'NONE',  ( 1.000000000000000000, 0.000000000000000000, 0.000000000000000000 ) ) ;
#17358 = ADVANCED_FACE ( 'NONE', ( #9884 ), #20848, .F. ) ;
#17359 = AXIS2_PLACEMENT_3D ( 'NONE', #21616, #27053, #29399 ) ;
#17360 = EDGE_CURVE ( 'NONE', #25659, #31873, #1711, .T. ) ;
#17361 = DIRECTION ( 'NONE',  ( 0.000000000000000000, 0.000000000000000000, 1.000000000000000000 ) ) ;
#17362 = ORIENTED_EDGE ( 'NONE', *, *, #14972, .T. ) ;
#17363 = EDGE_CURVE ( 'NONE', #9289, #15509, #29889, .T. ) ;
#17364 = CARTESIAN_POINT ( 'NONE',  ( -35.50000000000000000, -115.9926080209513657, 10.46845107750242398 ) ) ;
#17366 = DIRECTION ( 'NONE',  ( 0.000000000000000000, 4.163336342344333240E-14, -1.000000000000000000 ) ) ;
#17365 = CIRCLE ( 'NONE', #1886, 4.000000000000000000 ) ;
#17367 = FACE_OUTER_BOUND ( 'NONE', #7633, .T. ) ;
#17368 = DIRECTION ( 'NONE',  ( -1.174092375852890260E-15, 4.222049128630259891E-16, 1.000000000000000000 ) ) ;
#17369 = CARTESIAN_POINT ( 'NONE',  ( 0.000000000000000000, 0.000000000000000000, 0.000000000000000000 ) ) ;
#17370 = FACE_OUTER_BOUND ( 'NONE', #226, .T. ) ;
#17371 = CYLINDRICAL_SURFACE ( 'NONE', #7280, 20.00000000000000355 ) ;
#17372 = FACE_OUTER_BOUND ( 'NONE', #14253, .T. ) ;
#17373 = ORIENTED_EDGE ( 'NONE', *, *, #23577, .T. ) ;
#17374 = EDGE_CURVE ( 'NONE', #33223, #6287, #27003, .T. ) ;
#17375 = CARTESIAN_POINT ( 'NONE',  ( -37.47347596530441649, -113.0245472910329880, 5.027725545821551734 ) ) ;
#17376 = DIRECTION ( 'NONE',  ( -1.000000000000000000, 0.000000000000000000, 0.000000000000000000 ) ) ;
#17377 = FACE_OUTER_BOUND ( 'NONE', #14730, .T. ) ;
#17378 = EDGE_CURVE ( 'NONE', #33824, #3203, #34486, .T. ) ;
#17379 = VERTEX_POINT ( 'NONE', #21033 ) ;
#17380 = CIRCLE ( 'NONE', #28917, 17.49900000000001654 ) ;
#17381 = ORIENTED_EDGE ( 'NONE', *, *, #16574, .T. ) ;
#17382 = LINE ( 'NONE', #3726, #1567 ) ;
#17383 = DIRECTION ( 'NONE',  ( -1.000000000000000000, 0.000000000000000000, 0.000000000000000000 ) ) ;
#17384 = VERTEX_POINT ( 'NONE', #27352 ) ;
#17385 = CARTESIAN_POINT ( 'NONE',  ( -33.97545270896702618, -112.8166217158120475, 8.909774454178450043 ) ) ;
#17386 = ORIENTED_EDGE ( 'NONE', *, *, #26139, .T. ) ;
#17387 = AXIS2_PLACEMENT_3D ( 'NONE', #30508, #30850, #22379 ) ;
#17388 = DIRECTION ( 'NONE',  ( -1.000000000000000000, 0.000000000000000000, 0.000000000000000000 ) ) ;
#17389 = CARTESIAN_POINT ( 'NONE',  ( 0.000000000000000000, 8.725776631572770725, -3.753907720748954180 ) ) ;
#17390 = APPLICATION_PROTOCOL_DEFINITION ( 'draft international standard', 'automotive_design', 1998, #2522 ) ;
#17391 = ADVANCED_FACE ( 'NONE', ( #23756 ), #29693, .T. ) ;
#17392 = LINE ( 'NONE', #12549, #9293 ) ;
#17393 = ORIENTED_EDGE ( 'NONE', *, *, #8952, .T. ) ;
#17394 = ORIENTED_EDGE ( 'NONE', *, *, #30836, .F. ) ;
#17395 = FACE_OUTER_BOUND ( 'NONE', #13313, .T. ) ;
#17396 = PRODUCT_RELATED_PRODUCT_CATEGORY ( 'part', '', ( #34248 ) ) ;
#17397 = CARTESIAN_POINT ( 'NONE',  ( -9.999999999999994671, 0.000000000000000000, 0.000000000000000000 ) ) ;
#17398 = ORIENTED_EDGE ( 'NONE', *, *, #14093, .T. ) ;
#17399 = CARTESIAN_POINT ( 'NONE',  ( -39.49999999999999289, -5.633167542791597704, 121.0048025873810218 ) ) ;
#17400 = CIRCLE ( 'NONE', #32384, 13.00000000000000000 ) ;
#17401 = CARTESIAN_POINT ( 'NONE',  ( -34.50000000000000000, -113.0106174888879877, 1.881901162060937827 ) ) ;
#17402 = LINE ( 'NONE', #9138, #5274 ) ;
#17403 = DIRECTION ( 'NONE',  ( 0.000000000000000000, 0.000000000000000000, -1.000000000000000000 ) ) ;
#17404 = AXIS2_PLACEMENT_3D ( 'NONE', #15544, #26563, #12155 ) ;
#17405 = CARTESIAN_POINT ( 'NONE',  ( -34.50000000000000000, -115.6492853190479337, 9.359470924297957239 ) ) ;
#17406 = ADVANCED_FACE ( 'NONE', ( #21564 ), #26649, .F. ) ;
#17407 = CARTESIAN_POINT ( 'NONE',  ( 7.999999999999992895, -46.19362259308839214, 8.585149169758333088 ) ) ;
#17408 = DIRECTION ( 'NONE',  ( 0.000000000000000000, 0.000000000000000000, -1.000000000000000000 ) ) ;
#17409 = EDGE_CURVE ( 'NONE', #19596, #29784, #29326, .T. ) ;
#17410 = CARTESIAN_POINT ( 'NONE',  ( -39.00000000000000711, -114.9929510916434339, 12.26648026267477043 ) ) ;
#17411 = CARTESIAN_POINT ( 'NONE',  ( -39.49999999999999289, 0.4463568765849662556, 113.0433323525902125 ) ) ;
#17412 = DIRECTION ( 'NONE',  ( 1.000000000000000000, 0.000000000000000000, 0.000000000000000000 ) ) ;
#17413 = CARTESIAN_POINT ( 'NONE',  ( 8.000000000000000000, -19.83898331853678343, -9.508666619816857235 ) ) ;
#17414 = DIRECTION ( 'NONE',  ( -1.000000000000000000, 0.000000000000000000, 0.000000000000000000 ) ) ;
#17415 = VECTOR ( 'NONE', #9598, 1000.000000000000000 ) ;
#17416 = ORIENTED_EDGE ( 'NONE', *, *, #11458, .F. ) ;
#17417 = VECTOR ( 'NONE', #5869, 1000.000000000000000 ) ;
#17418 = DIRECTION ( 'NONE',  ( 1.541976423090495140E-16, -1.000000000000000000, 0.000000000000000000 ) ) ;
#17419 = VERTEX_POINT ( 'NONE', #13489 ) ;
#17420 = AXIS2_PLACEMENT_3D ( 'NONE', #8892, #19340, #24769 ) ;
#17421 = CARTESIAN_POINT ( 'NONE',  ( -34.92058450342249643, -111.8367748094582197, 3.808975545821551734 ) ) ;
#17422 = CARTESIAN_POINT ( 'NONE',  ( 7.999999999999992895, -43.55304910509426719, 28.41006711799970574 ) ) ;
#17423 = CARTESIAN_POINT ( 'NONE',  ( -35.50000000000000711, -115.9821387493194891, -0.8839717462762166633 ) ) ;
#17424 = EDGE_CURVE ( 'NONE', #25748, #2812, #32039, .T. ) ;
#17425 = VERTEX_POINT ( 'NONE', #35458 ) ;
#17426 = ORIENTED_EDGE ( 'NONE', *, *, #31720, .F. ) ;
#17427 = DIRECTION ( 'NONE',  ( 1.000000000000000000, 0.000000000000000000, -1.691777834109591283E-31 ) ) ;
#17428 = CARTESIAN_POINT ( 'NONE',  ( 7.999999999999992895, -32.32520163883559405, -34.09746168776067776 ) ) ;
#17429 = ORIENTED_EDGE ( 'NONE', *, *, #33586, .T. ) ;
#17430 = VERTEX_POINT ( 'NONE', #7713 ) ;
#17431 = AXIS2_PLACEMENT_3D ( 'NONE', #10604, #21560, #32558 ) ;
#17432 = CARTESIAN_POINT ( 'NONE',  ( 7.999999999999992895, 41.20225022064637699, 23.63323037071417332 ) ) ;
#17433 = EDGE_LOOP ( 'NONE', ( #18327, #8064, #1338, #22177 ) ) ;
#17434 = VERTEX_POINT ( 'NONE', #32216 ) ;
#17435 = CARTESIAN_POINT ( 'NONE',  ( -36.94073759706868287, -115.9999999999999858, 4.371475545821550845 ) ) ;
#17436 = DIRECTION ( 'NONE',  ( 1.000000000000000000, 0.000000000000000000, 0.000000000000000000 ) ) ;
#17437 = EDGE_CURVE ( 'NONE', #3084, #5415, #23552, .T. ) ;
#17438 = DIRECTION ( 'NONE',  ( -1.000000000000000000, 0.000000000000000000, 0.000000000000000000 ) ) ;
#17439 = ORIENTED_EDGE ( 'NONE', *, *, #25848, .T. ) ;
#17440 = ORIENTED_EDGE ( 'NONE', *, *, #27606, .F. ) ;
#17441 = CARTESIAN_POINT ( 'NONE',  ( -35.50000000000000000, -111.4147656069378058, -1.853877267569947529 ) ) ;
#17442 = ADVANCED_FACE ( 'NONE', ( #23942 ), #18347, .T. ) ;
#17443 = VECTOR ( 'NONE', #23968, 1000.000000000000000 ) ;
#17444 = AXIS2_PLACEMENT_3D ( 'NONE', #25857, #1184, #11614 ) ;
#17445 = EDGE_CURVE ( 'NONE', #15308, #11089, #35288, .T. ) ;
#17446 = AXIS2_PLACEMENT_3D ( 'NONE', #28497, #1485, #31722 ) ;
#17447 = DIRECTION ( 'NONE',  ( 0.000000000000000000, 0.3681245526846787519, -0.9297764858882511252 ) ) ;
#17448 = ORIENTED_EDGE ( 'NONE', *, *, #30690, .F. ) ;
#17449 = CARTESIAN_POINT ( 'NONE',  ( 0.000000000000000000, 0.000000000000000000, 60.00000000000000000 ) ) ;
#17450 = CARTESIAN_POINT ( 'NONE',  ( -39.00000000000000000, -113.9929510916434339, 12.56351784598954779 ) ) ;
#17451 = LINE ( 'NONE', #5786, #26917 ) ;
#17452 = EDGE_CURVE ( 'NONE', #27872, #7481, #7377, .T. ) ;
#17453 = LINE ( 'NONE', #1092, #22582 ) ;
#17454 = ADVANCED_FACE ( 'NONE', ( #32561 ), #10067, .F. ) ;
#17455 = CARTESIAN_POINT ( 'NONE',  ( -37.49023442168701337, -113.9929510916434339, 14.11852773550420359 ) ) ;
#17456 = CARTESIAN_POINT ( 'NONE',  ( 3.799999999999999822, -2.710505431213761085E-17, -45.89999999999999858 ) ) ;
#17457 = CARTESIAN_POINT ( 'NONE',  ( -35.98364338251434447, -114.9929510916434339, 13.11827392651456314 ) ) ;
#17458 = DIRECTION ( 'NONE',  ( 0.000000000000000000, 0.000000000000000000, 1.000000000000000000 ) ) ;
#17459 = VECTOR ( 'NONE', #31469, 1000.000000000000114 ) ;
#17460 = VERTEX_POINT ( 'NONE', #24124 ) ;
#17461 = LINE ( 'NONE', #25944, #26770 ) ;
#17462 = CARTESIAN_POINT ( 'NONE',  ( 8.000000000000000000, 15.92965478239641008, -15.17386234660365751 ) ) ;
#17463 = EDGE_LOOP ( 'NONE', ( #10014, #23981, #23104, #101 ) ) ;
#17464 = CARTESIAN_POINT ( 'NONE',  ( -35.93473953453761283, -114.9929510916434339, 13.11451721564123574 ) ) ;
#17465 = ORIENTED_EDGE ( 'NONE', *, *, #2482, .T. ) ;
#17466 = DIRECTION ( 'NONE',  ( 1.000000000000000000, 1.734723475976807094E-16, 0.000000000000000000 ) ) ;
#17467 = VERTEX_POINT ( 'NONE', #13149 ) ;
#17468 = DIRECTION ( 'NONE',  ( -1.000000000000000000, 0.000000000000000000, 0.000000000000000000 ) ) ;
#17469 = VERTEX_POINT ( 'NONE', #2519 ) ;
#17470 = CIRCLE ( 'NONE', #30720, 3.799999999999999822 ) ;
#17471 = VECTOR ( 'NONE', #18894, 1000.000000000000000 ) ;
#17472 = CARTESIAN_POINT ( 'NONE',  ( -35.50000000000000000, -115.0140978167138712, -0.6247823525984403936 ) ) ;
#17473 = CARTESIAN_POINT ( 'NONE',  ( 0.000000000000000000, 0.000000000000000000, 0.000000000000000000 ) ) ;
#17474 = CARTESIAN_POINT ( 'NONE',  ( -38.45611840935523418, -115.3723087153909432, 5.066024454178449155 ) ) ;
#17475 = ORIENTED_EDGE ( 'NONE', *, *, #24717, .F. ) ;
#17476 = CARTESIAN_POINT ( 'NONE',  ( -39.02454729103295961, -114.7691647218148745, 3.659774454178448710 ) ) ;
#17477 = DIRECTION ( 'NONE',  ( -1.000000000000000000, 0.000000000000000000, 0.000000000000000000 ) ) ;
#17478 = CARTESIAN_POINT ( 'NONE',  ( -35.50000000000000711, -112.0140978167138712, 0.6252176474015680441 ) ) ;
#17479 = ORIENTED_EDGE ( 'NONE', *, *, #1843, .F. ) ;
#17480 = VERTEX_POINT ( 'NONE', #24471 ) ;
#17481 = DIRECTION ( 'NONE',  ( 0.000000000000000000, 0.000000000000000000, 1.000000000000000000 ) ) ;
#17482 = SHAPE_REPRESENTATION_RELATIONSHIP ( 'NONE' , 'NONE' ,  #31216, #30145 ) ;
#17483 = EDGE_CURVE ( 'NONE', #20473, #32241, #10789, .T. ) ;
#17484 = DIRECTION ( 'NONE',  ( -1.783119874454246424E-31, -1.187911941725854497E-31, 1.000000000000000000 ) ) ;
#17486 = EDGE_LOOP ( 'NONE', ( #14177, #24005, #19107, #22794 ) ) ;
#17485 = AXIS2_PLACEMENT_3D ( 'NONE', #24747, #33541, #30674 ) ;
#17487 = VERTEX_POINT ( 'NONE', #30053 ) ;
#17488 = CARTESIAN_POINT ( 'NONE',  ( -34.50000000000000000, -115.2732872103912030, -1.592823285204062911 ) ) ;
#17489 = DIRECTION ( 'NONE',  ( 5.339440136655842133E-16, 1.000000000000000000, -1.918536189538073087E-16 ) ) ;
#17490 = ADVANCED_FACE ( 'NONE', ( #16336 ), #2700, .T. ) ;
#17491 = ORIENTED_EDGE ( 'NONE', *, *, #12316, .F. ) ;
#17492 = ORIENTED_EDGE ( 'NONE', *, *, #4523, .T. ) ;
#17493 = CARTESIAN_POINT ( 'NONE',  ( 0.000000000000000000, -18.62763138773852134, 2.494040418455287345 ) ) ;
#17494 = CARTESIAN_POINT ( 'NONE',  ( -37.43749999999998579, -113.9929510916434339, 13.11852480586264846 ) ) ;
#17495 = CIRCLE ( 'NONE', #4885, 4.000000000000000000 ) ;
#17496 = DIRECTION ( 'NONE',  ( 0.000000000000000000, 0.000000000000000000, 1.000000000000000000 ) ) ;
#17497 = CARTESIAN_POINT ( 'NONE',  ( -1.000000000000000888, -6.008326913195953800, 0.000000000000000000 ) ) ;
#17498 = CARTESIAN_POINT ( 'NONE',  ( -36.15625000000007816, -113.9929510916434339, 13.11852480586264846 ) ) ;
#17499 = TOROIDAL_SURFACE ( 'NONE', #270, 4.200000000000000178, 0.1999999999999998723 ) ;
#17500 = CARTESIAN_POINT ( 'NONE',  ( -35.50000000000000000, -115.9920935318519923, 10.44577481630138749 ) ) ;
#17501 = DIRECTION ( 'NONE',  ( 0.000000000000000000, 0.000000000000000000, 1.000000000000000000 ) ) ;
#17502 = CARTESIAN_POINT ( 'NONE',  ( 0.000000000000000000, -36.34385289850568057, -29.77717097092114074 ) ) ;
#17503 = ORIENTED_EDGE ( 'NONE', *, *, #21565, .F. ) ;
#17504 = CARTESIAN_POINT ( 'NONE',  ( 4.000000000000000000, 4.898587196589412829E-16, -40.89999999999999858 ) ) ;
#17505 = DIRECTION ( 'NONE',  ( 1.000000000000000000, 1.734723475976807094E-16, 0.000000000000000000 ) ) ;
#17506 = CARTESIAN_POINT ( 'NONE',  ( -3.799999999999999822, 4.382607293638566128E-16, -30.90000000000000568 ) ) ;
#17507 = VECTOR ( 'NONE', #20018, 1000.000000000000114 ) ;
#17508 = ORIENTED_EDGE ( 'NONE', *, *, #6007, .F. ) ;
#17509 = CARTESIAN_POINT ( 'NONE',  ( 8.000000000000007105, -0.3151488735046864553, -11.27190672109269798 ) ) ;
#17510 = CARTESIAN_POINT ( 'NONE',  ( 0.000000000000000000, -32.00046193115173310, 34.40241257139674502 ) ) ;
#17511 = CARTESIAN_POINT ( 'NONE',  ( 7.999999999999992895, 0.000000000000000000, 0.000000000000000000 ) ) ;
#17512 = LINE ( 'NONE', #4044, #1772 ) ;
#17513 = DIRECTION ( 'NONE',  ( 0.000000000000000000, 0.000000000000000000, -1.000000000000000000 ) ) ;
#17514 = CARTESIAN_POINT ( 'NONE',  ( 0.000000000000000000, 0.000000000000000000, 65.00000000000000000 ) ) ;
#17515 = ORIENTED_EDGE ( 'NONE', *, *, #18033, .T. ) ;
#17516 = CARTESIAN_POINT ( 'NONE',  ( 4.000000000000003553, -13.42368113696669418, 3.975523202427999614 ) ) ;
#17517 = CIRCLE ( 'NONE', #33043, 15.49899999999999878 ) ;
#17518 = CARTESIAN_POINT ( 'NONE',  ( -34.50000000000000000, -117.0140978167138854, -0.4997823525984417259 ) ) ;
#17519 = CARTESIAN_POINT ( 'NONE',  ( -46.00000000000000000, -25.98076211353320275, 84.99999999999992895 ) ) ;
#17520 = ORIENTED_EDGE ( 'NONE', *, *, #5964, .T. ) ;
#17521 = VERTEX_POINT ( 'NONE', #21397 ) ;
#17522 = CARTESIAN_POINT ( 'NONE',  ( -37.99999999999998579, -113.9407375970686758, 2.253524454178448710 ) ) ;
#17523 = EDGE_LOOP ( 'NONE', ( #30466, #8701, #21068, #10630 ) ) ;
#17524 = AXIS2_PLACEMENT_3D ( 'NONE', #10043, #2150, #29669 ) ;
#17525 = ORIENTED_EDGE ( 'NONE', *, *, #3980, .T. ) ;
#17526 = ORIENTED_EDGE ( 'NONE', *, *, #26013, .F. ) ;
#17527 = CARTESIAN_POINT ( 'NONE',  ( -35.50000000000000000, -114.5974311500472567, -0.6247823525984269599 ) ) ;
#17528 = EDGE_CURVE ( 'NONE', #13301, #26725, #33910, .T. ) ;
#17529 = CARTESIAN_POINT ( 'NONE',  ( -35.50000000000000711, -114.8474311500471572, -1.624782352598427959 ) ) ;
#17530 = DIRECTION ( 'NONE',  ( 0.000000000000000000, -0.1253332335642905471, -0.9921147013144795412 ) ) ;
#17531 = CARTESIAN_POINT ( 'NONE',  ( -36.06250000000002132, -114.9929510916434339, 13.11852480586264669 ) ) ;
#17532 = DIRECTION ( 'NONE',  ( -1.000000000000000000, -0.000000000000000000, -0.000000000000000000 ) ) ;
#17533 = EDGE_CURVE ( 'NONE', #17024, #8057, #5748, .T. ) ;
#17534 = DIRECTION ( 'NONE',  ( -1.000000000000000000, 0.000000000000000000, 0.000000000000000000 ) ) ;
#17535 = CARTESIAN_POINT ( 'NONE',  ( -34.50000000000000000, -114.9492820284331742, 10.20776876943783940 ) ) ;
#17536 = LINE ( 'NONE', #284, #3045 ) ;
#17537 = PRODUCT ( 'instrument roller bearing_iso_ISO 1224 - 180816 - R,14,SI,NC,14', 'instrument roller bearing_iso_ISO 1224 - 180816 - R,14,SI,NC,14', '', ( #25346 ) ) ;
#17538 = AXIS2_PLACEMENT_3D ( 'NONE', #4831, #23725, #15773 ) ;
#17539 = LINE ( 'NONE', #28194, #28383 ) ;
#17540 = ORIENTED_EDGE ( 'NONE', *, *, #21841, .T. ) ;
#17541 = CARTESIAN_POINT ( 'NONE',  ( -35.50000000000000000, -114.2450133963102843, 8.522190569412378736 ) ) ;
#17542 = CARTESIAN_POINT ( 'NONE',  ( -35.50000000000000711, -112.7765286249690035, 1.847058736912741583 ) ) ;
#17543 = DIRECTION ( 'NONE',  ( -1.047965281155519913E-16, -6.938893903907192632E-17, -1.000000000000000000 ) ) ;
#17544 = DIRECTION ( 'NONE',  ( 1.000000000000000000, -4.528031003192420052E-15, -1.179290629824070178E-15 ) ) ;
#17545 = VECTOR ( 'NONE', #18092, 1000.000000000000000 ) ;
#17546 = CARTESIAN_POINT ( 'NONE',  ( -34.49999999999998579, -21.98076211353320630, 83.49999999999994316 ) ) ;
#17547 = LINE ( 'NONE', #641, #10720 ) ;
#17548 = CARTESIAN_POINT ( 'NONE',  ( 5.400000000000085620, -1.000000000000049516, -44.50000000000000000 ) ) ;
#17549 = CARTESIAN_POINT ( 'NONE',  ( 8.000000000000007105, -11.27190672109260028, -0.3151488735048807444 ) ) ;
#17550 = CARTESIAN_POINT ( 'NONE',  ( 8.000000000000007105, 0.000000000000000000, 0.000000000000000000 ) ) ;
#17551 = VERTEX_POINT ( 'NONE', #27873 ) ;
#17552 = CARTESIAN_POINT ( 'NONE',  ( -36.25098837183130485, -114.6652019342044184, 5.683975545821551734 ) ) ;
#17553 = DIRECTION ( 'NONE',  ( 0.000000000000000000, 0.000000000000000000, -1.000000000000000000 ) ) ;
#17554 = CARTESIAN_POINT ( 'NONE',  ( 0.000000000000000000, 0.000000000000000000, -1.000000000000000222 ) ) ;
#17555 = ORIENTED_EDGE ( 'NONE', *, *, #5363, .F. ) ;
#17556 = CIRCLE ( 'NONE', #11808, 52.00000000000000711 ) ;
#17557 = VERTEX_POINT ( 'NONE', #28061 ) ;
#17558 = CARTESIAN_POINT ( 'NONE',  ( -4.000000000000000000, -2.710505431213761085E-17, -45.89999999999999858 ) ) ;
#17559 = ORIENTED_EDGE ( 'NONE', *, *, #26139, .F. ) ;
#17560 = CARTESIAN_POINT ( 'NONE',  ( -36.94073759706868287, -116.9999999999999858, 5.871475545821551734 ) ) ;
#17561 = ORIENTED_EDGE ( 'NONE', *, *, #20534, .F. ) ;
#17562 = DIRECTION ( 'NONE',  ( -1.000000000000000000, 0.000000000000000000, 0.000000000000000000 ) ) ;
#17563 = EDGE_CURVE ( 'NONE', #10728, #24139, #6082, .T. ) ;
#17564 = CARTESIAN_POINT ( 'NONE',  ( 1.799999999999995159, 1.496458227839707357E-15, 7.800000000000051337 ) ) ;
#17565 = CIRCLE ( 'NONE', #25640, 20.00000000000000355 ) ;
#17566 = EDGE_CURVE ( 'NONE', #2467, #6941, #28156, .T. ) ;
#17567 = CARTESIAN_POINT ( 'NONE',  ( 5.400000000000003020, 1.000000000000000888, 38.00000000000000000 ) ) ;
#17568 = APPLICATION_PROTOCOL_DEFINITION ( 'draft international standard', 'automotive_design', 1998, #7123 ) ;
#17569 = VECTOR ( 'NONE', #33120, 1000.000000000000000 ) ;
#17570 = DIRECTION ( 'NONE',  ( -4.662936703425629071E-15, 1.000000000000000000, -4.222049128630314618E-16 ) ) ;
#17571 = VERTEX_POINT ( 'NONE', #147 ) ;
#17572 = ORIENTED_EDGE ( 'NONE', *, *, #27527, .T. ) ;
#17573 = CIRCLE ( 'NONE', #25076, 19.99999999999998579 ) ;
#17574 = DIRECTION ( 'NONE',  ( -1.000000000000000000, 0.000000000000000000, 0.000000000000000000 ) ) ;
#17575 = CARTESIAN_POINT ( 'NONE',  ( -44.00199999999999534, -1.144142364505046046E-15, 3.000000000000002665 ) ) ;
#17576 = ADVANCED_FACE ( 'NONE', ( #14349 ), #30410, .T. ) ;
#17577 = ORIENTED_EDGE ( 'NONE', *, *, #33010, .F. ) ;
#17578 = DIRECTION ( 'NONE',  ( -1.000000000000000000, -1.734723475976807094E-16, -0.000000000000000000 ) ) ;
#17579 = ADVANCED_FACE ( 'NONE', ( #11483 ), #24997, .T. ) ;
#17580 = CIRCLE ( 'NONE', #6083, 17.49900000000001654 ) ;
#17581 = CARTESIAN_POINT ( 'NONE',  ( -34.50000000000000000, -115.0140978167138712, -0.6247823525984418369 ) ) ;
#17582 = FACE_OUTER_BOUND ( 'NONE', #20082, .T. ) ;
#17583 = CARTESIAN_POINT ( 'NONE',  ( -34.50000000000000000, -115.7766462221073454, 9.569741527169023598 ) ) ;
#17584 = DIRECTION ( 'NONE',  ( 0.000000000000000000, 0.000000000000000000, 1.000000000000000000 ) ) ;
#17585 = CARTESIAN_POINT ( 'NONE',  ( 0.000000000000000000, 32.00046193115148441, 34.40241257139697950 ) ) ;
#17586 = CARTESIAN_POINT ( 'NONE',  ( -39.00000000000000711, -114.9929510916434339, 12.59102132592608925 ) ) ;
#17587 = FACE_OUTER_BOUND ( 'NONE', #33933, .T. ) ;
#17588 = DIRECTION ( 'NONE',  ( 1.000000000000000000, 1.836970198721029934E-16, 0.000000000000000000 ) ) ;
#17589 = CARTESIAN_POINT ( 'NONE',  ( 9.714451465470119729E-14, 0.9999999999999870104, -40.00000000000000000 ) ) ;
#17590 = LINE ( 'NONE', #25728, #9458 ) ;
#17591 = CIRCLE ( 'NONE', #24512, 4.000000000000000000 ) ;
#17592 = DIRECTION ( 'NONE',  ( 0.000000000000000000, 0.9510565162951544194, -0.3090169943749447867 ) ) ;
#17593 = ORIENTED_EDGE ( 'NONE', *, *, #6641, .F. ) ;
#17594 = CARTESIAN_POINT ( 'NONE',  ( -35.69809690994941320, -116.9754527089670546, 4.277725545821552622 ) ) ;
#17595 = AXIS2_PLACEMENT_3D ( 'NONE', #32271, #13366, #7592 ) ;
#17596 = CYLINDRICAL_SURFACE ( 'NONE', #31903, 4.800000000000000711 ) ;
#17597 = ADVANCED_FACE ( 'NONE', ( #8597 ), #8766, .F. ) ;
#17598 = CARTESIAN_POINT ( 'NONE',  ( -35.50000000000000000, -113.0140978167138712, -0.3122823525984338988 ) ) ;
#17599 = ORIENTED_EDGE ( 'NONE', *, *, #23519, .F. ) ;
#17600 = EDGE_LOOP ( 'NONE', ( #4566, #26003, #2829, #6485 ) ) ;
#17601 = AXIS2_PLACEMENT_3D ( 'NONE', #8707, #19676, #27474 ) ;
#17602 = DIRECTION ( 'NONE',  ( -1.000000000000000000, 0.000000000000000000, 0.000000000000000000 ) ) ;
#17603 = CARTESIAN_POINT ( 'NONE',  ( 8.000000000000007105, 0.3151488735050472778, -11.27190672109269087 ) ) ;
#17604 = ORIENTED_EDGE ( 'NONE', *, *, #31775, .T. ) ;
#17605 = CIRCLE ( 'NONE', #34918, 9.499000000000004107 ) ;
#17606 = ORIENTED_EDGE ( 'NONE', *, *, #23202, .F. ) ;
#17607 = VECTOR ( 'NONE', #24190, 1000.000000000000000 ) ;
#17608 = AXIS2_PLACEMENT_3D ( 'NONE', #16304, #21528, #119 ) ;
#17609 = EDGE_CURVE ( 'NONE', #33387, #18497, #22282, .T. ) ;
#17610 = DIRECTION ( 'NONE',  ( -1.000000000000000000, -0.000000000000000000, -0.000000000000000000 ) ) ;
#17611 = ORIENTED_EDGE ( 'NONE', *, *, #8995, .F. ) ;
#17612 = EDGE_CURVE ( 'NONE', #8697, #13527, #545, .T. ) ;
#17613 = CARTESIAN_POINT ( 'NONE',  ( -35.00000000000000000, -113.9407375970687895, 2.496475545821554398 ) ) ;
#17614 = EDGE_CURVE ( 'NONE', #23698, #2158, #16696, .T. ) ;
#17615 = DIRECTION ( 'NONE',  ( 1.000000000000000000, 0.000000000000000000, 0.000000000000000000 ) ) ;
#17616 = CYLINDRICAL_SURFACE ( 'NONE', #24801, 19.99999999999998579 ) ;
#17617 = AXIS2_PLACEMENT_3D ( 'NONE', #7904, #19061, #27189 ) ;
#17618 = VERTEX_POINT ( 'NONE', #11650 ) ;
#17619 = ORIENTED_EDGE ( 'NONE', *, *, #232, .F. ) ;
#17620 = CARTESIAN_POINT ( 'NONE',  ( -35.50000000000000000, -112.7530559548648341, -2.608751991713152307 ) ) ;
#17621 = ADVANCED_BREP_SHAPE_REPRESENTATION ( '', ( #34526, #21307 ), #24207 ) ;
#17622 = VECTOR ( 'NONE', #31694, 1000.000000000000000 ) ;
#17623 = ADVANCED_FACE ( 'NONE', ( #33280 ), #30574, .T. ) ;
#17624 = CYLINDRICAL_SURFACE ( 'NONE', #24699, 20.00000000000000355 ) ;
#17625 = ORIENTED_EDGE ( 'NONE', *, *, #9449, .F. ) ;
#17626 = CARTESIAN_POINT ( 'NONE',  ( -37.93687354226506869, -114.9929510916434339, 12.87038173996323565 ) ) ;
#17627 = CIRCLE ( 'NONE', #2149, 4.800000000000006040 ) ;
#17628 = CIRCLE ( 'NONE', #2151, 4.800000000000006040 ) ;
#17629 = EDGE_CURVE ( 'NONE', #27414, #19486, #22381, .T. ) ;
#17630 = VECTOR ( 'NONE', #9961, 1000.000000000000000 ) ;
#17631 = CARTESIAN_POINT ( 'NONE',  ( -34.50000000000000000, -114.0998638248492085, 9.511920366020609308 ) ) ;
#17632 = CIRCLE ( 'NONE', #11332, 4.800000000000000711 ) ;
#17633 = FACE_OUTER_BOUND ( 'NONE', #35581, .T. ) ;
#17634 = DIRECTION ( 'NONE',  ( 0.000000000000000000, 0.9672551082808337197, -0.2538061376417689030 ) ) ;
#17635 = CARTESIAN_POINT ( 'NONE',  ( -37.59808119975203766, -113.9929510916434339, 14.11551573851449071 ) ) ;
#17636 = DIRECTION ( 'NONE',  ( 1.000000000000000000, 0.000000000000000000, 0.000000000000000000 ) ) ;
#17637 = CIRCLE ( 'NONE', #11919, 47.49900000000000944 ) ;
#17638 = CARTESIAN_POINT ( 'NONE',  ( -35.50005019975638021, -114.9929510916434339, 12.62670525340498529 ) ) ;
#17639 = FACE_OUTER_BOUND ( 'NONE', #30503, .T. ) ;
#17640 = ORIENTED_EDGE ( 'NONE', *, *, #32146, .F. ) ;
#17641 = CARTESIAN_POINT ( 'NONE',  ( 65.00000000000001421, -25.98076211353320986, 84.99999999999994316 ) ) ;
#17642 = CARTESIAN_POINT ( 'NONE',  ( 70.00000000000001421, -27.28312344603513040, 77.61394185240837373 ) ) ;
#17643 = VERTEX_POINT ( 'NONE', #2875 ) ;
#17644 = CARTESIAN_POINT ( 'NONE',  ( -35.50000000000000711, -114.9929510916434339, 12.17846912687782712 ) ) ;
#17645 = VERTEX_POINT ( 'NONE', #17809 ) ;
#17646 = CARTESIAN_POINT ( 'NONE',  ( 4.000000000000003553, 51.19683565102445044, 9.104066087303658961 ) ) ;
#17647 = EDGE_CURVE ( 'NONE', #32025, #2204, #9177, .T. ) ;
#17648 = VECTOR ( 'NONE', #2977, 1000.000000000000000 ) ;
#17649 = ORIENTED_EDGE ( 'NONE', *, *, #13509, .T. ) ;
#17650 = DIRECTION ( 'NONE',  ( -0.000000000000000000, 0.000000000000000000, -1.000000000000000000 ) ) ;
#17651 = VERTEX_POINT ( 'NONE', #22454 ) ;
#17652 = CIRCLE ( 'NONE', #1556, 14.00000000000000000 ) ;
#17653 = CARTESIAN_POINT ( 'NONE',  ( -35.50000000000000000, -113.0140978167138712, -0.6247823525983134951 ) ) ;
#17654 = CARTESIAN_POINT ( 'NONE',  ( -10.50000000000000178, 1.285879139104719253E-15, -1.200000000000006617 ) ) ;
#17655 = EDGE_CURVE ( 'NONE', #26672, #34739, #13793, .T. ) ;
#17656 = CARTESIAN_POINT ( 'NONE',  ( -35.54388159064475872, -112.6276912846090568, 7.316024454178449155 ) ) ;
#17657 = EDGE_CURVE ( 'NONE', #2418, #7438, #6873, .T. ) ;
#17658 = EDGE_LOOP ( 'NONE', ( #14968, #9028, #35352, #18904 ) ) ;
#17659 = CARTESIAN_POINT ( 'NONE',  ( -35.02454729103298803, -114.8876895276775087, 4.597274454178448266 ) ) ;
#17660 = AXIS2_PLACEMENT_3D ( 'NONE', #25894, #23532, #4115 ) ;
#17661 = CIRCLE ( 'NONE', #31474, 14.00000000000000000 ) ;
#17662 = CIRCLE ( 'NONE', #32070, 20.00000000000001421 ) ;
#17663 = PLANE ( 'NONE',  #34338 ) ;
#17664 = CARTESIAN_POINT ( 'NONE',  ( -35.50000000000000711, -112.0269151300720409, -0.7876962586524208776 ) ) ;
#17665 = VERTEX_POINT ( 'NONE', #19222 ) ;
#17666 = ORIENTED_EDGE ( 'NONE', *, *, #3395, .F. ) ;
#17667 = CONICAL_SURFACE ( 'NONE', #29119, 4.725000000000016520, 0.5675376247847534472 ) ;
#17668 = ADVANCED_FACE ( 'NONE', ( #30225 ), #5564, .T. ) ;
#17669 = DIRECTION ( 'NONE',  ( -1.000000000000000000, -0.000000000000000000, -0.000000000000000000 ) ) ;
#17670 = ADVANCED_FACE ( 'NONE', ( #18118 ), #34525, .T. ) ;
#17671 = AXIS2_PLACEMENT_3D ( 'NONE', #13260, #8358, #18821 ) ;
#17672 = DIRECTION ( 'NONE',  ( 0.000000000000000000, 0.000000000000000000, 1.000000000000000000 ) ) ;
#17673 = VERTEX_POINT ( 'NONE', #28585 ) ;
#17674 = ORIENTED_EDGE ( 'NONE', *, *, #27958, .T. ) ;
#17675 = CARTESIAN_POINT ( 'NONE',  ( -34.50000000000000000, -113.8814751941374652, 2.992951091643117678 ) ) ;
#17676 = CARTESIAN_POINT ( 'NONE',  ( -35.50000000000000711, -113.0796441757086939, 1.890140615870383956 ) ) ;
#17677 = ORIENTED_EDGE ( 'NONE', *, *, #32309, .F. ) ;
#17678 = PRODUCT_DEFINITION_CONTEXT ( 'detailed design', #34261, 'design' ) ;
#17679 = ORIENTED_EDGE ( 'NONE', *, *, #28358, .T. ) ;
#17680 = DIRECTION ( 'NONE',  ( 8.645950338799857827E-17, -6.938893903907203726E-17, -1.000000000000000000 ) ) ;
#17681 = CIRCLE ( 'NONE', #11368, 52.00000000000000711 ) ;
#17682 = CIRCLE ( 'NONE', #15954, 8.000000000000049738 ) ;
#17683 = CARTESIAN_POINT ( 'NONE',  ( -35.60016694755736211, -113.9929510916434339, 12.92579853460621386 ) ) ;
#17684 = CARTESIAN_POINT ( 'NONE',  ( -55.00000000000000000, -25.98076211353320275, 84.99999999999994316 ) ) ;
#17685 = CARTESIAN_POINT ( 'NONE',  ( -35.50640865667917723, -113.9929510916434339, 12.69998175888958691 ) ) ;
#17686 = AXIS2_PLACEMENT_3D ( 'NONE', #34557, #12404, #14548 ) ;
#17687 = CARTESIAN_POINT ( 'NONE',  ( -35.50000000000000000, -115.9929510916434481, 12.59102132592610346 ) ) ;
#17688 = DIRECTION ( 'NONE',  ( 0.000000000000000000, 0.3681245526846720906, 0.9297764858882537897 ) ) ;
#17689 = CARTESIAN_POINT ( 'NONE',  ( -39.49999999999999289, -12.31102132296306451, 91.73752798680880005 ) ) ;
#17690 = CARTESIAN_POINT ( 'NONE',  ( 65.00000000000001421, 46.40248769959372055, 64.62118051744215563 ) ) ;
#17691 = CARTESIAN_POINT ( 'NONE',  ( -9.999999999999994671, 0.000000000000000000, 0.000000000000000000 ) ) ;
#17692 = VECTOR ( 'NONE', #27730, 1000.000000000000000 ) ;
#17693 = DIRECTION ( 'NONE',  ( -1.000000000000000000, 0.000000000000000000, 0.000000000000000000 ) ) ;
#17694 = EDGE_CURVE ( 'NONE', #26822, #209, #16054, .T. ) ;
#17695 = EDGE_LOOP ( 'NONE', ( #26125, #23707, #30198, #32484 ) ) ;
#17696 = DIRECTION ( 'NONE',  ( -1.000000000000000000, -0.000000000000000000, 0.000000000000000000 ) ) ;
#17697 = EDGE_CURVE ( 'NONE', #16103, #8762, #4019, .T. ) ;
#17698 = CARTESIAN_POINT ( 'NONE',  ( -35.50000000000000711, -112.9876085932806262, 1.879154677457530065 ) ) ;
#17699 = CARTESIAN_POINT ( 'NONE',  ( -42.49999999999999289, -25.27980021920989984, 89.21410161513770731 ) ) ;
#17700 = CARTESIAN_POINT ( 'NONE',  ( -35.50000000000000711, -114.0928965812550757, 9.511088712577292270 ) ) ;
#17701 = DIRECTION ( 'NONE',  ( -1.000000000000000000, 0.000000000000000000, 0.000000000000000000 ) ) ;
#17702 = VERTEX_POINT ( 'NONE', #6431 ) ;
#17703 = DIRECTION ( 'NONE',  ( 1.000000000000000000, -4.625929269271460079E-15, -1.156482317317865020E-15 ) ) ;
#17704 = CARTESIAN_POINT ( 'NONE',  ( -34.50000000000000000, -116.9980674558286040, -0.8858242144478970514 ) ) ;
#17705 = DIRECTION ( 'NONE',  ( 0.000000000000000000, -0.6845471059286791782, -0.7289686274214204342 ) ) ;
#17706 = VERTEX_POINT ( 'NONE', #22988 ) ;
#17707 = ORIENTED_EDGE ( 'NONE', *, *, #15213, .F. ) ;
#17708 = CARTESIAN_POINT ( 'NONE',  ( -36.52652403469559061, -114.9754527089670262, 8.777725545821549957 ) ) ;
#17709 = AXIS2_PLACEMENT_3D ( 'NONE', #18885, #7717, #29880 ) ;
#17710 = ORIENTED_EDGE ( 'NONE', *, *, #9466, .F. ) ;
#17711 = VECTOR ( 'NONE', #5352, 1000.000000000000000 ) ;
#17712 = ORIENTED_EDGE ( 'NONE', *, *, #23597, .T. ) ;
#17713 = ORIENTED_EDGE ( 'NONE', *, *, #10603, .F. ) ;
#17714 = VECTOR ( 'NONE', #28931, 1000.000000000000000 ) ;
#17715 = CARTESIAN_POINT ( 'NONE',  ( -34.50000000000000000, -113.9344536409997630, 0.9850770315317123327 ) ) ;
#17716 = CIRCLE ( 'NONE', #8521, 8.000000000000012434 ) ;
#17717 = CARTESIAN_POINT ( 'NONE',  ( 0.000000000000000000, 0.000000000000000000, 49.10000000000000142 ) ) ;
#17718 = CARTESIAN_POINT ( 'NONE',  ( -1.479000000000008086, 0.000000000000000000, 0.000000000000000000 ) ) ;
#17719 = CARTESIAN_POINT ( 'NONE',  ( -35.50000000000000711, -114.9929510916434339, 12.53051367006571581 ) ) ;
#17720 = DIRECTION ( 'NONE',  ( 1.000000000000000000, -5.339440136655842133E-16, -1.047965281155519420E-16 ) ) ;
#17721 = CARTESIAN_POINT ( 'NONE',  ( 4.000000000000003553, 7.162210897275723021, 51.50439529848832620 ) ) ;
#17722 = CARTESIAN_POINT ( 'NONE',  ( -35.51674767832921731, -114.9929510916434339, 14.04194344061634503 ) ) ;
#17723 = PLANE ( 'NONE',  #30664 ) ;
#17724 = DIRECTION ( 'NONE',  ( -1.000000000000000000, 0.000000000000000000, -0.000000000000000000 ) ) ;
#17725 = ORIENTED_EDGE ( 'NONE', *, *, #33446, .F. ) ;
#17726 = CIRCLE ( 'NONE', #29839, 4.000000000000000000 ) ;
#17727 = CARTESIAN_POINT ( 'NONE',  ( -35.50000000000000000, -115.9929510916434481, 10.94631322572069365 ) ) ;
#17728 = CARTESIAN_POINT ( 'NONE',  ( -35.50000000000000711, -112.0140978167138712, -0.4997823525984337878 ) ) ;
#17729 = CYLINDRICAL_SURFACE ( 'NONE', #2436, 20.00000000000000355 ) ;
#17730 = DIRECTION ( 'NONE',  ( -1.000000000000000000, 0.000000000000000000, 0.000000000000000000 ) ) ;
#17731 = CARTESIAN_POINT ( 'NONE',  ( 7.999999999999992895, -20.99948489194393275, -42.60488980472803888 ) ) ;
#17732 = AXIS2_PLACEMENT_3D ( 'NONE', #9268, #14840, #1171 ) ;
#17733 = CARTESIAN_POINT ( 'NONE',  ( -2.000000000000001776, 0.000000000000000000, 0.000000000000000000 ) ) ;
#17734 = CARTESIAN_POINT ( 'NONE',  ( -42.49999999999999289, -42.98076211353323828, 83.49999999999991473 ) ) ;
#17735 = EDGE_CURVE ( 'NONE', #33969, #26363, #14922, .T. ) ;
#17736 = DIRECTION ( 'NONE',  ( -1.000000000000000000, -0.000000000000000000, -0.000000000000000000 ) ) ;
#17737 = DIRECTION ( 'NONE',  ( 0.000000000000000000, 0.000000000000000000, -1.000000000000000000 ) ) ;
#17738 = ORIENTED_EDGE ( 'NONE', *, *, #34342, .T. ) ;
#17739 = CARTESIAN_POINT ( 'NONE',  ( -35.97545270896705460, -114.3549511594417680, 7.090225545821551734 ) ) ;
#17740 = DIRECTION ( 'NONE',  ( -1.000000000000000000, -0.000000000000000000, 0.000000000000000000 ) ) ;
#17741 = CARTESIAN_POINT ( 'NONE',  ( 0.000000000000000000, 13.55483219355729396, 11.06713717293245658 ) ) ;
#17742 = ORIENTED_EDGE ( 'NONE', *, *, #544, .T. ) ;
#17743 = ORIENTED_EDGE ( 'NONE', *, *, #25314, .T. ) ;
#17744 = CARTESIAN_POINT ( 'NONE',  ( -2.000000000000001332, 1.037758488706469473E-15, 4.724999999999999645 ) ) ;
#17745 = DIRECTION ( 'NONE',  ( 0.000000000000000000, 0.000000000000000000, 1.000000000000000000 ) ) ;
#17746 = ORIENTED_EDGE ( 'NONE', *, *, #10861, .T. ) ;
#17747 = CARTESIAN_POINT ( 'NONE',  ( -33.97545270896703329, -115.1833782841879810, 8.590225545821549957 ) ) ;
#17748 = EDGE_CURVE ( 'NONE', #19124, #27521, #17761, .T. ) ;
#17749 = VERTEX_POINT ( 'NONE', #14700 ) ;
#17750 =( LENGTH_UNIT ( ) NAMED_UNIT ( * ) SI_UNIT ( .MILLI., .METRE. ) );
#17751 = FACE_OUTER_BOUND ( 'NONE', #28175, .T. ) ;
#17752 = DIRECTION ( 'NONE',  ( 0.000000000000000000, 0.000000000000000000, 1.000000000000000000 ) ) ;
#17753 = APPLICATION_PROTOCOL_DEFINITION ( 'draft international standard', 'automotive_design', 1998, #7346 ) ;
#17754 = LINE ( 'NONE', #15048, #12745 ) ;
#17755 = ORIENTED_EDGE ( 'NONE', *, *, #29324, .F. ) ;
#17756 = VERTEX_POINT ( 'NONE', #14883 ) ;
#17757 = AXIS2_PLACEMENT_3D ( 'NONE', #17137, #25265, #31014 ) ;
#17758 = CARTESIAN_POINT ( 'NONE',  ( 70.00001200000001234, -29.47590766695025621, 82.98552407851634882 ) ) ;
#17759 = DIRECTION ( 'NONE',  ( 0.000000000000000000, 0.000000000000000000, 1.000000000000000000 ) ) ;
#17760 = ORIENTED_EDGE ( 'NONE', *, *, #11048, .T. ) ;
#17761 = LINE ( 'NONE', #23172, #30324 ) ;
#17762 = CARTESIAN_POINT ( 'NONE',  ( -34.50000000000000000, -113.0140978167138712, -0.6247823525983134951 ) ) ;
#17763 = DIRECTION ( 'NONE',  ( -1.000000000000000000, 0.000000000000000000, 0.000000000000000000 ) ) ;
#17764 = DIRECTION ( 'NONE',  ( 0.000000000000000000, 0.000000000000000000, 1.000000000000000000 ) ) ;
#17765 = CARTESIAN_POINT ( 'NONE',  ( -36.62499999999902656, -115.9929510916434481, 14.11852480586265024 ) ) ;
#17766 = DIRECTION ( 'NONE',  ( 1.084202172485500613E-16, -6.938893903907203726E-17, -1.000000000000000000 ) ) ;
#17767 = FACE_BOUND ( 'NONE', #12463, .T. ) ;
#17768 = CARTESIAN_POINT ( 'NONE',  ( -38.81062062679291103, -114.9929510916434339, 13.37409560816442067 ) ) ;
#17769 = CARTESIAN_POINT ( 'NONE',  ( -4.000000000000000000, -2.710505431213761085E-17, -21.89999999999999858 ) ) ;
#17770 = CARTESIAN_POINT ( 'NONE',  ( 0.000000000000000000, -2.710505431213761085E-17, -30.90000000000000568 ) ) ;
#17771 = CYLINDRICAL_SURFACE ( 'NONE', #2105, 20.00000000000000355 ) ;
#17772 = CARTESIAN_POINT ( 'NONE',  ( 8.000000000000000000, -18.62763138773852134, 10.49404041845529001 ) ) ;
#17773 = ADVANCED_FACE ( 'NONE', ( #20449 ), #31462, .T. ) ;
#17774 = EDGE_CURVE ( 'NONE', #17469, #9296, #24009, .T. ) ;
#17775 = CARTESIAN_POINT ( 'NONE',  ( -29.99999999999999289, 2.571758278209443239E-15, 0.000000000000000000 ) ) ;
#17776 = ORIENTED_EDGE ( 'NONE', *, *, #25973, .F. ) ;
#17777 = CARTESIAN_POINT ( 'NONE',  ( -39.16322519054178741, -111.9205845034225177, 6.433975545821551734 ) ) ;
#17778 = DIRECTION ( 'NONE',  ( -1.000000000000000000, -0.000000000000000000, 0.000000000000000000 ) ) ;
#17779 = CARTESIAN_POINT ( 'NONE',  ( -35.50000000000000000, -113.0140978167138712, 0.8752176474015154195 ) ) ;
#17780 = ORIENTED_EDGE ( 'NONE', *, *, #7618, .F. ) ;
#17781 = AXIS2_PLACEMENT_3D ( 'NONE', #26823, #2176, #322 ) ;
#17782 = VERTEX_POINT ( 'NONE', #23347 ) ;
#17783 = DIRECTION ( 'NONE',  ( 1.000000000000000000, -0.000000000000000000, -0.000000000000000000 ) ) ;
#17784 = LINE ( 'NONE', #6458, #18064 ) ;
#17785 = VERTEX_POINT ( 'NONE', #9842 ) ;
#17786 = EDGE_CURVE ( 'NONE', #26887, #5109, #13635, .T. ) ;
#17787 = VERTEX_POINT ( 'NONE', #1045 ) ;
#17788 = CIRCLE ( 'NONE', #2867, 4.800000000000000711 ) ;
#17789 = VECTOR ( 'NONE', #17979, 1000.000000000000000 ) ;
#17790 = ORIENTED_EDGE ( 'NONE', *, *, #20002, .T. ) ;
#17791 = CARTESIAN_POINT ( 'NONE',  ( 7.999999999999992895, -46.21320724403657465, 10.97699764141937884 ) ) ;
#17792 = CARTESIAN_POINT ( 'NONE',  ( -38.97545270896704039, -114.8876895276775087, 4.652725545821550845 ) ) ;
#17793 =( NAMED_UNIT ( * ) SI_UNIT ( $, .STERADIAN. ) SOLID_ANGLE_UNIT ( ) );
#17794 = DIRECTION ( 'NONE',  ( 1.000000000000000000, -5.339440136655842133E-16, -1.047965281155519420E-16 ) ) ;
#17795 = VERTEX_POINT ( 'NONE', #6965 ) ;
#17796 = ORIENTED_EDGE ( 'NONE', *, *, #19383, .T. ) ;
#17797 = CARTESIAN_POINT ( 'NONE',  ( -35.50000000000000000, -111.0301281775997353, -0.8858242144478579716 ) ) ;
#17798 = CARTESIAN_POINT ( 'NONE',  ( -21.15833593587365513, -21.76666049839542438, 84.29903810567665801 ) ) ;
#17799 = AXIS2_PLACEMENT_3D ( 'NONE', #23488, #28892, #1707 ) ;
#17800 = LINE ( 'NONE', #20673, #21244 ) ;
#17801 = EDGE_LOOP ( 'NONE', ( #16759, #19908, #12074, #30354 ) ) ;
#17802 = CARTESIAN_POINT ( 'NONE',  ( 7.999999999999992895, 27.43636312076375461, -38.14186064215119387 ) ) ;
#17803 = ADVANCED_FACE ( 'NONE', ( #15056, #1393 ), #12200, .F. ) ;
#17804 = VECTOR ( 'NONE', #9145, 1000.000000000000000 ) ;
#17805 = CARTESIAN_POINT ( 'NONE',  ( -34.50000000000000000, -114.1189822439768449, 9.514224058074130852 ) ) ;
#17806 = DIRECTION ( 'NONE',  ( 0.000000000000000000, 0.000000000000000000, -1.000000000000000000 ) ) ;
#17807 = DIRECTION ( 'NONE',  ( 1.000000000000000000, 0.000000000000000000, 0.000000000000000000 ) ) ;
#17808 = AXIS2_PLACEMENT_3D ( 'NONE', #12342, #3376, #9460 ) ;
#17809 = CARTESIAN_POINT ( 'NONE',  ( 0.000000000000000000, 18.53613841426857789, -48.58406706613882875 ) ) ;
#17810 = CARTESIAN_POINT ( 'NONE',  ( -37.24999999999992184, -113.9929510916434339, 14.11852480586265024 ) ) ;
#17812 = CARTESIAN_POINT ( 'NONE',  ( 50.00005079999998969, 14.30000000000000071, -3.000000000000002665 ) ) ;
#17811 = AXIS2_PLACEMENT_3D ( 'NONE', #13316, #2174, #10433 ) ;
#17813 = CARTESIAN_POINT ( 'NONE',  ( -36.87500000000098055, -114.9929510916434339, 13.11852480586264669 ) ) ;
#17814 = VERTEX_POINT ( 'NONE', #12369 ) ;
#17815 = CARTESIAN_POINT ( 'NONE',  ( 4.000000000000003553, -24.47917365149978508, 45.87777302070926311 ) ) ;
#17816 = LINE ( 'NONE', #9368, #20936 ) ;
#17817 = ADVANCED_FACE ( 'NONE', ( #9317 ), #34348, .T. ) ;
#17818 = EDGE_LOOP ( 'NONE', ( #11548, #1851, #28961, #14073 ) ) ;
#17819 = EDGE_CURVE ( 'NONE', #428, #4878, #20630, .T. ) ;
#17820 = CARTESIAN_POINT ( 'NONE',  ( -35.49999931242378892, -114.9929510916434339, 12.61439929482945566 ) ) ;
#17821 = ORIENTED_EDGE ( 'NONE', *, *, #1841, .F. ) ;
#17822 = EDGE_CURVE ( 'NONE', #16219, #12018, #31630, .T. ) ;
#17823 = CARTESIAN_POINT ( 'NONE',  ( -35.62769128460905677, -115.4561184093552413, 3.191024454178449155 ) ) ;
#17824 = ORIENTED_EDGE ( 'NONE', *, *, #26381, .T. ) ;
#17825 = CARTESIAN_POINT ( 'NONE',  ( 7.999999999999992895, 0.000000000000000000, 0.000000000000000000 ) ) ;
#17826 = ORIENTED_EDGE ( 'NONE', *, *, #31733, .T. ) ;
#17827 = CARTESIAN_POINT ( 'NONE',  ( -34.50000000000000000, -113.0140978167138712, 0.8127176474015720409 ) ) ;
#17828 = LINE ( 'NONE', #7031, #2401 ) ;
#17829 = CARTESIAN_POINT ( 'NONE',  ( -39.02454729103295961, -114.7691647218148745, 6.659774454178450043 ) ) ;
#17830 = EDGE_CURVE ( 'NONE', #35186, #11728, #994, .T. ) ;
#17831 = ORIENTED_EDGE ( 'NONE', *, *, #12730, .F. ) ;
#17832 = CARTESIAN_POINT ( 'NONE',  ( -38.97545270896704039, -113.1123104723225197, 5.347274454178449155 ) ) ;
#17833 = EDGE_CURVE ( 'NONE', #180, #23058, #11828, .T. ) ;
#17834 = TOROIDAL_SURFACE ( 'NONE', #11524, 5.015999999999992909, 0.04100000000000673939 ) ;
#17835 = DIRECTION ( 'NONE',  ( -1.000000000000000000, -0.000000000000000000, -0.000000000000000000 ) ) ;
#17836 = CARTESIAN_POINT ( 'NONE',  ( -35.50000000000000711, -112.7549084230351752, -1.592823285203595285 ) ) ;
#17837 = ORIENTED_EDGE ( 'NONE', *, *, #17694, .F. ) ;
#17838 = VERTEX_POINT ( 'NONE', #31105 ) ;
#17839 = LINE ( 'NONE', #28838, #14783 ) ;
#17840 = AXIS2_PLACEMENT_3D ( 'NONE', #19846, #6195, #33734 ) ;
#17841 = AXIS2_PLACEMENT_3D ( 'NONE', #176, #27384, #8458 ) ;
#17842 =( LENGTH_UNIT ( ) NAMED_UNIT ( * ) SI_UNIT ( .MILLI., .METRE. ) );
#17843 = DIRECTION ( 'NONE',  ( 0.000000000000000000, 0.1253332335643045359, -0.9921147013144778759 ) ) ;
#17844 = VERTEX_POINT ( 'NONE', #17399 ) ;
#17845 = VERTEX_POINT ( 'NONE', #28403 ) ;
#17846 = CARTESIAN_POINT ( 'NONE',  ( -34.50000000000000000, -112.5103839485166333, -1.498529437127682495 ) ) ;
#17847 = DIRECTION ( 'NONE',  ( -1.000000000000000000, -1.734723475976807094E-16, -0.000000000000000000 ) ) ;
#17848 = PRODUCT ( 'Mounting Base Plate Frame', 'Mounting Base Plate Frame', '', ( #33801 ) ) ;
#17849 = ORIENTED_EDGE ( 'NONE', *, *, #9962, .T. ) ;
#17850 = EDGE_LOOP ( 'NONE', ( #1786, #20956, #357, #14693 ) ) ;
#17851 = CARTESIAN_POINT ( 'NONE',  ( 0.000000000000000000, 0.000000000000000000, 60.00000000000000000 ) ) ;
#17852 = EDGE_CURVE ( 'NONE', #35528, #8976, #22259, .T. ) ;
#17853 = CARTESIAN_POINT ( 'NONE',  ( -37.99999897736217491, -113.9929510916434339, 12.62466071271733092 ) ) ;
#17854 = EDGE_CURVE ( 'NONE', #33264, #18917, #32631, .T. ) ;
#17855 = VECTOR ( 'NONE', #25267, 1000.000000000000000 ) ;
#17856 = CARTESIAN_POINT ( 'NONE',  ( 0.000000000000000000, -7.162210897276083621, 51.50439529848826936 ) ) ;
#17857 = EDGE_CURVE ( 'NONE', #7400, #22893, #21665, .T. ) ;
#17858 = CARTESIAN_POINT ( 'NONE',  ( -35.50000000000000000, -113.9929510916434339, 12.50851088611648265 ) ) ;
#17859 = CARTESIAN_POINT ( 'NONE',  ( -35.50400759022158326, -115.9929510916434481, 12.68378527132497524 ) ) ;
#17860 = UNCERTAINTY_MEASURE_WITH_UNIT (LENGTH_MEASURE( 1.000000000000000082E-05 ), #34474, 'distance_accuracy_value', 'NONE');
#17861 = CARTESIAN_POINT ( 'NONE',  ( 7.999999999999992895, -27.43636312076294814, -38.14186064215180494 ) ) ;
#17862 = PLANE ( 'NONE',  #25006 ) ;
#17863 = EDGE_CURVE ( 'NONE', #35305, #10821, #26967, .T. ) ;
#17864 = EDGE_CURVE ( 'NONE', #5260, #16053, #5039, .T. ) ;
#17865 = MECHANICAL_DESIGN_GEOMETRIC_PRESENTATION_REPRESENTATION (  '', ( #17268 ), #2383 ) ;
#17866 = CARTESIAN_POINT ( 'NONE',  ( 4.000000000000000000, 4.627536653468036720E-16, 55.00000000000000000 ) ) ;
#17867 = CARTESIAN_POINT ( 'NONE',  ( -1.600000000000004086, -12.74999999999999822, -1.200000000000006617 ) ) ;
#17868 = CARTESIAN_POINT ( 'NONE',  ( -39.49999999999999289, -1.338792908815551458E-14, 114.0000000000000000 ) ) ;
#17869 = ORIENTED_EDGE ( 'NONE', *, *, #6334, .T. ) ;
#17870 = DIRECTION ( 'NONE',  ( 0.000000000000000000, 0.3681245526846719240, 0.9297764858882537897 ) ) ;
#17871 = CARTESIAN_POINT ( 'NONE',  ( -35.50000000000000711, -113.4307644833805000, -1.624782352598427959 ) ) ;
#17872 = DIRECTION ( 'NONE',  ( -1.000000000000000000, 0.000000000000000000, -0.000000000000000000 ) ) ;
#17873 = CONTEXT_DEPENDENT_SHAPE_REPRESENTATION ( #699, #23014 ) ;
#17874 = DIRECTION ( 'NONE',  ( 0.000000000000000000, 0.000000000000000000, -1.000000000000000000 ) ) ;
#17875 = CARTESIAN_POINT ( 'NONE',  ( 0.000000000000000000, 0.000000000000000000, 35.10000000000000142 ) ) ;
#17876 = ADVANCED_FACE ( 'NONE', ( #10215 ), #4471, .T. ) ;
#17877 = VERTEX_POINT ( 'NONE', #27138 ) ;
#17878 = CYLINDRICAL_SURFACE ( 'NONE', #28527, 20.00000000000000355 ) ;
#17879 = CARTESIAN_POINT ( 'NONE',  ( -34.50000000000000000, -116.6134300264884445, -1.853877267570539944 ) ) ;
#17880 = PLANE ( 'NONE',  #29535 ) ;
#17881 = ORIENTED_EDGE ( 'NONE', *, *, #23388, .F. ) ;
#17882 = VERTEX_POINT ( 'NONE', #10027 ) ;
#17883 = CIRCLE ( 'NONE', #26523, 4.000000000000000000 ) ;
#17884 = CARTESIAN_POINT ( 'NONE',  ( -37.35495115944176803, -115.0245472910329880, 8.965225545821551734 ) ) ;
#17885 = ORIENTED_EDGE ( 'NONE', *, *, #31358, .F. ) ;
#17886 = VERTEX_POINT ( 'NONE', #35074 ) ;
#17887 = ORIENTED_EDGE ( 'NONE', *, *, #35544, .T. ) ;
#17888 = CARTESIAN_POINT ( 'NONE',  ( -35.50000000000000000, -115.0140978167143402, -0.6247823525984417259 ) ) ;
#17889 = AXIS2_PLACEMENT_3D ( 'NONE', #33685, #14590, #25603 ) ;
#17890 = VECTOR ( 'NONE', #7177, 1000.000000000000000 ) ;
#17891 = DIRECTION ( 'NONE',  ( 0.000000000000000000, 0.8660254037844398178, -0.4999999999999981681 ) ) ;
#17892 = EDGE_CURVE ( 'NONE', #32586, #17665, #29764, .T. ) ;
#17893 = CARTESIAN_POINT ( 'NONE',  ( -44.00000000000000000, 0.000000000000000000, 0.000000000000000000 ) ) ;
#17895 = EDGE_CURVE ( 'NONE', #15452, #23013, #18826, .T. ) ;
#17894 = APPLICATION_CONTEXT ( 'automotive_design' ) ;
#17896 = CARTESIAN_POINT ( 'NONE',  ( -35.50000000000000711, -114.9929510916434339, 12.39849696637031506 ) ) ;
#17897 = EDGE_CURVE ( 'NONE', #17469, #2729, #10565, .T. ) ;
#17898 = DIRECTION ( 'NONE',  ( -1.000000000000000000, -0.000000000000000000, -0.000000000000000000 ) ) ;
#17899 = CARTESIAN_POINT ( 'NONE',  ( -36.15625000000007816, -114.9929510916434339, 14.11852480586264846 ) ) ;
#17900 = DIRECTION ( 'NONE',  ( -1.000000000000000000, 0.000000000000000000, 0.000000000000000000 ) ) ;
#17901 = UNCERTAINTY_MEASURE_WITH_UNIT (LENGTH_MEASURE( 1.000000000000000082E-05 ), #5668, 'distance_accuracy_value', 'NONE');
#17902 = EDGE_CURVE ( 'NONE', #272, #30478, #7671, .T. ) ;
#17903 = DIRECTION ( 'NONE',  ( 0.000000000000000000, 0.000000000000000000, 1.000000000000000000 ) ) ;
#17904 = ORIENTED_EDGE ( 'NONE', *, *, #25856, .F. ) ;
#17905 = CARTESIAN_POINT ( 'NONE',  ( -35.50000000000000000, -115.9929510916434481, 12.17846912687782712 ) ) ;
#17906 = CARTESIAN_POINT ( 'NONE',  ( -35.50000000000000711, -116.0140896356112989, -0.6575071456984549201 ) ) ;
#17907 = DIRECTION ( 'NONE',  ( 8.645950338799857827E-17, -6.938893903907203726E-17, -1.000000000000000000 ) ) ;
#17908 = EDGE_CURVE ( 'NONE', #17702, #5884, #18482, .T. ) ;
#17909 = LINE ( 'NONE', #15026, #1448 ) ;
#17910 = DIRECTION ( 'NONE',  ( 1.734723475976807094E-16, -1.000000000000000000, 0.000000000000000000 ) ) ;
#17911 = DIRECTION ( 'NONE',  ( -8.708451184622495809E-17, 6.938893903907203726E-17, 1.000000000000000000 ) ) ;
#17912 = CARTESIAN_POINT ( 'NONE',  ( -4.000000000000000000, -2.710505431213761085E-17, 45.00000000000000000 ) ) ;
#17913 = CARTESIAN_POINT ( 'NONE',  ( 4.000000000000000000, 17.56975900509174693, 9.555290079479316745 ) ) ;
#17914 = CARTESIAN_POINT ( 'NONE',  ( 0.000000000000000000, -22.82995208772657492, -41.06517797613687293 ) ) ;
#17915 = ORIENTED_EDGE ( 'NONE', *, *, #21344, .F. ) ;
#17916 = AXIS2_PLACEMENT_3D ( 'NONE', #10301, #21262, #32262 ) ;
#17917 = PRESENTATION_LAYER_ASSIGNMENT (  '', '', ( #28264 ) ) ;
#17918 = CARTESIAN_POINT ( 'NONE',  ( -37.99999999999998579, -114.0592624029313242, 4.746475545821549957 ) ) ;
#17919 = FACE_OUTER_BOUND ( 'NONE', #31974, .T. ) ;
#17920 = CARTESIAN_POINT ( 'NONE',  ( 8.000000000000000000, 0.000000000000000000, 0.000000000000000000 ) ) ;
#17921 = ORIENTED_EDGE ( 'NONE', *, *, #34184, .T. ) ;
#17922 = ORIENTED_EDGE ( 'NONE', *, *, #16282, .F. ) ;
#17923 = DIRECTION ( 'NONE',  ( -1.000000000000000000, 0.000000000000000000, 0.000000000000000000 ) ) ;
#17924 = FACE_OUTER_BOUND ( 'NONE', #8753, .T. ) ;
#17925 = ORIENTED_EDGE ( 'NONE', *, *, #20497, .T. ) ;
#17926 = CARTESIAN_POINT ( 'NONE',  ( -34.02454729103297382, -112.6980969099494132, 9.902725545821553510 ) ) ;
#17927 = ORIENTED_EDGE ( 'NONE', *, *, #30141, .F. ) ;
#17928 = CARTESIAN_POINT ( 'NONE',  ( 8.000000000000007105, -3.753907720748892007, -8.725776631572756514 ) ) ;
#17929 = COLOUR_RGB ( '', 0.09019608, 0.27058824, 0.51372549) ;
#17930 = CARTESIAN_POINT ( 'NONE',  ( 3.872983346207517386, -1.000000000000028644, -52.50000000000000000 ) ) ;
#17931 = DIRECTION ( 'NONE',  ( 0.000000000000000000, 0.000000000000000000, 1.000000000000000000 ) ) ;
#17932 = DIRECTION ( 'NONE',  ( 0.000000000000000000, -0.9822872507286903865, 0.1873813145857150253 ) ) ;
#17933 = ORIENTED_EDGE ( 'NONE', *, *, #11285, .F. ) ;
#17934 = EDGE_LOOP ( 'NONE', ( #5119, #21422, #5347, #6827 ) ) ;
#17935 = EDGE_CURVE ( 'NONE', #8636, #24798, #17082, .T. ) ;
#17936 = LINE ( 'NONE', #7140, #7024 ) ;
#17937 = CARTESIAN_POINT ( 'NONE',  ( 8.000000000000000000, 0.000000000000000000, 0.000000000000000000 ) ) ;
#17938 = VECTOR ( 'NONE', #31806, 999.9999999999998863 ) ;
#17939 = ORIENTED_EDGE ( 'NONE', *, *, #18521, .T. ) ;
#17940 = DIRECTION ( 'NONE',  ( -1.000000000000000000, -1.836970198721029934E-16, 0.000000000000000000 ) ) ;
#17941 = DIRECTION ( 'NONE',  ( 0.000000000000000000, 0.000000000000000000, 1.000000000000000000 ) ) ;
#17942 = CARTESIAN_POINT ( 'NONE',  ( 8.000000000000000000, -6.085920226791118992, 15.78165944574518775 ) ) ;
#17943 = CARTESIAN_POINT ( 'NONE',  ( -34.50000000000000000, -115.9929510916434481, 12.59652202191340464 ) ) ;
#17944 = CARTESIAN_POINT ( 'NONE',  ( 0.000000000000000000, -38.92705108641750655, 27.21837053747785973 ) ) ;
#17945 = CARTESIAN_POINT ( 'NONE',  ( -37.76916472181487450, -111.9754527089670404, 2.534774454178448710 ) ) ;
#17946 = CARTESIAN_POINT ( 'NONE',  ( -34.50000000000000000, -115.9874658933321001, 10.35517832894335832 ) ) ;
#17947 = DIRECTION ( 'NONE',  ( -1.000000000000000000, 1.502314598737152375E-16, 8.673617379884158732E-17 ) ) ;
#17948 = CYLINDRICAL_SURFACE ( 'NONE', #24775, 8.000000000000000000 ) ;
#17949 = VECTOR ( 'NONE', #32312, 1000.000000000000000 ) ;
#17950 = DIRECTION ( 'NONE',  ( 0.000000000000000000, 0.9848077530122095746, -0.1736481776669212829 ) ) ;
#17951 = PLANE ( 'NONE',  #4318 ) ;
#17952 = CARTESIAN_POINT ( 'NONE',  ( -3.799999999999999822, 4.382607293638566128E-16, -45.89999999999999858 ) ) ;
#17953 = DIRECTION ( 'NONE',  ( 0.000000000000000000, 0.000000000000000000, -1.000000000000000000 ) ) ;
#17954 = VERTEX_POINT ( 'NONE', #29653 ) ;
#17955 = CARTESIAN_POINT ( 'NONE',  ( -40.02454729103296671, -112.8166217158120332, 4.840225545821551734 ) ) ;
#17956 = CARTESIAN_POINT ( 'NONE',  ( 4.000000000000003553, 31.08872492059957793, 41.68322423723111569 ) ) ;
#17957 = CARTESIAN_POINT ( 'NONE',  ( -35.50000000000000000, -113.0140978167138712, 0.2502176474015764263 ) ) ;
#17958 = ORIENTED_EDGE ( 'NONE', *, *, #34999, .T. ) ;
#17959 = ORIENTED_EDGE ( 'NONE', *, *, #12174, .F. ) ;
#17960 = DIRECTION ( 'NONE',  ( -1.000000000000000000, 0.000000000000000000, 0.000000000000000000 ) ) ;
#17961 = AXIS2_PLACEMENT_3D ( 'NONE', #15681, #33492, #16579 ) ;
#17962 = DIRECTION ( 'NONE',  ( 0.000000000000000000, 0.000000000000000000, 1.000000000000000000 ) ) ;
#17963 = ORIENTED_EDGE ( 'NONE', *, *, #8111, .F. ) ;
#17964 = ORIENTED_EDGE ( 'NONE', *, *, #14607, .T. ) ;
#17965 = AXIS2_PLACEMENT_3D ( 'NONE', #22666, #2429, #21842 ) ;
#17966 = VERTEX_POINT ( 'NONE', #4992 ) ;
#17967 = CARTESIAN_POINT ( 'NONE',  ( 3.799999999999999822, 4.653657836759942730E-16, -34.40000000000000568 ) ) ;
#17968 = CARTESIAN_POINT ( 'NONE',  ( -36.23083527818513261, -111.9754527089670404, 8.215225545821549957 ) ) ;
#17969 = DIRECTION ( 'NONE',  ( 1.000000000000000000, 0.000000000000000000, 0.000000000000000000 ) ) ;
#17970 = DIRECTION ( 'NONE',  ( -1.000000000000000000, 0.000000000000000000, 0.000000000000000000 ) ) ;
#17971 = ORIENTED_EDGE ( 'NONE', *, *, #15082, .T. ) ;
#17972 = ORIENTED_EDGE ( 'NONE', *, *, #28778, .F. ) ;
#17973 = CIRCLE ( 'NONE', #3636, 22.00000000000000000 ) ;
#17974 = CARTESIAN_POINT ( 'NONE',  ( -35.50000000000000000, -117.0140978167138854, -0.4997823525984417259 ) ) ;
#17975 = CIRCLE ( 'NONE', #11656, 3.999999999999996447 ) ;
#17976 = EDGE_CURVE ( 'NONE', #3480, #5736, #6181, .T. ) ;
#17977 = VECTOR ( 'NONE', #31204, 1000.000000000000000 ) ;
#17978 = DIRECTION ( 'NONE',  ( -1.783119874454246424E-31, -1.187911941725854497E-31, 1.000000000000000000 ) ) ;
#17979 = DIRECTION ( 'NONE',  ( -1.000000000000000000, 0.000000000000000000, 0.000000000000000000 ) ) ;
#17980 = ORIENTED_EDGE ( 'NONE', *, *, #27077, .F. ) ;
#17981 = CARTESIAN_POINT ( 'NONE',  ( -38.00000000000000711, -114.9929510916434339, 12.39849696637031151 ) ) ;
#17982 = VECTOR ( 'NONE', #14818, 1000.000000000000000 ) ;
#17983 = CARTESIAN_POINT ( 'NONE',  ( -34.50000000000000000, -114.9929296450195721, 10.49869535309826674 ) ) ;
#17984 = CIRCLE ( 'NONE', #11097, 19.99999999999998579 ) ;
#17985 = CARTESIAN_POINT ( 'NONE',  ( 0.000000000000000000, -0.5097555531871997836, -19.99350267651955804 ) ) ;
#17986 = CARTESIAN_POINT ( 'NONE',  ( -37.62959469683911351, -114.9929510916434339, 13.10254527216511633 ) ) ;
#17987 = DIRECTION ( 'NONE',  ( -1.000000000000000000, 0.000000000000000000, 0.000000000000000000 ) ) ;
#17988 = EDGE_CURVE ( 'NONE', #15153, #751, #19409, .T. ) ;
#17989 = CARTESIAN_POINT ( 'NONE',  ( -37.52454134262689678, -113.9929510916434339, 14.11837420659362152 ) ) ;
#17990 = DIRECTION ( 'NONE',  ( 1.000000000000000000, 0.000000000000000000, -0.000000000000000000 ) ) ;
#17991 = DIRECTION ( 'NONE',  ( -1.000000000000000000, 0.000000000000000000, 0.000000000000000000 ) ) ;
#17992 = SURFACE_STYLE_USAGE ( .BOTH. , #12613 ) ;
#17993 = ORIENTED_EDGE ( 'NONE', *, *, #13888, .F. ) ;
#17994 = CARTESIAN_POINT ( 'NONE',  ( 7.999999999999992895, 0.000000000000000000, 0.000000000000000000 ) ) ;
#17995 = DIRECTION ( 'NONE',  ( 0.000000000000000000, 0.000000000000000000, -1.000000000000000000 ) ) ;
#17996 = VERTEX_POINT ( 'NONE', #12737 ) ;
#17997 = CARTESIAN_POINT ( 'NONE',  ( -35.83891589277640577, -114.9929510916434339, 13.09299768411358222 ) ) ;
#17998 = VERTEX_POINT ( 'NONE', #31993 ) ;
#17999 = CARTESIAN_POINT ( 'NONE',  ( -42.49999999999999289, -27.48076211353304998, 70.99999999999988631 ) ) ;
#18000 = ORIENTED_EDGE ( 'NONE', *, *, #21925, .F. ) ;
#18001 = CIRCLE ( 'NONE', #3663, 47.49900000000001654 ) ;
#18002 = DIRECTION ( 'NONE',  ( 1.000000000000000000, 0.000000000000000000, 0.000000000000000000 ) ) ;
#18003 = ORIENTED_EDGE ( 'NONE', *, *, #28864, .F. ) ;
#18004 = VECTOR ( 'NONE', #18075, 1000.000000000000000 ) ;
#18005 = CARTESIAN_POINT ( 'NONE',  ( -34.50000000000000000, -113.0140978167139991, -0.6091573525984278481 ) ) ;
#18006 = CARTESIAN_POINT ( 'NONE',  ( 4.000000000000003553, 51.85248208264518155, 3.914090171286383146 ) ) ;
#18007 = FACE_OUTER_BOUND ( 'NONE', #990, .T. ) ;
#18008 = ORIENTED_EDGE ( 'NONE', *, *, #11448, .F. ) ;
#18009 = CARTESIAN_POINT ( 'NONE',  ( -38.37230871539094323, -112.5438815906447729, 5.441024454178449155 ) ) ;
#18010 = EDGE_CURVE ( 'NONE', #29619, #24892, #1022, .T. ) ;
#18011 = FACE_OUTER_BOUND ( 'NONE', #2952, .T. ) ;
#18012 = VECTOR ( 'NONE', #36, 1000.000000000000000 ) ;
#18013 = CARTESIAN_POINT ( 'NONE',  ( -35.50000000000000711, -114.5974311500472425, -1.624782352598427959 ) ) ;
#18014 = CIRCLE ( 'NONE', #12272, 4.000000000000000000 ) ;
#18015 = ORIENTED_EDGE ( 'NONE', *, *, #24298, .T. ) ;
#18016 = ORIENTED_EDGE ( 'NONE', *, *, #9265, .F. ) ;
#18017 = CARTESIAN_POINT ( 'NONE',  ( 8.000000000000000000, 15.46619997295644389, -1.007799283846741556 ) ) ;
#18018 = AXIS2_PLACEMENT_3D ( 'NONE', #20925, #12856, #23834 ) ;
#18019 = CARTESIAN_POINT ( 'NONE',  ( 0.000000000000000000, 40.47821179127715396, 32.64221760512774040 ) ) ;
#18020 = VERTEX_POINT ( 'NONE', #7850 ) ;
#18021 = EDGE_LOOP ( 'NONE', ( #8671, #7033, #4717, #11723 ) ) ;
#18022 = CARTESIAN_POINT ( 'NONE',  ( -34.50000000000000000, -113.5133328644208746, 2.949007337991939259 ) ) ;
#18023 = CARTESIAN_POINT ( 'NONE',  ( -35.50000000000000711, -112.0140900043112282, 0.8439677466545482121 ) ) ;
#18024 = EDGE_CURVE ( 'NONE', #2854, #18471, #24426, .T. ) ;
#18025 = EDGE_CURVE ( 'NONE', #9, #33840, #26317, .T. ) ;
#18026 = CARTESIAN_POINT ( 'NONE',  ( 0.000000000000000000, -9.744342220503076746, -46.48873837489808380 ) ) ;
#18027 = ORIENTED_EDGE ( 'NONE', *, *, #18927, .T. ) ;
#18028 = ORIENTED_EDGE ( 'NONE', *, *, #19643, .T. ) ;
#18029 = CARTESIAN_POINT ( 'NONE',  ( -4.000000000000000000, -2.710505431213761085E-17, -55.00000000000000000 ) ) ;
#18030 = AXIS2_PLACEMENT_3D ( 'NONE', #29128, #34531, #31634 ) ;
#18031 = CARTESIAN_POINT ( 'NONE',  ( -38.00000000000000711, -113.9929510916434339, 12.50851088611646311 ) ) ;
#18032 = CARTESIAN_POINT ( 'NONE',  ( -1.479000000000008086, 0.000000000000000000, 0.000000000000000000 ) ) ;
#18033 = EDGE_CURVE ( 'NONE', #6113, #35401, #35415, .T. ) ;
#18034 = CARTESIAN_POINT ( 'NONE',  ( -35.50000000000000000, -113.9929510916434339, 11.21034663311132107 ) ) ;
#18035 = EDGE_CURVE ( 'NONE', #22481, #26780, #19949, .T. ) ;
#18036 = CARTESIAN_POINT ( 'NONE',  ( -35.50000000000000000, -115.9710363517788068, 10.20486393345008835 ) ) ;
#18037 = CYLINDRICAL_SURFACE ( 'NONE', #7253, 13.99999999999999822 ) ;
#18039 = CIRCLE ( 'NONE', #14558, 9.499000000000000554 ) ;
#18038 = CARTESIAN_POINT ( 'NONE',  ( 7.999999999999992895, -42.41764978026620270, 20.20639853260275487 ) ) ;
#18040 = AXIS2_PLACEMENT_3D ( 'NONE', #22950, #6930, #6394 ) ;
#18041 = ORIENTED_EDGE ( 'NONE', *, *, #26455, .F. ) ;
#18042 = DIRECTION ( 'NONE',  ( -1.000000000000000000, 0.000000000000000000, 0.000000000000000000 ) ) ;
#18043 = DIRECTION ( 'NONE',  ( 0.000000000000000000, 0.000000000000000000, 1.000000000000000000 ) ) ;
#18044 = DIRECTION ( 'NONE',  ( 0.000000000000000000, 0.5877852522924685852, 0.8090169943749506709 ) ) ;
#18045 = VERTEX_POINT ( 'NONE', #16478 ) ;
#18046 = CARTESIAN_POINT ( 'NONE',  ( 7.999999999999992895, 0.000000000000000000, 0.000000000000000000 ) ) ;
#18047 = CARTESIAN_POINT ( 'NONE',  ( -35.50000000000000711, -113.1807644833805426, -1.624782352598427959 ) ) ;
#18048 = CARTESIAN_POINT ( 'NONE',  ( 7.999999999999992895, -13.56094713063537327, -50.20060470671755581 ) ) ;
#18049 = ITEM_DEFINED_TRANSFORMATION ( 'NONE', 'NONE', #14988,  #21307 ) ;
#18050 = DIRECTION ( 'NONE',  ( -1.000000000000000000, 1.110223024625156540E-16, 0.000000000000000000 ) ) ;
#18051 = DIRECTION ( 'NONE',  ( 1.000000000000000000, -4.524158825347490025E-15, -1.169797080839617330E-15 ) ) ;
#18052 = EDGE_CURVE ( 'NONE', #519, #32655, #4484, .T. ) ;
#18053 = ORIENTED_EDGE ( 'NONE', *, *, #13493, .T. ) ;
#18054 = DIRECTION ( 'NONE',  ( 0.000000000000000000, 0.000000000000000000, 1.000000000000000000 ) ) ;
#18055 = CARTESIAN_POINT ( 'NONE',  ( -35.50000000000000000, -113.5133328644208746, 2.949007337991939259 ) ) ;
#18056 = DIRECTION ( 'NONE',  ( -1.000000000000000000, -0.000000000000000000, -0.000000000000000000 ) ) ;
#18057 = VERTEX_POINT ( 'NONE', #14307 ) ;
#18058 = ORIENTED_EDGE ( 'NONE', *, *, #23996, .F. ) ;
#18059 = CARTESIAN_POINT ( 'NONE',  ( -37.99999999999998579, -113.9407375970686758, 5.253524454178449155 ) ) ;
#18060 = ORIENTED_EDGE ( 'NONE', *, *, #2042, .F. ) ;
#18061 = ORIENTED_EDGE ( 'NONE', *, *, #31055, .F. ) ;
#18062 = CARTESIAN_POINT ( 'NONE',  ( -35.50000000000000000, -114.3474311500471572, -0.6247823525984269599 ) ) ;
#18063 = SHAPE_REPRESENTATION ( 'shaft 3', ( #21307 ), #26556 ) ;
#18064 = VECTOR ( 'NONE', #15435, 1000.000000000000000 ) ;
#18065 = ADVANCED_FACE ( 'NONE', ( #22411 ), #30536, .T. ) ;
#18066 = AXIS2_PLACEMENT_3D ( 'NONE', #19066, #29711, #5057 ) ;
#18067 = EDGE_CURVE ( 'NONE', #23561, #14501, #16831, .T. ) ;
#18068 = EDGE_CURVE ( 'NONE', #4435, #34390, #9650, .T. ) ;
#18069 = DIRECTION ( 'NONE',  ( 1.000000000000000000, -5.339440136655842133E-16, -1.047965281155519420E-16 ) ) ;
#18070 = DIRECTION ( 'NONE',  ( 1.000000000000000000, 0.000000000000000000, 0.000000000000000000 ) ) ;
#18071 = CARTESIAN_POINT ( 'NONE',  ( -36.00585935943767169, -114.9929510916434339, 13.11852578240983291 ) ) ;
#18072 = DIRECTION ( 'NONE',  ( -9.266685234918781277E-17, -7.036038418561930364E-15, 1.000000000000000000 ) ) ;
#18073 = EDGE_CURVE ( 'NONE', #16796, #6343, #29224, .T. ) ;
#18074 = CARTESIAN_POINT ( 'NONE',  ( -34.80050084267117683, -114.9929510916434339, 13.54034599209289169 ) ) ;
#18075 = DIRECTION ( 'NONE',  ( -1.000000000000000000, 0.000000000000000000, 0.000000000000000000 ) ) ;
#18076 = DIRECTION ( 'NONE',  ( 0.000000000000000000, 0.8660254037844398178, -0.4999999999999980016 ) ) ;
#18077 = ORIENTED_EDGE ( 'NONE', *, *, #24468, .T. ) ;
#18078 = CARTESIAN_POINT ( 'NONE',  ( -35.51597953369717686, -115.9929510916434481, 12.74811950270164473 ) ) ;
#18079 = CARTESIAN_POINT ( 'NONE',  ( -35.50000000000000711, -115.3362660311619692, -1.573728109101206085 ) ) ;
#18080 = DIRECTION ( 'NONE',  ( 0.000000000000000000, -0.8660254037844329345, -0.5000000000000101030 ) ) ;
#18081 = CARTESIAN_POINT ( 'NONE',  ( 8.000000000000000000, 17.06000345190455292, -10.43821259704003346 ) ) ;
#18082 = PLANE ( 'NONE',  #23378 ) ;
#18083 = ORIENTED_EDGE ( 'NONE', *, *, #13107, .F. ) ;
#18084 = DIRECTION ( 'NONE',  ( 0.000000000000000000, 0.000000000000000000, 1.000000000000000000 ) ) ;
#18085 = DIRECTION ( 'NONE',  ( 0.000000000000000000, 0.000000000000000000, 1.000000000000000000 ) ) ;
#18086 = AXIS2_PLACEMENT_3D ( 'NONE', #19721, #28043, #17028 ) ;
#18087 = VECTOR ( 'NONE', #2143, 1000.000000000000000 ) ;
#18088 = CARTESIAN_POINT ( 'NONE',  ( 7.999999999999992895, 46.19362259308833529, 8.585149169758651055 ) ) ;
#18089 = CARTESIAN_POINT ( 'NONE',  ( 0.000000000000000000, 3.872983346207417021, -1.000000000000000000 ) ) ;
#18090 = EDGE_LOOP ( 'NONE', ( #8808, #27288, #14062, #31756 ) ) ;
#18091 = CARTESIAN_POINT ( 'NONE',  ( -36.52652403469556930, -113.0245472910329880, 4.222274454178449155 ) ) ;
#18092 = DIRECTION ( 'NONE',  ( -1.000000000000000000, -0.000000000000000000, 0.000000000000000000 ) ) ;
#18093 = FACE_OUTER_BOUND ( 'NONE', #33961, .T. ) ;
#18094 = EDGE_CURVE ( 'NONE', #10384, #7481, #27838, .T. ) ;
#18095 = AXIS2_PLACEMENT_3D ( 'NONE', #35090, #32365, #1599 ) ;
#18096 = ORIENTED_EDGE ( 'NONE', *, *, #28925, .F. ) ;
#18097 = VERTEX_POINT ( 'NONE', #25136 ) ;
#18098 = FILL_AREA_STYLE_COLOUR ( '', #19933 ) ;
#18099 = ADVANCED_FACE ( 'NONE', ( #24785 ), #11443, .T. ) ;
#18100 = CYLINDRICAL_SURFACE ( 'NONE', #16920, 3.799999999999999822 ) ;
#18101 = ORIENTED_EDGE ( 'NONE', *, *, #1745, .F. ) ;
#18102 = CARTESIAN_POINT ( 'NONE',  ( -36.11231047232249125, -115.9754527089670262, 2.777725545821550845 ) ) ;
#18103 = ORIENTED_EDGE ( 'NONE', *, *, #5498, .T. ) ;
#18104 = CIRCLE ( 'NONE', #2612, 11.00000000000001066 ) ;
#18105 = ORIENTED_EDGE ( 'NONE', *, *, #27920, .F. ) ;
#18106 = CARTESIAN_POINT ( 'NONE',  ( 0.000000000000000000, 38.92705108641732181, 27.21837053747812263 ) ) ;
#18107 = LINE ( 'NONE', #4462, #1076 ) ;
#18108 = ADVANCED_FACE ( 'NONE', ( #33575 ), #19187, .T. ) ;
#18109 = EDGE_CURVE ( 'NONE', #20427, #18045, #16556, .T. ) ;
#18110 = CARTESIAN_POINT ( 'NONE',  ( 2.000000000000001776, 0.000000000000000000, 0.000000000000000000 ) ) ;
#18111 = VERTEX_POINT ( 'NONE', #16293 ) ;
#18112 = ORIENTED_EDGE ( 'NONE', *, *, #8873, .F. ) ;
#18113 = AXIS2_PLACEMENT_3D ( 'NONE', #5404, #24659, #30063 ) ;
#18114 = VECTOR ( 'NONE', #25324, 1000.000000000000000 ) ;
#18115 = CYLINDRICAL_SURFACE ( 'NONE', #23110, 13.99999999999999822 ) ;
#18116 = DIRECTION ( 'NONE',  ( -1.000000000000000000, 0.000000000000000000, -0.000000000000000000 ) ) ;
#18117 = EDGE_LOOP ( 'NONE', ( #27274, #35212 ) ) ;
#18118 = FACE_OUTER_BOUND ( 'NONE', #20155, .T. ) ;
#18119 = CIRCLE ( 'NONE', #16391, 4.000000000000000000 ) ;
#18120 = FACE_OUTER_BOUND ( 'NONE', #16546, .T. ) ;
#18121 = DIRECTION ( 'NONE',  ( 0.000000000000000000, 0.000000000000000000, 1.000000000000000000 ) ) ;
#18122 = AXIS2_PLACEMENT_3D ( 'NONE', #17212, #1889, #9306 ) ;
#18123 = CARTESIAN_POINT ( 'NONE',  ( -34.50000000000000000, -115.9929510916434481, 12.50851088611648265 ) ) ;
#18124 = DIRECTION ( 'NONE',  ( 1.000000000000000000, 1.734723475976807094E-16, 0.000000000000000000 ) ) ;
#18125 = CARTESIAN_POINT ( 'NONE',  ( -34.97545270896703329, -113.2308352781851397, 7.409774454178450043 ) ) ;
#18126 = CARTESIAN_POINT ( 'NONE',  ( -34.50000000000000000, -115.9929510916434481, 12.57451923796416260 ) ) ;
#18127 = PLANE ( 'NONE',  #10781 ) ;
#18128 = CARTESIAN_POINT ( 'NONE',  ( 0.000000000000000000, 0.000000000000000000, 0.000000000000000000 ) ) ;
#18129 = CIRCLE ( 'NONE', #33104, 7.199999999999992184 ) ;
#18130 = FACE_OUTER_BOUND ( 'NONE', #3167, .T. ) ;
#18131 = DIRECTION ( 'NONE',  ( 0.000000000000000000, 0.000000000000000000, -1.000000000000000000 ) ) ;
#18132 = CARTESIAN_POINT ( 'NONE',  ( 8.000000000000000000, -15.46619997295643856, 1.007799283846635863 ) ) ;
#18133 =( LENGTH_UNIT ( ) NAMED_UNIT ( * ) SI_UNIT ( .MILLI., .METRE. ) );
#18134 = ORIENTED_EDGE ( 'NONE', *, *, #33890, .T. ) ;
#18135 = CARTESIAN_POINT ( 'NONE',  ( -36.94073759706868287, -116.9999999999999858, 7.371475545821551734 ) ) ;
#18136 = LINE ( 'NONE', #26983, #22134 ) ;
#18137 = CARTESIAN_POINT ( 'NONE',  ( -35.50000000000000000, -113.0140978167137860, -0.6247823525984055326 ) ) ;
#18138 = EDGE_CURVE ( 'NONE', #17029, #19012, #33237, .T. ) ;
#18139 = ORIENTED_EDGE ( 'NONE', *, *, #34186, .T. ) ;
#18140 = ORIENTED_EDGE ( 'NONE', *, *, #21601, .T. ) ;
#18141 = EDGE_CURVE ( 'NONE', #7789, #13072, #28087, .T. ) ;
#18143 = DIRECTION ( 'NONE',  ( -1.000000000000000000, 0.000000000000000000, 0.000000000000000000 ) ) ;
#18142 = PRODUCT ( 'shaft1', 'shaft1', '', ( #8759 ) ) ;
#18144 = CIRCLE ( 'NONE', #33661, 9.999999999999994671 ) ;
#18145 = DIRECTION ( 'NONE',  ( 0.000000000000000000, 0.000000000000000000, 1.000000000000000000 ) ) ;
#18146 = ORIENTED_EDGE ( 'NONE', *, *, #11236, .F. ) ;
#18147 = VERTEX_POINT ( 'NONE', #33061 ) ;
#18148 = ORIENTED_EDGE ( 'NONE', *, *, #33075, .T. ) ;
#18149 = AXIS2_PLACEMENT_3D ( 'NONE', #27803, #17318, #17145 ) ;
#18150 = VECTOR ( 'NONE', #14365, 1000.000000000000000 ) ;
#18151 = DIRECTION ( 'NONE',  ( -1.000000000000000000, 0.000000000000000000, 0.000000000000000000 ) ) ;
#18152 = CARTESIAN_POINT ( 'NONE',  ( -35.54388159064475872, -115.3723087153909432, 8.683975545821551734 ) ) ;
#18153 = DIRECTION ( 'NONE',  ( 0.000000000000000000, 0.000000000000000000, -1.000000000000000000 ) ) ;
#18154 = CARTESIAN_POINT ( 'NONE',  ( 8.000000000000000000, 5.400000000000000355, -0.9999999999999985567 ) ) ;
#18156 = VERTEX_POINT ( 'NONE', #16656 ) ;
#18155 = VECTOR ( 'NONE', #23724, 1000.000000000000000 ) ;
#18157 = VERTEX_POINT ( 'NONE', #8726 ) ;
#18158 = CARTESIAN_POINT ( 'NONE',  ( -35.50000000000000711, -112.0209493036498287, 0.9959249592223760050 ) ) ;
#18159 = APPLICATION_CONTEXT ( 'automotive_design' ) ;
#18160 = CARTESIAN_POINT ( 'NONE',  ( 7.999999999999992895, 0.000000000000000000, 0.000000000000000000 ) ) ;
#18161 = ADVANCED_FACE ( 'NONE', ( #2654 ), #11266, .T. ) ;
#18162 = CARTESIAN_POINT ( 'NONE',  ( 8.000000000000000000, 16.71027810728552154, 4.579731798933998732 ) ) ;
#18163 = ORIENTED_EDGE ( 'NONE', *, *, #21166, .T. ) ;
#18164 = CARTESIAN_POINT ( 'NONE',  ( -38.00000000000000711, -114.9929510916434339, 12.50851088611646311 ) ) ;
#18165 = DIRECTION ( 'NONE',  ( -1.000000000000000000, 0.000000000000000000, 0.000000000000000000 ) ) ;
#18166 = CARTESIAN_POINT ( 'NONE',  ( -34.50000000000000000, -114.9929510916434339, 10.51175824272318415 ) ) ;
#18167 = DIRECTION ( 'NONE',  ( 0.000000000000000000, 0.8660254037844362651, 0.5000000000000042188 ) ) ;
#18168 = CARTESIAN_POINT ( 'NONE',  ( -37.46874999999996447, -114.9929510916434339, 13.11852480586264669 ) ) ;
#18169 = DIRECTION ( 'NONE',  ( 0.000000000000000000, 0.9510565162951523099, 0.3090169943749513370 ) ) ;
#18170 = CARTESIAN_POINT ( 'NONE',  ( -34.50000000000000000, -114.9929510916434339, 10.68227981832981044 ) ) ;
#18171 = CARTESIAN_POINT ( 'NONE',  ( -35.00000000000000000, -114.0000000000003411, 9.500000000000035527 ) ) ;
#18172 = VECTOR ( 'NONE', #26979, 1000.000000000000000 ) ;
#18173 = CARTESIAN_POINT ( 'NONE',  ( -37.89983305244309975, -114.9929510916434339, 12.92579853460519246 ) ) ;
#18174 = SURFACE_STYLE_FILL_AREA ( #28457 ) ;
#18175 = ORIENTED_EDGE ( 'NONE', *, *, #2261, .T. ) ;
#18176 = DIRECTION ( 'NONE',  ( -1.000000000000000000, -0.000000000000000000, 0.000000000000000000 ) ) ;
#18177 = LINE ( 'NONE', #34042, #33017 ) ;
#18178 = VERTEX_POINT ( 'NONE', #19695 ) ;
#18179 = CARTESIAN_POINT ( 'NONE',  ( -37.24999999999992895, -114.9929510916434339, 13.11852480586264669 ) ) ;
#18180 = VERTEX_POINT ( 'NONE', #632 ) ;
#18181 = DIRECTION ( 'NONE',  ( -1.000000000000000000, 0.000000000000000000, -0.000000000000000000 ) ) ;
#18182 = VECTOR ( 'NONE', #19852, 1000.000000000000000 ) ;
#18183 = CARTESIAN_POINT ( 'NONE',  ( 0.000000000000000000, 11.27190672109280811, -0.3151488735047974776 ) ) ;
#18184 = CIRCLE ( 'NONE', #4411, 3.799999999999999822 ) ;
#18185 = ORIENTED_EDGE ( 'NONE', *, *, #18732, .T. ) ;
#18186 = CYLINDRICAL_SURFACE ( 'NONE', #11318, 5.000000000000004441 ) ;
#18187 = ORIENTED_EDGE ( 'NONE', *, *, #10138, .F. ) ;
#18188 = EDGE_CURVE ( 'NONE', #31626, #24139, #11611, .T. ) ;
#18189 = CARTESIAN_POINT ( 'NONE',  ( -34.50000000000000000, -113.0140978167138712, 0.5627176474015715968 ) ) ;
#18190 = CARTESIAN_POINT ( 'NONE',  ( 0.000000000000000000, -11.90021268425586953, 45.45261810511210143 ) ) ;
#18191 = CARTESIAN_POINT ( 'NONE',  ( -36.11231047232249125, -112.0245472910329880, 8.722274454178448266 ) ) ;
#18192 = EDGE_LOOP ( 'NONE', ( #12710, #26529 ) ) ;
#18193 = CARTESIAN_POINT ( 'NONE',  ( -39.99999999999999289, -113.9407375970686758, 2.253524454178448710 ) ) ;
#18194 = AXIS2_PLACEMENT_3D ( 'NONE', #20146, #28639, #23409 ) ;
#18195 = CARTESIAN_POINT ( 'NONE',  ( 7.999999999999992895, 34.03046037009305280, -33.13733193845769165 ) ) ;
#18196 = AXIS2_PLACEMENT_3D ( 'NONE', #26493, #7869, #18858 ) ;
#18197 = CARTESIAN_POINT ( 'NONE',  ( -35.50000000000000711, -113.2224311500466030, -1.624782352598427959 ) ) ;
#18198 = ORIENTED_EDGE ( 'NONE', *, *, #8796, .F. ) ;
#18199 = ORIENTED_EDGE ( 'NONE', *, *, #154, .F. ) ;
#18200 = CARTESIAN_POINT ( 'NONE',  ( 70.00001200000002655, -24.93377057609608727, 81.10410929332670094 ) ) ;
#18201 = ADVANCED_FACE ( 'NONE', ( #13618, #10925 ), #21892, .T. ) ;
#18202 = VECTOR ( 'NONE', #15737, 1000.000000000000000 ) ;
#18203 = LINE ( 'NONE', #12279, #4643 ) ;
#18204 = ORIENTED_EDGE ( 'NONE', *, *, #9885, .F. ) ;
#18205 = ORIENTED_EDGE ( 'NONE', *, *, #15383, .T. ) ;
#18206 = CARTESIAN_POINT ( 'NONE',  ( -34.50000000000000000, -112.7549084230351752, -1.592823285203595285 ) ) ;
#18207 = CIRCLE ( 'NONE', #34305, 3.799999999999999822 ) ;
#18208 = AXIS2_PLACEMENT_3D ( 'NONE', #33247, #19024, #27147 ) ;
#18209 = CARTESIAN_POINT ( 'NONE',  ( -6.896599878636569869, -12.98179148322720167, 0.000000000000000000 ) ) ;
#18210 = ORIENTED_EDGE ( 'NONE', *, *, #20408, .F. ) ;
#18211 = ORIENTED_EDGE ( 'NONE', *, *, #32543, .F. ) ;
#18212 = VECTOR ( 'NONE', #28126, 1000.000000000000000 ) ;
#18213 = DIRECTION ( 'NONE',  ( 1.000000000000000000, -1.110223024625156540E-16, 0.000000000000000000 ) ) ;
#18214 = VECTOR ( 'NONE', #31958, 1000.000000000000000 ) ;
#18215 = CARTESIAN_POINT ( 'NONE',  ( -34.50000000000000000, -113.9929510916436470, 10.50625754673581724 ) ) ;
#18216 = DIRECTION ( 'NONE',  ( 1.000000000000000000, 0.000000000000000000, 0.000000000000000000 ) ) ;
#18217 = CARTESIAN_POINT ( 'NONE',  ( -37.54084996655477369, -113.9929510916434339, 13.11692036158760466 ) ) ;
#18218 = CARTESIAN_POINT ( 'NONE',  ( -37.43749999999998579, -115.9929510916434481, 13.11852480586264846 ) ) ;
#18219 = CYLINDRICAL_SURFACE ( 'NONE', #27923, 20.00000000000000355 ) ;
#18220 = CARTESIAN_POINT ( 'NONE',  ( 4.000000000000000000, -17.06000345190431844, -10.43821259704038695 ) ) ;
#18221 = AXIS2_PLACEMENT_3D ( 'NONE', #14090, #238, #19494 ) ;
#18222 = EDGE_LOOP ( 'NONE', ( #33359, #23795, #17921, #16335 ) ) ;
#18223 = CARTESIAN_POINT ( 'NONE',  ( 7.999999999999992895, -11.46872990052349550, -45.56340405422456996 ) ) ;
#18224 = DIRECTION ( 'NONE',  ( -1.000000000000000000, -0.000000000000000000, -0.000000000000000000 ) ) ;
#18225 = CYLINDRICAL_SURFACE ( 'NONE', #25462, 3.799999999999999822 ) ;
#18226 = ORIENTED_EDGE ( 'NONE', *, *, #31545, .T. ) ;
#18227 = VECTOR ( 'NONE', #27070, 1000.000000000000000 ) ;
#18228 = DIRECTION ( 'NONE',  ( 0.000000000000000000, 0.000000000000000000, -1.000000000000000000 ) ) ;
#18229 = EDGE_CURVE ( 'NONE', #34100, #7117, #23299, .T. ) ;
#18230 = CARTESIAN_POINT ( 'NONE',  ( -35.50000000000000711, -112.0140978167138712, -0.5622823525984296245 ) ) ;
#18231 = CARTESIAN_POINT ( 'NONE',  ( 0.000000000000000000, 0.000000000000000000, -39.50000000000000711 ) ) ;
#18232 = EDGE_CURVE ( 'NONE', #15796, #14501, #13695, .T. ) ;
#18233 = AXIS2_PLACEMENT_3D ( 'NONE', #21320, #4086, #7469 ) ;
#18234 = VECTOR ( 'NONE', #12986, 1000.000000000000000 ) ;
#18235 = CARTESIAN_POINT ( 'NONE',  ( 0.000000000000000000, -1.000000000000001554, -22.00000000000000000 ) ) ;
#18236 = CYLINDRICAL_SURFACE ( 'NONE', #34334, 4.000000000000000000 ) ;
#18237 = ORIENTED_EDGE ( 'NONE', *, *, #26543, .F. ) ;
#18238 = FACE_OUTER_BOUND ( 'NONE', #12437, .T. ) ;
#18239 = CARTESIAN_POINT ( 'NONE',  ( -34.50000000000000000, -111.0301281775997353, -0.8858242144478579716 ) ) ;
#18240 = CARTESIAN_POINT ( 'NONE',  ( 8.000000000000007105, -9.604183132802312173, -5.908880290975638161 ) ) ;
#18241 = EDGE_LOOP ( 'NONE', ( #8895, #26768, #911, #28878 ) ) ;
#18242 = ORIENTED_EDGE ( 'NONE', *, *, #32147, .F. ) ;
#18243 = CARTESIAN_POINT ( 'NONE',  ( -35.99999999999999289, -113.9407375970686758, 9.996475545821549957 ) ) ;
#18244 = EDGE_CURVE ( 'NONE', #33932, #428, #21084, .T. ) ;
#18245 = AXIS2_PLACEMENT_3D ( 'NONE', #21525, #32524, #24616 ) ;
#18246 = CARTESIAN_POINT ( 'NONE',  ( 0.000000000000000000, 0.000000000000000000, 0.000000000000000000 ) ) ;
#18247 = ORIENTED_EDGE ( 'NONE', *, *, #31210, .F. ) ;
#18248 = ORIENTED_EDGE ( 'NONE', *, *, #17424, .F. ) ;
#18249 = CARTESIAN_POINT ( 'NONE',  ( -35.50000000000000000, -115.0140978167138712, 0.3752176474015736507 ) ) ;
#18250 = AXIS2_PLACEMENT_3D ( 'NONE', #3666, #19311, #27799 ) ;
#18251 = FACE_OUTER_BOUND ( 'NONE', #9838, .T. ) ;
#18252 = DIRECTION ( 'NONE',  ( 1.282131172192753642E-16, -6.938893903907203726E-17, -1.000000000000000000 ) ) ;
#18253 = CARTESIAN_POINT ( 'NONE',  ( -35.50000000000000000, -113.9929510916434339, 10.50625754673586876 ) ) ;
#18254 = CARTESIAN_POINT ( 'NONE',  ( 0.000000000000000000, 0.000000000000000000, 65.00000000000000000 ) ) ;
#18255 = CIRCLE ( 'NONE', #2775, 52.00000000000000711 ) ;
#18256 = ADVANCED_FACE ( 'NONE', ( #19869 ), #25852, .T. ) ;
#18257 = CARTESIAN_POINT ( 'NONE',  ( -37.59808119975203766, -114.9929510916434339, 14.11551573851448893 ) ) ;
#18258 = CARTESIAN_POINT ( 'NONE',  ( 8.000000000000000000, -0.3212489022564151142, -16.91141623315864706 ) ) ;
#18259 = CARTESIAN_POINT ( 'NONE',  ( 6.071532165918824830E-15, 1.000000000000000000, 38.00000000000000000 ) ) ;
#18260 = ORIENTED_EDGE ( 'NONE', *, *, #8321, .T. ) ;
#18261 = CARTESIAN_POINT ( 'NONE',  ( -36.24999999999983658, -115.9929510916434481, 13.11852480586264846 ) ) ;
#18262 = CARTESIAN_POINT ( 'NONE',  ( -35.50000000000000711, -113.0557643173828524, -1.624792769101735868 ) ) ;
#18263 = CYLINDRICAL_SURFACE ( 'NONE', #11630, 9.499000000000000554 ) ;
#18264 = DIRECTION ( 'NONE',  ( 1.000000000000000000, -0.000000000000000000, -0.000000000000000000 ) ) ;
#18265 = DIRECTION ( 'NONE',  ( -1.000000000000000000, 0.000000000000000000, -0.000000000000000000 ) ) ;
#18266 = AXIS2_PLACEMENT_3D ( 'NONE', #16213, #24530, #18757 ) ;
#18267 = ORIENTED_EDGE ( 'NONE', *, *, #34873, .F. ) ;
#18268 = LINE ( 'NONE', #12706, #2724 ) ;
#18269 = LINE ( 'NONE', #2097, #4936 ) ;
#18270 = ADVANCED_FACE ( 'NONE', ( #23994 ), #28538, .T. ) ;
#18271 = DIRECTION ( 'NONE',  ( 0.000000000000000000, -0.7705132427757817037, -0.6374239897486988493 ) ) ;
#18272 = LINE ( 'NONE', #15199, #4641 ) ;
#18273 = ORIENTED_EDGE ( 'NONE', *, *, #1824, .F. ) ;
#18274 = EDGE_CURVE ( 'NONE', #11413, #21432, #1350, .T. ) ;
#18275 = AXIS2_PLACEMENT_3D ( 'NONE', #23403, #15277, #10071 ) ;
#18276 = ADVANCED_FACE ( 'NONE', ( #30885 ), #1179, .T. ) ;
#18277 = CARTESIAN_POINT ( 'NONE',  ( -36.33479806579561000, -114.7490116281687165, 3.191024454178448710 ) ) ;
#18278 = DIRECTION ( 'NONE',  ( -1.000000000000000000, 0.000000000000000000, 0.000000000000000000 ) ) ;
#18279 = AXIS2_PLACEMENT_3D ( 'NONE', #11864, #4317, #15083 ) ;
#18280 = DIRECTION ( 'NONE',  ( 0.000000000000000000, 0.000000000000000000, -1.000000000000000000 ) ) ;
#18281 = ORIENTED_EDGE ( 'NONE', *, *, #35204, .F. ) ;
#18282 = ORIENTED_EDGE ( 'NONE', *, *, #30318, .T. ) ;
#18283 = AXIS2_PLACEMENT_3D ( 'NONE', #8937, #17213, #28221 ) ;
#18284 = SURFACE_SIDE_STYLE ('',( #9825 ) ) ;
#18285 = DIRECTION ( 'NONE',  ( 0.000000000000000000, 0.000000000000000000, 1.000000000000000000 ) ) ;
#18286 = EDGE_LOOP ( 'NONE', ( #4711, #16005, #4013, #4000 ) ) ;
#18287 = CARTESIAN_POINT ( 'NONE',  ( -34.83677480945821259, -116.0794154965774965, 5.683975545821551734 ) ) ;
#18288 = EDGE_CURVE ( 'NONE', #29301, #8849, #22333, .T. ) ;
#18289 = ORIENTED_EDGE ( 'NONE', *, *, #28388, .F. ) ;
#18290 = AXIS2_PLACEMENT_3D ( 'NONE', #10421, #27161, #131 ) ;
#18291 = EDGE_CURVE ( 'NONE', #30739, #14603, #21182, .T. ) ;
#18292 = DIRECTION ( 'NONE',  ( 1.000000000000000000, 0.000000000000000000, 0.000000000000000000 ) ) ;
#18293 = ORIENTED_EDGE ( 'NONE', *, *, #2737, .F. ) ;
#18294 = VERTEX_POINT ( 'NONE', #31237 ) ;
#18295 = CARTESIAN_POINT ( 'NONE',  ( 4.000000000000000000, 4.898587196589412829E-16, 60.00000000000000000 ) ) ;
#18296 = DIRECTION ( 'NONE',  ( 0.000000000000000000, -1.000000000000000000, -2.423959199780483078E-15 ) ) ;
#18297 = ORIENTED_EDGE ( 'NONE', *, *, #13449, .T. ) ;
#18298 = ORIENTED_EDGE ( 'NONE', *, *, #22659, .F. ) ;
#18299 = CARTESIAN_POINT ( 'NONE',  ( 8.000000000000000000, -19.83898331853694685, 9.508666619816578347 ) ) ;
#18300 = DIRECTION ( 'NONE',  ( -1.000000000000000000, 0.000000000000000000, 0.000000000000000000 ) ) ;
#18301 = VECTOR ( 'NONE', #10265, 1000.000000000000000 ) ;
#18302 = ORIENTED_EDGE ( 'NONE', *, *, #6638, .F. ) ;
#18303 = DIRECTION ( 'NONE',  ( -1.000000000000000000, 0.000000000000000000, 0.000000000000000000 ) ) ;
#18304 = EDGE_CURVE ( 'NONE', #32416, #1635, #8537, .T. ) ;
#18305 = DIRECTION ( 'NONE',  ( 0.8432271980573221581, -3.471037937261304171E-16, 0.5375573387615479870 ) ) ;
#18306 = CARTESIAN_POINT ( 'NONE',  ( 0.000000000000000000, 11.90021268425554624, 45.45261810511217959 ) ) ;
#18307 = VECTOR ( 'NONE', #15218, 1000.000000000000000 ) ;
#18308 = CARTESIAN_POINT ( 'NONE',  ( -34.50000000000000000, -115.9929510916434481, 10.94631322572069365 ) ) ;
#18309 = EDGE_CURVE ( 'NONE', #16212, #29334, #33268, .T. ) ;
#18310 = CARTESIAN_POINT ( 'NONE',  ( -1.387778780781445676E-14, 0.4273491293403097746, -0.7999999999999951594 ) ) ;
#18311 = CARTESIAN_POINT ( 'NONE',  ( -35.54388159064475872, -112.6276912846090568, 5.816024454178449155 ) ) ;
#18312 = EDGE_CURVE ( 'NONE', #27521, #14212, #29841, .T. ) ;
#18313 = CARTESIAN_POINT ( 'NONE',  ( -34.50000000000000000, -115.9929510916434481, 10.55026311463432087 ) ) ;
#18314 = DIRECTION ( 'NONE',  ( -1.000000000000000000, 0.000000000000000000, 0.000000000000000000 ) ) ;
#18315 = CARTESIAN_POINT ( 'NONE',  ( -37.49999999999999289, -6.699660887819688604, 116.5112005972652014 ) ) ;
#18316 = DIRECTION ( 'NONE',  ( -1.000000000000000000, 0.000000000000000000, 0.000000000000000000 ) ) ;
#18317 = CARTESIAN_POINT ( 'NONE',  ( 8.000000000000000000, 8.931325931664870765, -16.53603053422199665 ) ) ;
#18318 = DIRECTION ( 'NONE',  ( -1.000000000000000000, 0.000000000000000000, 0.000000000000000000 ) ) ;
#18319 = DIRECTION ( 'NONE',  ( 0.000000000000000000, 0.000000000000000000, 1.000000000000000000 ) ) ;
#18320 = VERTEX_POINT ( 'NONE', #20226 ) ;
#18321 = EDGE_CURVE ( 'NONE', #1657, #21466, #18396, .T. ) ;
#18322 = CARTESIAN_POINT ( 'NONE',  ( -39.16322519054178741, -111.9205845034225177, 7.933975545821553510 ) ) ;
#18323 = EDGE_CURVE ( 'NONE', #8621, #32451, #28680, .T. ) ;
#18324 = CARTESIAN_POINT ( 'NONE',  ( -9.999999999999994671, 0.000000000000000000, 0.000000000000000000 ) ) ;
#18325 = CARTESIAN_POINT ( 'NONE',  ( -35.50000000000000711, -116.0140978167138712, 0.3752176474015736507 ) ) ;
#18326 = ORIENTED_EDGE ( 'NONE', *, *, #22451, .T. ) ;
#18327 = ORIENTED_EDGE ( 'NONE', *, *, #8757, .F. ) ;
#18328 = DIRECTION ( 'NONE',  ( -1.000000000000000000, 0.000000000000000000, 0.000000000000000000 ) ) ;
#18329 = LINE ( 'NONE', #10422, #7707 ) ;
#18330 = ORIENTED_EDGE ( 'NONE', *, *, #26960, .F. ) ;
#18331 = CIRCLE ( 'NONE', #23494, 47.49900000000000944 ) ;
#18332 = ORIENTED_EDGE ( 'NONE', *, *, #19909, .T. ) ;
#18333 = ORIENTED_EDGE ( 'NONE', *, *, #7492, .F. ) ;
#18334 = AXIS2_PLACEMENT_3D ( 'NONE', #19456, #548, #33491 ) ;
#18335 = ADVANCED_FACE ( 'NONE', ( #17355 ), #6746, .T. ) ;
#18336 = CIRCLE ( 'NONE', #35600, 47.49900000000000944 ) ;
#18337 = FACE_OUTER_BOUND ( 'NONE', #13604, .T. ) ;
#18338 = CYLINDRICAL_SURFACE ( 'NONE', #13118, 20.00000000000000355 ) ;
#18339 = DIRECTION ( 'NONE',  ( 0.000000000000000000, 0.000000000000000000, -1.000000000000000000 ) ) ;
#18340 = DIRECTION ( 'NONE',  ( -0.000000000000000000, 0.000000000000000000, -1.000000000000000000 ) ) ;
#18341 = ORIENTED_EDGE ( 'NONE', *, *, #31040, .F. ) ;
#18342 = ORIENTED_EDGE ( 'NONE', *, *, #3146, .T. ) ;
#18343 = CARTESIAN_POINT ( 'NONE',  ( -35.50000000000000711, -112.0140900043366088, -0.5935324770972457697 ) ) ;
#18344 = CARTESIAN_POINT ( 'NONE',  ( 0.000000000000000000, 0.000000000000000000, 0.000000000000000000 ) ) ;
#18345 = FACE_OUTER_BOUND ( 'NONE', #14604, .T. ) ;
#18346 = ORIENTED_EDGE ( 'NONE', *, *, #12808, .F. ) ;
#18347 = CYLINDRICAL_SURFACE ( 'NONE', #6301, 52.00000000000000711 ) ;
#18348 = EDGE_CURVE ( 'NONE', #25018, #10010, #20007, .T. ) ;
#18349 = CARTESIAN_POINT ( 'NONE',  ( -34.50000000000000000, -112.1222502514821144, 1.343475657184566296 ) ) ;
#18350 = EDGE_CURVE ( 'NONE', #21046, #19596, #15680, .T. ) ;
#18351 = CARTESIAN_POINT ( 'NONE',  ( -34.50000000000000000, -114.9925223117477202, 10.47601618151863079 ) ) ;
#18352 = DIRECTION ( 'NONE',  ( 0.000000000000000000, 1.000000000000000000, 3.491564676272318479E-15 ) ) ;
#18353 = VECTOR ( 'NONE', #24424, 1000.000000000000000 ) ;
#18354 = CARTESIAN_POINT ( 'NONE',  ( -35.51597953369718397, -114.9929510916434339, 12.74811950270164473 ) ) ;
#18355 = DIRECTION ( 'NONE',  ( -1.000000000000000000, 0.000000000000000000, 0.000000000000000000 ) ) ;
#18356 = CARTESIAN_POINT ( 'NONE',  ( -39.00000000000000000, -113.9929510916434339, 11.73841344789285657 ) ) ;
#18357 = LINE ( 'NONE', #4336, #3340 ) ;
#18358 = DIRECTION ( 'NONE',  ( -1.000000000000000000, 0.000000000000000000, 0.000000000000000000 ) ) ;
#18359 = DIRECTION ( 'NONE',  ( 0.000000000000000000, 0.6845471059286846183, 0.7289686274214153272 ) ) ;
#18360 = ORIENTED_EDGE ( 'NONE', *, *, #3374, .T. ) ;
#18361 = VECTOR ( 'NONE', #18213, 1000.000000000000000 ) ;
#18362 = DIRECTION ( 'NONE',  ( -1.000000000000000000, -0.000000000000000000, 0.000000000000000000 ) ) ;
#18363 = DIRECTION ( 'NONE',  ( 1.000000000000000000, -5.339440136655842133E-16, -1.047965281155519420E-16 ) ) ;
#18364 = ORIENTED_EDGE ( 'NONE', *, *, #13569, .F. ) ;
#18365 = CARTESIAN_POINT ( 'NONE',  ( -37.53269373325071712, -114.9929510916434339, 13.11752178341324360 ) ) ;
#18366 = ORIENTED_EDGE ( 'NONE', *, *, #24422, .T. ) ;
#18367 = ADVANCED_FACE ( 'NONE', ( #26698 ), #15017, .T. ) ;
#18368 = CARTESIAN_POINT ( 'NONE',  ( -35.00000000000000000, -114.0592624029313242, 6.003524454178450043 ) ) ;
#18369 = ADVANCED_FACE ( 'NONE', ( #19098 ), #21615, .T. ) ;
#18370 = CARTESIAN_POINT ( 'NONE',  ( -42.49999999999999289, -20.27980021920970799, 72.12564434701783966 ) ) ;
#18371 = VERTEX_POINT ( 'NONE', #27404 ) ;
#18372 = ORIENTED_EDGE ( 'NONE', *, *, #28415, .T. ) ;
#18373 = DIRECTION ( 'NONE',  ( 0.000000000000000000, -0.9048270524660235736, 0.4257792915650641663 ) ) ;
#18374 = VERTEX_POINT ( 'NONE', #7763 ) ;
#18375 = CARTESIAN_POINT ( 'NONE',  ( -37.05926240293133134, -116.9999999999999858, 3.378524454178448710 ) ) ;
#18376 = APPLICATION_CONTEXT ( 'automotive_design' ) ;
#18377 = CARTESIAN_POINT ( 'NONE',  ( 4.000000000000000000, -19.77827456857337651, 2.969824084036396528 ) ) ;
#18378 = CYLINDRICAL_SURFACE ( 'NONE', #3882, 12.55910585664918422 ) ;
#18379 = ORIENTED_EDGE ( 'NONE', *, *, #35124, .T. ) ;
#18380 = VERTEX_POINT ( 'NONE', #29749 ) ;
#18381 = DIRECTION ( 'NONE',  ( -1.000000000000000000, 0.000000000000000000, 0.000000000000000000 ) ) ;
#18382 = CYLINDRICAL_SURFACE ( 'NONE', #20738, 22.00000000000000000 ) ;
#18383 = VERTEX_POINT ( 'NONE', #13361 ) ;
#18384 = ORIENTED_EDGE ( 'NONE', *, *, #4870, .F. ) ;
#18385 = AXIS2_PLACEMENT_3D ( 'NONE', #30746, #671, #8247 ) ;
#18386 = CARTESIAN_POINT ( 'NONE',  ( -34.50000000000000000, -111.2304026862503719, 1.811733666967775713 ) ) ;
#18387 = CARTESIAN_POINT ( 'NONE',  ( 0.000000000000000000, 11.06713717293239441, 13.55483219355733837 ) ) ;
#18388 = AXIS2_PLACEMENT_3D ( 'NONE', #25327, #33589, #6234 ) ;
#18389 = EDGE_LOOP ( 'NONE', ( #14407, #3869, #10623, #14235 ) ) ;
#18390 = ORIENTED_EDGE ( 'NONE', *, *, #29324, .T. ) ;
#18391 = VERTEX_POINT ( 'NONE', #27227 ) ;
#18392 = CIRCLE ( 'NONE', #22412, 52.00000000000000711 ) ;
#18393 = CARTESIAN_POINT ( 'NONE',  ( -35.50000000000000711, -114.0928965812550757, 9.511088712577292270 ) ) ;
#18394 = EDGE_CURVE ( 'NONE', #19400, #16551, #29576, .T. ) ;
#18395 = CARTESIAN_POINT ( 'NONE',  ( -34.50000000000000000, -113.9917898843777522, 10.50611893782865813 ) ) ;
#18396 = LINE ( 'NONE', #29398, #1671 ) ;
#18397 = PLANE ( 'NONE',  #17359 ) ;
#18398 = CARTESIAN_POINT ( 'NONE',  ( -38.00000000000000711, -113.9929510916434339, 12.59652202191340820 ) ) ;
#18399 = CARTESIAN_POINT ( 'NONE',  ( -37.50818044754229419, -115.9929510916434481, 13.11847460610629845 ) ) ;
#18400 = CARTESIAN_POINT ( 'NONE',  ( 4.000000000000000000, -7.317194182740272446, 18.61340026142649506 ) ) ;
#18401 = CARTESIAN_POINT ( 'NONE',  ( 0.9999999999999453770, -6.008326913195871199, -0.7999999999999951594 ) ) ;
#18402 = ORIENTED_EDGE ( 'NONE', *, *, #30173, .F. ) ;
#18403 = AXIS2_PLACEMENT_3D ( 'NONE', #18254, #20593, #14843 ) ;
#18404 = CARTESIAN_POINT ( 'NONE',  ( 8.000000000000000000, 0.000000000000000000, 0.000000000000000000 ) ) ;
#18405 = DIRECTION ( 'NONE',  ( -1.000000000000000000, 0.000000000000000000, 0.000000000000000000 ) ) ;
#18406 = DIRECTION ( 'NONE',  ( 1.000000000000000000, -5.339440136655842133E-16, -1.047965281155519420E-16 ) ) ;
#18407 = ORIENTED_EDGE ( 'NONE', *, *, #4026, .F. ) ;
#18408 = AXIS2_PLACEMENT_3D ( 'NONE', #22066, #27493, #25132 ) ;
#18409 = PLANE ( 'NONE',  #10701 ) ;
#18410 = CARTESIAN_POINT ( 'NONE',  ( -35.50000000000000711, -113.3474311500483935, -1.624782352598427959 ) ) ;
#18411 = CARTESIAN_POINT ( 'NONE',  ( 0.000000000000000000, 0.000000000000000000, -55.00000000000000000 ) ) ;
#18412 = VECTOR ( 'NONE', #22740, 999.9999999999998863 ) ;
#18413 = AXIS2_PLACEMENT_3D ( 'NONE', #34775, #10097, #27032 ) ;
#18414 = CARTESIAN_POINT ( 'NONE',  ( -35.50000000000000711, -114.1414532730574507, 9.517316564499758158 ) ) ;
#18415 = DIRECTION ( 'NONE',  ( 0.000000000000000000, -0.3090169943749547787, 0.9510565162951513107 ) ) ;
#18416 = ORIENTED_EDGE ( 'NONE', *, *, #34167, .F. ) ;
#18417 = DIRECTION ( 'NONE',  ( -1.000000000000000000, 0.000000000000000000, 0.000000000000000000 ) ) ;
#18418 = CARTESIAN_POINT ( 'NONE',  ( -35.50000000000000000, -112.9650106922503170, -2.624765990393421955 ) ) ;
#18419 = CYLINDRICAL_SURFACE ( 'NONE', #25516, 8.000000000000000000 ) ;
#18420 = ORIENTED_EDGE ( 'NONE', *, *, #12958, .T. ) ;
#18421 = EDGE_LOOP ( 'NONE', ( #19448, #1202, #28938, #21985 ) ) ;
#18422 = CARTESIAN_POINT ( 'NONE',  ( -38.97545270896704039, -113.1123104723225197, 3.847274454178449599 ) ) ;
#18423 = DIRECTION ( 'NONE',  ( 0.000000000000000000, 0.000000000000000000, -1.000000000000000000 ) ) ;
#18424 = ORIENTED_EDGE ( 'NONE', *, *, #9420, .T. ) ;
#18425 = ORIENTED_EDGE ( 'NONE', *, *, #27515, .F. ) ;
#18426 = CARTESIAN_POINT ( 'NONE',  ( -34.50000000000000000, -114.8474311500471572, -0.6247823525984269599 ) ) ;
#18427 = AXIS2_PLACEMENT_3D ( 'NONE', #6967, #2134, #17764 ) ;
#18428 = DIRECTION ( 'NONE',  ( 0.000000000000000000, 0.000000000000000000, 1.000000000000000000 ) ) ;
#18429 = CARTESIAN_POINT ( 'NONE',  ( -42.49999999999999289, -18.77980021920990694, 100.4724318643354053 ) ) ;
#18430 = CIRCLE ( 'NONE', #2937, 4.800000000000000711 ) ;
#18431 = ADVANCED_FACE ( 'NONE', ( #35160 ), #30277, .F. ) ;
#18432 = CARTESIAN_POINT ( 'NONE',  ( -38.00000000000000711, -114.9929510916434339, 12.59102132592608925 ) ) ;
#18433 = DIRECTION ( 'NONE',  ( 0.000000000000000000, 0.000000000000000000, -1.000000000000000000 ) ) ;
#18434 = VECTOR ( 'NONE', #31031, 1000.000000000000000 ) ;
#18435 = AXIS2_PLACEMENT_3D ( 'NONE', #35151, #32257, #12993 ) ;
#18436 = CARTESIAN_POINT ( 'NONE',  ( -34.50000000000000000, -112.0140978167138712, 0.8127176474015721519 ) ) ;
#18437 = AXIS2_PLACEMENT_3D ( 'NONE', #34025, #20488, #17615 ) ;
#18438 = CARTESIAN_POINT ( 'NONE',  ( -35.07817881376918479, -114.9929510916434339, 13.81802396319203297 ) ) ;
#18439 = DIRECTION ( 'NONE',  ( 0.000000000000000000, -0.3090169943749545567, 0.9510565162951513107 ) ) ;
#18440 = PRODUCT_DEFINITION_SHAPE ( 'NONE', 'NONE',  #8827 ) ;
#18441 = DIRECTION ( 'NONE',  ( -1.000000000000000000, -0.000000000000000000, 0.000000000000000000 ) ) ;
#18442 = ORIENTED_EDGE ( 'NONE', *, *, #3561, .T. ) ;
#18443 = ADVANCED_FACE ( 'NONE', ( #24166 ), #35334, .T. ) ;
#18444 = CARTESIAN_POINT ( 'NONE',  ( -36.99999999999988631, -115.9929510916434481, 13.11852480586264846 ) ) ;
#18445 = CARTESIAN_POINT ( 'NONE',  ( -35.50000000000000711, -115.0468226098135744, -1.624774171496087716 ) ) ;
#18446 = DIRECTION ( 'NONE',  ( -1.000000000000000000, -0.000000000000000000, -0.000000000000000000 ) ) ;
#18447 = CARTESIAN_POINT ( 'NONE',  ( 0.000000000000000000, 21.63912866391145684, -3.968388925834583247 ) ) ;
#18448 = CYLINDRICAL_SURFACE ( 'NONE', #24016, 4.800000000000000711 ) ;
#18449 = EDGE_LOOP ( 'NONE', ( #29468, #27659, #27952, #35136 ) ) ;
#18450 = CARTESIAN_POINT ( 'NONE',  ( 4.000000000000000000, 7.317194182740155206, 18.61340026142654125 ) ) ;
#18451 = CARTESIAN_POINT ( 'NONE',  ( -46.00000000000000000, 0.000000000000000000, 8.000000000000000000 ) ) ;
#18452 = CARTESIAN_POINT ( 'NONE',  ( 8.000000000000000000, 0.000000000000000000, 0.000000000000000000 ) ) ;
#18453 = CARTESIAN_POINT ( 'NONE',  ( 7.999999999999992895, -47.00885577955408223, -6.806061952192771436 ) ) ;
#18454 = AXIS2_PLACEMENT_3D ( 'NONE', #20453, #12560, #9677 ) ;
#18455 = CARTESIAN_POINT ( 'NONE',  ( -36.25098837183129774, -113.3347980657956242, 7.316024454178450043 ) ) ;
#18456 = CYLINDRICAL_SURFACE ( 'NONE', #32518, 2.447112362156711018 ) ;
#18457 = CYLINDRICAL_SURFACE ( 'NONE', #26899, 1.000000000000000444 ) ;
#18458 = VERTEX_POINT ( 'NONE', #16387 ) ;
#18459 = ORIENTED_EDGE ( 'NONE', *, *, #9904, .F. ) ;
#18460 = CARTESIAN_POINT ( 'NONE',  ( -34.49999999999998579, -37.35511776651544125, 93.29903810567650169 ) ) ;
#18461 = CYLINDRICAL_SURFACE ( 'NONE', #261, 7.000000000000006217 ) ;
#18462 = ORIENTED_EDGE ( 'NONE', *, *, #27573, .F. ) ;
#18463 = CARTESIAN_POINT ( 'NONE',  ( -38.99999999999999289, -114.0592624029313242, 9.246475545821551734 ) ) ;
#18464 = EDGE_LOOP ( 'NONE', ( #24634, #19111, #24198, #25035 ) ) ;
#18465 = AXIS2_PLACEMENT_3D ( 'NONE', #8838, #17115, #28121 ) ;
#18466 = PRESENTATION_LAYER_ASSIGNMENT (  '', '', ( #10435 ) ) ;
#18467 = AXIS2_PLACEMENT_3D ( 'NONE', #11171, #19951, #706 ) ;
#18468 = EDGE_CURVE ( 'NONE', #27933, #22358, #8116, .T. ) ;
#18469 = CARTESIAN_POINT ( 'NONE',  ( 55.00000000000000000, 20.00000000000001776, 110.0000000000000000 ) ) ;
#18470 = ORIENTED_EDGE ( 'NONE', *, *, #32128, .F. ) ;
#18471 = VERTEX_POINT ( 'NONE', #2569 ) ;
#18472 = CARTESIAN_POINT ( 'NONE',  ( 4.000000000000003553, 9.508666619816942500, -19.83898331853677632 ) ) ;
#18473 = CARTESIAN_POINT ( 'NONE',  ( 4.000000000000000000, 4.898587196589412829E-16, 65.00000000000000000 ) ) ;
#18474 = ORIENTED_EDGE ( 'NONE', *, *, #23274, .T. ) ;
#18475 = VERTEX_POINT ( 'NONE', #21442 ) ;
#18476 = EDGE_CURVE ( 'NONE', #12864, #26214, #35016, .T. ) ;
#18477 = PLANE ( 'NONE',  #27169 ) ;
#18478 = DIRECTION ( 'NONE',  ( -1.000000000000000000, 0.000000000000000000, 0.000000000000000000 ) ) ;
#18479 = EDGE_CURVE ( 'NONE', #27299, #11684, #22900, .T. ) ;
#18480 = EDGE_CURVE ( 'NONE', #33000, #29366, #32796, .T. ) ;
#18481 = ORIENTED_EDGE ( 'NONE', *, *, #4182, .T. ) ;
#18482 = LINE ( 'NONE', #15761, #12503 ) ;
#18483 = CARTESIAN_POINT ( 'NONE',  ( 8.000000000000000000, 0.5097555531875970214, -19.99350267651952606 ) ) ;
#18484 = DIRECTION ( 'NONE',  ( -1.000000000000000000, 0.000000000000000000, 0.000000000000000000 ) ) ;
#18485 = DIRECTION ( 'NONE',  ( 1.000000000000000000, -5.339440136655842133E-16, -1.047965281155519420E-16 ) ) ;
#18486 = CARTESIAN_POINT ( 'NONE',  ( -35.62769128460905677, -115.4561184093552413, 3.191024454178449155 ) ) ;
#18487 = EDGE_CURVE ( 'NONE', #24111, #13301, #10870, .T. ) ;
#18488 = CIRCLE ( 'NONE', #30019, 3.999999999999994227 ) ;
#18489 = CARTESIAN_POINT ( 'NONE',  ( -34.50000000000000000, -115.9929510916434481, 10.53376102667243508 ) ) ;
#18490 = DIRECTION ( 'NONE',  ( -1.000000000000000000, 0.000000000000000000, 0.000000000000000000 ) ) ;
#18491 = EDGE_CURVE ( 'NONE', #21764, #14072, #30097, .T. ) ;
#18492 = CYLINDRICAL_SURFACE ( 'NONE', #29377, 20.00000000000000355 ) ;
#18493 = CARTESIAN_POINT ( 'NONE',  ( 8.000000000000007105, -9.604183132802424083, 5.908880290975512928 ) ) ;
#18494 = FACE_OUTER_BOUND ( 'NONE', #5125, .T. ) ;
#18495 = LINE ( 'NONE', #1952, #10139 ) ;
#18496 = CARTESIAN_POINT ( 'NONE',  ( 0.000000000000000000, 30.03615769709793426, -42.44795908868959344 ) ) ;
#18497 = VERTEX_POINT ( 'NONE', #16577 ) ;
#18498 = CARTESIAN_POINT ( 'NONE',  ( -35.54388159064475872, -115.3723087153909432, 5.683975545821551734 ) ) ;
#18499 = DIRECTION ( 'NONE',  ( 0.000000000000000000, 0.000000000000000000, -1.000000000000000000 ) ) ;
#18500 = DIRECTION ( 'NONE',  ( 0.000000000000000000, 0.000000000000000000, 1.000000000000000000 ) ) ;
#18501 = ORIENTED_EDGE ( 'NONE', *, *, #8882, .F. ) ;
#18502 = ORIENTED_EDGE ( 'NONE', *, *, #8430, .F. ) ;
#18503 = CARTESIAN_POINT ( 'NONE',  ( 0.000000000000000000, -2.710505431213761085E-17, 45.89999999999999858 ) ) ;
#18504 = DIRECTION ( 'NONE',  ( -1.000000000000000000, -0.000000000000000000, 0.000000000000000000 ) ) ;
#18505 = ORIENTED_EDGE ( 'NONE', *, *, #35480, .F. ) ;
#18506 = VERTEX_POINT ( 'NONE', #5435 ) ;
#18507 = VERTEX_POINT ( 'NONE', #5615 ) ;
#18508 = EDGE_CURVE ( 'NONE', #4978, #4101, #10840, .T. ) ;
#18509 = DIRECTION ( 'NONE',  ( 0.000000000000000000, -0.9510565162951565288, 0.3090169943749382919 ) ) ;
#18510 = FACE_OUTER_BOUND ( 'NONE', #15871, .T. ) ;
#18511 = CIRCLE ( 'NONE', #3011, 9.499000000000004107 ) ;
#18512 = STYLED_ITEM ( 'NONE', ( #30781 ), #39 ) ;
#18513 = AXIS2_PLACEMENT_3D ( 'NONE', #27491, #2833, #33058 ) ;
#18514 = DIRECTION ( 'NONE',  ( 0.000000000000000000, 0.000000000000000000, 1.000000000000000000 ) ) ;
#18515 = DIRECTION ( 'NONE',  ( 0.000000000000000000, 0.000000000000000000, 1.000000000000000000 ) ) ;
#18516 = EDGE_LOOP ( 'NONE', ( #4309, #32409 ) ) ;
#18517 = ORIENTED_EDGE ( 'NONE', *, *, #27868, .F. ) ;
#18518 = CARTESIAN_POINT ( 'NONE',  ( -35.50000000000000711, -112.0140978167138712, -0.3122823525984337878 ) ) ;
#18519 = EDGE_CURVE ( 'NONE', #14609, #13647, #20029, .T. ) ;
#18520 = DIRECTION ( 'NONE',  ( -1.047965281155515106E-16, 6.938893903907203726E-17, 1.000000000000000000 ) ) ;
#18521 = EDGE_CURVE ( 'NONE', #17673, #35062, #11010, .T. ) ;
#18522 = EDGE_CURVE ( 'NONE', #20307, #29572, #13721, .T. ) ;
#18523 = CARTESIAN_POINT ( 'NONE',  ( 0.000000000000000000, -0.6505223195686569149, 51.99593080916758936 ) ) ;
#18524 = ORIENTED_EDGE ( 'NONE', *, *, #22916, .F. ) ;
#18525 = DIRECTION ( 'NONE',  ( -1.000000000000000000, 0.000000000000000000, 0.000000000000000000 ) ) ;
#18526 = CARTESIAN_POINT ( 'NONE',  ( -34.50000000000000000, -112.9185811467682754, 1.870920967077121411 ) ) ;
#18527 = CARTESIAN_POINT ( 'NONE',  ( -34.50000306791346816, -114.9929510916434339, 12.62875129555796150 ) ) ;
#18528 = DIRECTION ( 'NONE',  ( 0.000000000000000000, 0.000000000000000000, -1.000000000000000000 ) ) ;
#18529 = CARTESIAN_POINT ( 'NONE',  ( -37.49414064056234253, -114.9929510916434339, 13.11852578240983291 ) ) ;
#18530 = CARTESIAN_POINT ( 'NONE',  ( 3.799999999999999822, -2.710505431213761085E-17, -20.99999999999999645 ) ) ;
#18531 = CARTESIAN_POINT ( 'NONE',  ( -34.50000000000000000, -114.1189822439768449, 9.514224058074130852 ) ) ;
#18532 = CARTESIAN_POINT ( 'NONE',  ( 8.000000000000000000, 3.384281271887823461, 18.48663108841358138 ) ) ;
#18533 = ADVANCED_FACE ( 'NONE', ( #18575 ), #4911, .T. ) ;
#18534 = CARTESIAN_POINT ( 'NONE',  ( -38.00000000000000711, -114.9929510916434339, 12.39849696637031151 ) ) ;
#18535 = DIRECTION ( 'NONE',  ( 0.000000000000000000, 0.000000000000000000, 1.000000000000000000 ) ) ;
#18536 = EDGE_LOOP ( 'NONE', ( #19585, #20266, #1412, #22751 ) ) ;
#18537 = DIRECTION ( 'NONE',  ( 0.000000000000000000, 0.000000000000000000, -1.000000000000000000 ) ) ;
#18538 = LINE ( 'NONE', #13503, #20336 ) ;
#18539 = VERTEX_POINT ( 'NONE', #24869 ) ;
#18540 = VECTOR ( 'NONE', #2570, 1000.000000000000000 ) ;
#18541 = CARTESIAN_POINT ( 'NONE',  ( -36.03125000000004263, -114.9929510916434339, 13.11852480586264669 ) ) ;
#18542 = ORIENTED_EDGE ( 'NONE', *, *, #35040, .F. ) ;
#18543 = CIRCLE ( 'NONE', #22007, 13.99999999999999645 ) ;
#18544 = AXIS2_PLACEMENT_3D ( 'NONE', #27262, #5306, #3442 ) ;
#18545 = CARTESIAN_POINT ( 'NONE',  ( -38.45611840935523418, -115.3723087153909432, 8.066024454178448266 ) ) ;
#18546 = CARTESIAN_POINT ( 'NONE',  ( 112.0000000000000000, 81.48267994499606459, 25.65054357219660019 ) ) ;
#18547 = VERTEX_POINT ( 'NONE', #28102 ) ;
#18548 = ORIENTED_EDGE ( 'NONE', *, *, #21925, .T. ) ;
#18549 = CARTESIAN_POINT ( 'NONE',  ( 8.000000000000000000, 16.31134495048485178, 6.336799421339877725 ) ) ;
#18550 = ORIENTED_EDGE ( 'NONE', *, *, #10455, .F. ) ;
#18551 = CARTESIAN_POINT ( 'NONE',  ( -35.00000000000000000, -114.0592624029313242, 7.503524454178449155 ) ) ;
#18552 = ADVANCED_FACE ( 'NONE', ( #30619 ), #8479, .T. ) ;
#18553 = VECTOR ( 'NONE', #8129, 1000.000000000000000 ) ;
#18554 = AXIS2_PLACEMENT_3D ( 'NONE', #20056, #22948, #20229 ) ;
#18555 = ADVANCED_FACE ( 'NONE', ( #33322, #8817 ), #19779, .F. ) ;
#18556 = CARTESIAN_POINT ( 'NONE',  ( 65.00000000000001421, -35.39471919948800149, 89.19850115919967948 ) ) ;
#18557 = DIRECTION ( 'NONE',  ( 0.000000000000000000, -0.8090169943749405679, -0.5877852522924827960 ) ) ;
#18558 = ORIENTED_EDGE ( 'NONE', *, *, #22857, .T. ) ;
#18560 = ORIENTED_EDGE ( 'NONE', *, *, #21550, .F. ) ;
#18559 = EDGE_CURVE ( 'NONE', #3119, #403, #27482, .T. ) ;
#18561 = CARTESIAN_POINT ( 'NONE',  ( 8.000000000000007105, -9.604183132802312173, -5.908880290975638161 ) ) ;
#18562 = CARTESIAN_POINT ( 'NONE',  ( 8.000000000000000000, -2.912696353505664248, -21.80633394113455736 ) ) ;
#18563 = EDGE_LOOP ( 'NONE', ( #34569, #32081, #32790, #3426 ) ) ;
#18564 = ORIENTED_EDGE ( 'NONE', *, *, #22499, .T. ) ;
#18565 = CARTESIAN_POINT ( 'NONE',  ( -34.50000000000000000, -111.0141129414446652, 0.9205922128478062350 ) ) ;
#18566 = CIRCLE ( 'NONE', #12243, 7.199999999999993072 ) ;
#18567 = CIRCLE ( 'NONE', #20262, 11.00000000000000000 ) ;
#18568 = EDGE_CURVE ( 'NONE', #25018, #892, #17451, .T. ) ;
#18569 = DIRECTION ( 'NONE',  ( 0.000000000000000000, -1.000000000000000000, 0.000000000000000000 ) ) ;
#18570 = VECTOR ( 'NONE', #4055, 1000.000000000000000 ) ;
#18571 = ORIENTED_EDGE ( 'NONE', *, *, #4841, .T. ) ;
#18572 = EDGE_CURVE ( 'NONE', #1656, #440, #33858, .T. ) ;
#18573 = CARTESIAN_POINT ( 'NONE',  ( -35.50000000000000711, -114.9902084924877954, 10.43071793783961176 ) ) ;
#18574 = CARTESIAN_POINT ( 'NONE',  ( -34.50000000000000000, -113.9929510916434339, 10.51725893871049067 ) ) ;
#18575 = FACE_OUTER_BOUND ( 'NONE', #27779, .T. ) ;
#18576 = CARTESIAN_POINT ( 'NONE',  ( -4.000000000000000000, -2.710505431213761085E-17, -45.10000000000000142 ) ) ;
#18577 = CARTESIAN_POINT ( 'NONE',  ( -38.00000000000000711, -113.9929510916434339, 12.60752341388803721 ) ) ;
#18578 = CARTESIAN_POINT ( 'NONE',  ( -35.96730626674924025, -115.9929510916434481, 13.11752178341330222 ) ) ;
#18579 = CARTESIAN_POINT ( 'NONE',  ( 8.000000000000000000, 5.482169781019050170, -16.00140663693117560 ) ) ;
#18580 = AXIS2_PLACEMENT_3D ( 'NONE', #10959, #22104, #33100 ) ;
#18581 = CARTESIAN_POINT ( 'NONE',  ( 0.000000000000000000, -6.336799421339700977, -16.31134495048491573 ) ) ;
#18582 = AXIS2_PLACEMENT_3D ( 'NONE', #17509, #33550, #16801 ) ;
#18583 = ORIENTED_EDGE ( 'NONE', *, *, #32353, .T. ) ;
#18584 = CARTESIAN_POINT ( 'NONE',  ( 1.599999999999990319, 0.000000000000000000, 0.000000000000000000 ) ) ;
#18585 = DIRECTION ( 'NONE',  ( 0.000000000000000000, -0.9510565162951564178, 0.3090169943749385140 ) ) ;
#18586 = CARTESIAN_POINT ( 'NONE',  ( -4.000000000000000000, 0.000000000000000000, 65.00000000000000000 ) ) ;
#18587 = ORIENTED_EDGE ( 'NONE', *, *, #6035, .T. ) ;
#18588 = CARTESIAN_POINT ( 'NONE',  ( 7.999999999999992895, -47.49120266317495975, -0.8606222198180163430 ) ) ;
#18589 = AXIS2_PLACEMENT_3D ( 'NONE', #3279, #14238, #30290 ) ;
#18590 = CIRCLE ( 'NONE', #7662, 5.000000000000004441 ) ;
#18591 = CARTESIAN_POINT ( 'NONE',  ( -35.50000000000000711, -112.1403507321855528, -1.128496220798856253 ) ) ;
#18592 = DIRECTION ( 'NONE',  ( -1.000000000000000000, -1.734723475976807094E-16, -0.000000000000000000 ) ) ;
#18593 = CARTESIAN_POINT ( 'NONE',  ( -35.50000000000000711, -114.9929510916434339, 10.59426868253284226 ) ) ;
#18594 = CARTESIAN_POINT ( 'NONE',  ( 8.000000000000007105, -3.753907720748892007, -8.725776631572756514 ) ) ;
#18595 = EDGE_CURVE ( 'NONE', #9753, #25616, #5954, .T. ) ;
#18596 = VERTEX_POINT ( 'NONE', #3796 ) ;
#18597 = ADVANCED_FACE ( 'NONE', ( #22329 ), #33150, .F. ) ;
#18598 = CARTESIAN_POINT ( 'NONE',  ( -3.799999999999999822, 4.653657836759942730E-16, -55.89999999999999858 ) ) ;
#18599 = CARTESIAN_POINT ( 'NONE',  ( -35.50000000000000000, -111.0397324434303101, -0.9506101647064429949 ) ) ;
#18600 = ORIENTED_EDGE ( 'NONE', *, *, #15368, .T. ) ;
#18601 = ORIENTED_EDGE ( 'NONE', *, *, #4997, .T. ) ;
#18602 = CARTESIAN_POINT ( 'NONE',  ( -35.62769128460905677, -115.4561184093552413, 1.691024454178448710 ) ) ;
#18603 =( NAMED_UNIT ( * ) SI_UNIT ( $, .STERADIAN. ) SOLID_ANGLE_UNIT ( ) );
#18604 = FACE_OUTER_BOUND ( 'NONE', #7575, .T. ) ;
#18606 = VERTEX_POINT ( 'NONE', #16912 ) ;
#18605 = AXIS2_PLACEMENT_3D ( 'NONE', #4479, #23355, #21186 ) ;
#18607 = EDGE_LOOP ( 'NONE', ( #9188, #29246, #21789, #1008 ) ) ;
#18608 = CARTESIAN_POINT ( 'NONE',  ( -34.50000000000000000, -113.0140978167136581, 0.8752176474015690433 ) ) ;
#18609 = CIRCLE ( 'NONE', #26673, 9.499000000000012989 ) ;
#18610 = CARTESIAN_POINT ( 'NONE',  ( 0.000000000000000000, -13.42368113696669418, 3.975523202427999614 ) ) ;
#18611 = LINE ( 'NONE', #12689, #5896 ) ;
#18612 = CIRCLE ( 'NONE', #11141, 19.99999999999998579 ) ;
#18613 = CARTESIAN_POINT ( 'NONE',  ( -37.46874999999996447, -114.9929510916434339, 13.11852480586264669 ) ) ;
#18614 = VECTOR ( 'NONE', #17724, 1000.000000000000000 ) ;
#18615 = DIRECTION ( 'NONE',  ( -1.000000000000000000, 0.000000000000000000, 0.000000000000000000 ) ) ;
#18616 = DIRECTION ( 'NONE',  ( -1.000000000000000000, 0.000000000000000000, 0.000000000000000000 ) ) ;
#18617 = CARTESIAN_POINT ( 'NONE',  ( -34.50000000000000000, -112.0651520602111191, -0.9469505670458575608 ) ) ;
#18618 = CARTESIAN_POINT ( 'NONE',  ( 8.000000000000007105, 0.000000000000000000, 0.000000000000000000 ) ) ;
#18619 = AXIS2_PLACEMENT_3D ( 'NONE', #8754, #3207, #28047 ) ;
#18620 = DIRECTION ( 'NONE',  ( -1.000000000000000000, 0.000000000000000000, 0.000000000000000000 ) ) ;
#18621 = ORIENTED_EDGE ( 'NONE', *, *, #31686, .F. ) ;
#18622 = CARTESIAN_POINT ( 'NONE',  ( -37.46093750000000711, -115.9929510916434481, 13.11852480586264846 ) ) ;
#18623 = CARTESIAN_POINT ( 'NONE',  ( -34.49999999999998579, -25.98076211353320986, 84.99999999999994316 ) ) ;
#18624 =( NAMED_UNIT ( * ) PLANE_ANGLE_UNIT ( ) SI_UNIT ( $, .RADIAN. ) );
#18625 = CARTESIAN_POINT ( 'NONE',  ( 0.000000000000000000, 0.000000000000000000, -55.89999999999999858 ) ) ;
#18626 = CARTESIAN_POINT ( 'NONE',  ( 7.999999999999992895, -29.60891106212813995, 37.14118181634756866 ) ) ;
#18627 = ORIENTED_EDGE ( 'NONE', *, *, #20257, .F. ) ;
#18628 = CYLINDRICAL_SURFACE ( 'NONE', #7624, 52.00000000000000711 ) ;
#18629 = CARTESIAN_POINT ( 'NONE',  ( 7.999999999999992895, 0.000000000000000000, 0.000000000000000000 ) ) ;
#18630 = CARTESIAN_POINT ( 'NONE',  ( 4.000000000000000000, 4.898587196589412829E-16, 45.00000000000000711 ) ) ;
#18631 = DIRECTION ( 'NONE',  ( -1.000000000000000000, 0.000000000000000000, 0.000000000000000000 ) ) ;
#18632 = DIRECTION ( 'NONE',  ( -1.000000000000000000, -1.734723475976807094E-16, -0.000000000000000000 ) ) ;
#18633 = DIRECTION ( 'NONE',  ( 1.000000000000000000, 0.000000000000000000, 0.000000000000000000 ) ) ;
#18634 = ORIENTED_EDGE ( 'NONE', *, *, #26417, .T. ) ;
#18635 = ORIENTED_EDGE ( 'NONE', *, *, #3294, .T. ) ;
#18636 =( REPRESENTATION_RELATIONSHIP ('NONE','NONE', #26607, #4547 ) REPRESENTATION_RELATIONSHIP_WITH_TRANSFORMATION ( #30344 )SHAPE_REPRESENTATION_RELATIONSHIP( ) );
#18637 = CIRCLE ( 'NONE', #19764, 9.499000000000007660 ) ;
#18638 = ADVANCED_FACE ( 'NONE', ( #25226 ), #30792, .T. ) ;
#18639 = FACE_OUTER_BOUND ( 'NONE', #7255, .T. ) ;
#18640 = LINE ( 'NONE', #24768, #26453 ) ;
#18641 = DIRECTION ( 'NONE',  ( 1.000000000000000000, -0.000000000000000000, -0.000000000000000000 ) ) ;
#18642 = EDGE_LOOP ( 'NONE', ( #4652, #18470 ) ) ;
#18643 = CARTESIAN_POINT ( 'NONE',  ( -35.02454729103298803, -113.1123104723225197, 5.402725545821551734 ) ) ;
#18644 = ORIENTED_EDGE ( 'NONE', *, *, #17988, .T. ) ;
#18645 =( NAMED_UNIT ( * ) PLANE_ANGLE_UNIT ( ) SI_UNIT ( $, .RADIAN. ) );
#18646 = EDGE_LOOP ( 'NONE', ( #30992, #20629, #13256, #31970 ) ) ;
#18647 = ORIENTED_EDGE ( 'NONE', *, *, #23353, .T. ) ;
#18648 = CARTESIAN_POINT ( 'NONE',  ( 0.000000000000000000, 0.000000000000000000, -33.50000000000000711 ) ) ;
#18649 = ADVANCED_FACE ( 'NONE', ( #6132, #719 ), #19963, .T. ) ;
#18650 = DIRECTION ( 'NONE',  ( -1.000000000000000000, 0.000000000000000000, -0.000000000000000000 ) ) ;
#18651 = VERTEX_POINT ( 'NONE', #8648 ) ;
#18652 = VERTEX_POINT ( 'NONE', #17095 ) ;
#18653 = DIRECTION ( 'NONE',  ( 1.000000000000000000, -4.524158825347490025E-15, -1.169797080839617330E-15 ) ) ;
#18654 = CARTESIAN_POINT ( 'NONE',  ( -39.49999999999999289, -3.784235812937200460, 96.08311962715481513 ) ) ;
#18655 = DIRECTION ( 'NONE',  ( -1.000000000000000000, -1.836970198721029934E-16, -0.000000000000000000 ) ) ;
#18656 = DIRECTION ( 'NONE',  ( 0.000000000000000000, -0.8443279255020201823, 0.5358267949789887741 ) ) ;
#18657 = CARTESIAN_POINT ( 'NONE',  ( 8.000000000000000000, 0.000000000000000000, 0.000000000000000000 ) ) ;
#18658 = CIRCLE ( 'NONE', #24993, 7.000000000000006217 ) ;
#18659 = DIRECTION ( 'NONE',  ( 1.000000000000000000, 1.836970198721029934E-16, 0.000000000000000000 ) ) ;
#18660 = CARTESIAN_POINT ( 'NONE',  ( -36.94073759706868287, -112.0000000000000142, 5.628524454178449155 ) ) ;
#18661 = CARTESIAN_POINT ( 'NONE',  ( -34.50000000000000000, -115.9927366631908825, 10.47601115720670073 ) ) ;
#18662 = FACE_OUTER_BOUND ( 'NONE', #8452, .T. ) ;
#18663 = CIRCLE ( 'NONE', #4891, 47.49900000000001654 ) ;
#18664 = CARTESIAN_POINT ( 'NONE',  ( 0.000000000000000000, 0.000000000000000000, 0.000000000000000000 ) ) ;
#18665 = DIRECTION ( 'NONE',  ( 0.000000000000000000, 0.000000000000000000, -1.000000000000000000 ) ) ;
#18666 = DIRECTION ( 'NONE',  ( -1.000000000000000000, 0.000000000000000000, -0.000000000000000000 ) ) ;
#18667 = DIRECTION ( 'NONE',  ( 0.000000000000000000, 0.000000000000000000, -1.000000000000000000 ) ) ;
#18668 = ORIENTED_EDGE ( 'NONE', *, *, #1665, .T. ) ;
#18669 = CARTESIAN_POINT ( 'NONE',  ( -39.07941549657749647, -116.1632251905417803, 9.058975545821549957 ) ) ;
#18670 = DIRECTION ( 'NONE',  ( -1.000000000000000000, 0.000000000000000000, 0.000000000000000000 ) ) ;
#18671 = LINE ( 'NONE', #2497, #13098 ) ;
#18672 = ORIENTED_EDGE ( 'NONE', *, *, #25604, .F. ) ;
#18673 = AXIS2_PLACEMENT_3D ( 'NONE', #11186, #19621, #35516 ) ;
#18674 = ORIENTED_EDGE ( 'NONE', *, *, #30183, .F. ) ;
#18675 = EDGE_CURVE ( 'NONE', #33313, #5508, #14398, .T. ) ;
#18676 = CYLINDRICAL_SURFACE ( 'NONE', #21672, 4.000000000000000000 ) ;
#18677 = DIRECTION ( 'NONE',  ( 0.000000000000000000, 0.000000000000000000, -1.000000000000000000 ) ) ;
#18678 = ORIENTED_EDGE ( 'NONE', *, *, #35264, .F. ) ;
#18679 = EDGE_CURVE ( 'NONE', #16323, #30634, #3620, .T. ) ;
#18680 = ORIENTED_EDGE ( 'NONE', *, *, #23139, .F. ) ;
#18681 = CLOSED_SHELL ( 'NONE', ( #32588, #24946, #33552, #26659, #22063, #31566, #711, #3347, #1410, #32885, #25772, #10800, #3612, #31463, #9915, #15243, #14564, #31098, #10118, #12592, #29714, #21401, #19748, #32204, #28448, #34395, #35081, #2542, #28119, #25792, #29090, #27123, #7007, #1147, #19182, #23324, #31, #20657, #18443, #2125, #10605, #947, #22213, #2606, #15786, #19556, #15943, #28489, #31507, #10680, #19198, #25285, #10349, #20340, #14436, #9665, #22047, #34747, #20701, #26501, #5344, #2493, #26057, #22408, #11247, #16340, #23183, #217, #8209, #20979, #30045, #35058, #34107, #20461, #15330, #12916, #28299, #34355, #5980, #35448, #24035, #16681, #20443, #16754, #24315 ) ) ;
#18682 = CARTESIAN_POINT ( 'NONE',  ( -21.15833593587365513, -27.48076211353326670, 88.99999999999994316 ) ) ;
#18683 = AXIS2_PLACEMENT_3D ( 'NONE', #8736, #11111, #27507 ) ;
#18684 = CARTESIAN_POINT ( 'NONE',  ( 7.999999999999992895, 0.000000000000000000, 0.000000000000000000 ) ) ;
#18685 = EDGE_CURVE ( 'NONE', #24050, #18057, #899, .T. ) ;
#18686 = CARTESIAN_POINT ( 'NONE',  ( 45.89999999999999147, -1.734723475976807094E-15, 69.99999999999998579 ) ) ;
#18687 = ADVANCED_FACE ( 'NONE', ( #8999 ), #1611, .T. ) ;
#18688 = AXIS2_PLACEMENT_3D ( 'NONE', #24975, #11287, #30030 ) ;
#18689 = DIRECTION ( 'NONE',  ( -1.000000000000000000, 0.000000000000000000, 0.000000000000000000 ) ) ;
#18690 = ORIENTED_EDGE ( 'NONE', *, *, #6564, .F. ) ;
#18691 = ORIENTED_EDGE ( 'NONE', *, *, #33966, .F. ) ;
#18692 = CARTESIAN_POINT ( 'NONE',  ( -35.50000000000000711, -112.1222502514821144, 1.343475657184566296 ) ) ;
#18693 = VECTOR ( 'NONE', #20261, 1000.000000000000000 ) ;
#18694 = CARTESIAN_POINT ( 'NONE',  ( -55.00000000000000000, 0.000000000000000000, 0.000000000000000000 ) ) ;
#18695 = CARTESIAN_POINT ( 'NONE',  ( 65.00000000000001421, -25.98076211353320986, 84.99999999999994316 ) ) ;
#18696 = ORIENTED_EDGE ( 'NONE', *, *, #1106, .F. ) ;
#18697 = DIRECTION ( 'NONE',  ( 0.000000000000000000, 0.000000000000000000, 1.000000000000000000 ) ) ;
#18698 = CARTESIAN_POINT ( 'NONE',  ( -34.50000000000000000, -112.7549084230351752, -1.592823285203595285 ) ) ;
#18699 = CARTESIAN_POINT ( 'NONE',  ( -34.50000000000000000, -114.9860996047076895, 10.38555023491505835 ) ) ;
#18700 = DIRECTION ( 'NONE',  ( -1.000000000000000000, 0.000000000000000000, 0.000000000000000000 ) ) ;
#18701 = CARTESIAN_POINT ( 'NONE',  ( -36.12500000000014211, -114.9929510916434339, 13.11852480586264669 ) ) ;
#18702 = CARTESIAN_POINT ( 'NONE',  ( -46.00000000000000000, 0.000000000000000000, 70.00000000000000000 ) ) ;
#18703 = CARTESIAN_POINT ( 'NONE',  ( -39.00000000000000000, -113.9929510916434339, 12.57451923796417681 ) ) ;
#18704 = CARTESIAN_POINT ( 'NONE',  ( 0.000000000000000000, -2.710505431213761085E-17, -21.89999999999999858 ) ) ;
#18705 = ADVANCED_FACE ( 'NONE', ( #14045 ), #11363, .T. ) ;
#18706 = DIRECTION ( 'NONE',  ( -1.000000000000000000, -1.836970198721029934E-16, -0.000000000000000000 ) ) ;
#18707 = FILL_AREA_STYLE_COLOUR ( '', #15905 ) ;
#18708 = EDGE_LOOP ( 'NONE', ( #32336, #29635 ) ) ;
#18709 = DIRECTION ( 'NONE',  ( 0.000000000000000000, 0.000000000000000000, -1.000000000000000000 ) ) ;
#18710 = CARTESIAN_POINT ( 'NONE',  ( -90.00000000000002842, 9.554310223899640008E-16, 4.980000000000024407 ) ) ;
#18711 = AXIS2_PLACEMENT_3D ( 'NONE', #606, #21682, #5323 ) ;
#18712 = ORIENTED_EDGE ( 'NONE', *, *, #28412, .F. ) ;
#18713 = CARTESIAN_POINT ( 'NONE',  ( -37.99994980024369085, -114.9929510916434339, 12.62670525340494621 ) ) ;
#18714 = ORIENTED_EDGE ( 'NONE', *, *, #21547, .F. ) ;
#18715 = CARTESIAN_POINT ( 'NONE',  ( -37.76916472181487450, -111.9754527089670404, 7.034774454178450931 ) ) ;
#18716 = DIRECTION ( 'NONE',  ( 1.282131172192753642E-16, -6.938893903907203726E-17, -1.000000000000000000 ) ) ;
#18717 = ORIENTED_EDGE ( 'NONE', *, *, #13220, .F. ) ;
#18718 = VERTEX_POINT ( 'NONE', #9360 ) ;
#18719 = EDGE_CURVE ( 'NONE', #1616, #8203, #22310, .T. ) ;
#18720 = CARTESIAN_POINT ( 'NONE',  ( 0.000000000000000000, -22.82995208772716467, 41.06517797613655318 ) ) ;
#18721 = CARTESIAN_POINT ( 'NONE',  ( 8.000000000000007105, 0.000000000000000000, 0.000000000000000000 ) ) ;
#18722 = ADVANCED_FACE ( 'NONE', ( #31676 ), #9540, .T. ) ;
#18723 = EDGE_CURVE ( 'NONE', #1299, #6291, #1090, .T. ) ;
#18724 = ORIENTED_EDGE ( 'NONE', *, *, #12555, .F. ) ;
#18725 = CARTESIAN_POINT ( 'NONE',  ( -39.16322519054179452, -116.0794154965774823, 3.566024454178448710 ) ) ;
#18726 = CIRCLE ( 'NONE', #3220, 52.00000000000000711 ) ;
#18727 = CARTESIAN_POINT ( 'NONE',  ( 44.00000000000000000, 11.00000000000001066, 1.347111479062088010E-15 ) ) ;
#18728 = CARTESIAN_POINT ( 'NONE',  ( 8.000000000000000000, -19.35373470438975119, -10.46102064772362183 ) ) ;
#18729 = ORIENTED_EDGE ( 'NONE', *, *, #16312, .F. ) ;
#18730 = EDGE_LOOP ( 'NONE', ( #2751, #25555 ) ) ;
#18731 = DIRECTION ( 'NONE',  ( -1.000000000000000000, 0.000000000000000000, -0.000000000000000000 ) ) ;
#18732 = EDGE_CURVE ( 'NONE', #12018, #35000, #25209, .T. ) ;
#18733 = EDGE_CURVE ( 'NONE', #33477, #11373, #35552, .T. ) ;
#18734 = CARTESIAN_POINT ( 'NONE',  ( 7.999999999999992895, 44.25018368420782622, -27.31155879685134735 ) ) ;
#18735 = VERTEX_POINT ( 'NONE', #17985 ) ;
#18736 = EDGE_LOOP ( 'NONE', ( #35182, #17252, #14348, #3690 ) ) ;
#18737 = CARTESIAN_POINT ( 'NONE',  ( -34.50000000000000000, -112.6572589393539516, 2.844055607295835397 ) ) ;
#18738 = AXIS2_PLACEMENT_3D ( 'NONE', #5110, #7600, #29589 ) ;
#18739 = DIRECTION ( 'NONE',  ( 0.000000000000000000, 0.9510565162951544194, -0.3090169943749448977 ) ) ;
#18740 = EDGE_LOOP ( 'NONE', ( #3602, #25781, #4944, #25426 ) ) ;
#18741 = CARTESIAN_POINT ( 'NONE',  ( -35.50000000000000711, -114.2598117360253696, 9.542047897280109936 ) ) ;
#18742 = CIRCLE ( 'NONE', #7793, 17.49900000000000233 ) ;
#18743 = AXIS2_PLACEMENT_3D ( 'NONE', #5752, #33460, #3061 ) ;
#18744 = CARTESIAN_POINT ( 'NONE',  ( -34.50000000000000000, -113.9929510916434339, 10.55026311463432087 ) ) ;
#18745 = DIRECTION ( 'NONE',  ( -1.000000000000000000, 0.000000000000000000, 0.000000000000000000 ) ) ;
#18746 = LINE ( 'NONE', #26699, #21413 ) ;
#18747 = CARTESIAN_POINT ( 'NONE',  ( -38.00000000000000711, -113.9929510916434339, 12.59102132592609102 ) ) ;
#18748 = AXIS2_PLACEMENT_3D ( 'NONE', #6907, #4227, #12679 ) ;
#18749 = ADVANCED_FACE ( 'NONE', ( #34401 ), #12419, .T. ) ;
#18750 = CARTESIAN_POINT ( 'NONE',  ( -36.50000000000010658, -115.9929510916434481, 13.11852480586264846 ) ) ;
#18751 = AXIS2_PLACEMENT_3D ( 'NONE', #10406, #9686, #4664 ) ;
#18752 = CARTESIAN_POINT ( 'NONE',  ( -49.99999999999998579, -60.00000000000000000, 120.0000000000000000 ) ) ;
#18753 = DIRECTION ( 'NONE',  ( -1.000000000000000000, 0.000000000000000000, 0.000000000000000000 ) ) ;
#18754 = EDGE_CURVE ( 'NONE', #26302, #26408, #1808, .T. ) ;
#18755 = VERTEX_POINT ( 'NONE', #25937 ) ;
#18756 = EDGE_CURVE ( 'NONE', #32280, #4250, #28650, .T. ) ;
#18757 = DIRECTION ( 'NONE',  ( 0.000000000000000000, 0.000000000000000000, 1.000000000000000000 ) ) ;
#18758 = PLANE ( 'NONE',  #5905 ) ;
#18759 = CARTESIAN_POINT ( 'NONE',  ( 0.000000000000000000, 51.93417535146742381, -2.615612846549375536 ) ) ;
#18760 = AXIS2_PLACEMENT_3D ( 'NONE', #723, #34405, #23222 ) ;
#18761 = ORIENTED_EDGE ( 'NONE', *, *, #3107, .T. ) ;
#18762 = DIRECTION ( 'NONE',  ( -1.000000000000000000, 0.000000000000000000, 0.000000000000000000 ) ) ;
#18763 = AXIS2_PLACEMENT_3D ( 'NONE', #9558, #28467, #3814 ) ;
#18764 = CARTESIAN_POINT ( 'NONE',  ( -35.50000000000000711, -116.0012805033554883, -0.7876962586524312027 ) ) ;
#18765 = CARTESIAN_POINT ( 'NONE',  ( 7.999999999999992895, 27.43636312076321104, 38.14186064215159888 ) ) ;
#18766 = ADVANCED_FACE ( 'NONE', ( #26291, #6654 ), #20678, .T. ) ;
#18767 = EDGE_CURVE ( 'NONE', #34183, #29017, #28058, .T. ) ;
#18768 = CARTESIAN_POINT ( 'NONE',  ( -35.50000000000000711, -114.9929517792218689, 10.50900788599415314 ) ) ;
#18769 = DIRECTION ( 'NONE',  ( 0.000000000000000000, -6.938893903907202493E-17, -1.000000000000000000 ) ) ;
#18770 = VECTOR ( 'NONE', #28776, 1000.000000000000000 ) ;
#18771 = VERTEX_POINT ( 'NONE', #23580 ) ;
#18772 = AXIS2_PLACEMENT_3D ( 'NONE', #29048, #25996, #9608 ) ;
#18773 = CARTESIAN_POINT ( 'NONE',  ( -35.50000000000000000, -112.9611193698460738, 2.883091707513499635 ) ) ;
#18774 = ORIENTED_EDGE ( 'NONE', *, *, #13960, .T. ) ;
#18775 = ORIENTED_EDGE ( 'NONE', *, *, #10968, .F. ) ;
#18776 = AXIS2_PLACEMENT_3D ( 'NONE', #13455, #24437, #35422 ) ;
#18777 = CARTESIAN_POINT ( 'NONE',  ( -38.99999999999999289, -113.9407375970686900, 2.253524454178449155 ) ) ;
#18778 = AXIS2_PLACEMENT_3D ( 'NONE', #29596, #2058, #32287 ) ;
#18779 = ADVANCED_FACE ( 'NONE', ( #17633 ), #29352, .T. ) ;
#18780 = CIRCLE ( 'NONE', #25708, 4.725000000000016520 ) ;
#18781 = CARTESIAN_POINT ( 'NONE',  ( -9.999999999999994671, 0.000000000000000000, 0.000000000000000000 ) ) ;
#18782 = ORIENTED_EDGE ( 'NONE', *, *, #33629, .F. ) ;
#18783 = ORIENTED_EDGE ( 'NONE', *, *, #30564, .F. ) ;
#18784 = CARTESIAN_POINT ( 'NONE',  ( -34.50000000000000000, -113.0140978167138712, 0.0002176474015659786963 ) ) ;
#18785 = CARTESIAN_POINT ( 'NONE',  ( 8.000000000000000000, 0.000000000000000000, 0.000000000000000000 ) ) ;
#18786 = DIRECTION ( 'NONE',  ( 0.000000000000000000, 0.000000000000000000, 1.000000000000000000 ) ) ;
#18787 = VECTOR ( 'NONE', #20774, 1000.000000000000000 ) ;
#18788 = CARTESIAN_POINT ( 'NONE',  ( 0.000000000000000000, 0.000000000000000000, 0.000000000000000000 ) ) ;
#18789 = AXIS2_PLACEMENT_3D ( 'NONE', #30060, #21938, #19229 ) ;
#18790 = AXIS2_PLACEMENT_3D ( 'NONE', #8160, #21663, #10347 ) ;
#18791 = CARTESIAN_POINT ( 'NONE',  ( -38.00000000000000711, -114.9929510916434339, 10.50625754673587231 ) ) ;
#18792 = CARTESIAN_POINT ( 'NONE',  ( 0.000000000000000000, 0.000000000000000000, 0.000000000000000000 ) ) ;
#18793 = LINE ( 'NONE', #32304, #22815 ) ;
#18794 = CARTESIAN_POINT ( 'NONE',  ( -34.50000000000000000, -112.0140978167138712, -0.4685323525984295134 ) ) ;
#18795 = AXIS2_PLACEMENT_3D ( 'NONE', #16844, #27848, #3191 ) ;
#18796 = EDGE_CURVE ( 'NONE', #25838, #9043, #34573, .T. ) ;
#18797 = FACE_OUTER_BOUND ( 'NONE', #15822, .T. ) ;
#18798 = VECTOR ( 'NONE', #19290, 1000.000000000000000 ) ;
#18799 = EDGE_CURVE ( 'NONE', #13248, #19516, #30924, .T. ) ;
#18800 = AXIS2_PLACEMENT_3D ( 'NONE', #29624, #2443, #2277 ) ;
#18801 = DIRECTION ( 'NONE',  ( -1.000000000000000000, 0.000000000000000000, 0.000000000000000000 ) ) ;
#18803 = VERTEX_POINT ( 'NONE', #7380 ) ;
#18802 = CIRCLE ( 'NONE', #25135, 1.000000000000000888 ) ;
#18804 = CARTESIAN_POINT ( 'NONE',  ( -35.50000000000000711, -114.1861579685891712, 9.524983039397698192 ) ) ;
#18805 = DIRECTION ( 'NONE',  ( -1.000000000000000000, 0.000000000000000000, 0.000000000000000000 ) ) ;
#18806 = CARTESIAN_POINT ( 'NONE',  ( 7.999999999999992895, 0.000000000000000000, 0.000000000000000000 ) ) ;
#18807 = LINE ( 'NONE', #13413, #5918 ) ;
#18808 = FACE_OUTER_BOUND ( 'NONE', #25479, .T. ) ;
#18809 = VERTEX_POINT ( 'NONE', #25762 ) ;
#18810 = DIRECTION ( 'NONE',  ( -1.000000000000000000, -1.836970198721029934E-16, -0.000000000000000000 ) ) ;
#18811 = FACE_OUTER_BOUND ( 'NONE', #13211, .T. ) ;
#18812 = CARTESIAN_POINT ( 'NONE',  ( 0.000000000000000000, 0.000000000000000000, 0.000000000000000000 ) ) ;
#18813 = LINE ( 'NONE', #29814, #21855 ) ;
#18814 = LINE ( 'NONE', #13594, #20992 ) ;
#18815 = CARTESIAN_POINT ( 'NONE',  ( 0.000000000000000000, 3.678165988948789877, -15.05623113391063406 ) ) ;
#18816 = ORIENTED_EDGE ( 'NONE', *, *, #7988, .F. ) ;
#18817 = VECTOR ( 'NONE', #18805, 1000.000000000000000 ) ;
#18818 = ORIENTED_EDGE ( 'NONE', *, *, #8362, .T. ) ;
#18819 = CARTESIAN_POINT ( 'NONE',  ( 0.000000000000000000, -3.384281271887680909, -18.48663108841362757 ) ) ;
#18820 = AXIS2_PLACEMENT_3D ( 'NONE', #3096, #369, #22332 ) ;
#18821 = DIRECTION ( 'NONE',  ( 0.000000000000000000, 0.000000000000000000, 1.000000000000000000 ) ) ;
#18822 = DIRECTION ( 'NONE',  ( 0.000000000000000000, 0.000000000000000000, 1.000000000000000000 ) ) ;
#18823 = EDGE_LOOP ( 'NONE', ( #23435, #7133, #2250, #2826 ) ) ;
#18824 = CARTESIAN_POINT ( 'NONE',  ( -35.02454729103298803, -113.1123104723225197, 6.902725545821550845 ) ) ;
#18825 = ORIENTED_EDGE ( 'NONE', *, *, #29068, .F. ) ;
#18826 = CIRCLE ( 'NONE', #3317, 7.020000000000045759 ) ;
#18827 = EDGE_LOOP ( 'NONE', ( #25952, #23391, #4876, #2778 ) ) ;
#18828 = ORIENTED_EDGE ( 'NONE', *, *, #20973, .T. ) ;
#18829 = VECTOR ( 'NONE', #9924, 1000.000000000000000 ) ;
#18830 = DIRECTION ( 'NONE',  ( -1.000000000000000000, 0.000000000000000000, 0.000000000000000000 ) ) ;
#18831 = AXIS2_PLACEMENT_3D ( 'NONE', #6411, #19713, #14328 ) ;
#18832 = CIRCLE ( 'NONE', #17092, 22.00000000000000000 ) ;
#18833 = DIRECTION ( 'NONE',  ( 0.000000000000000000, 0.000000000000000000, -1.000000000000000000 ) ) ;
#18834 = EDGE_LOOP ( 'NONE', ( #11558, #21949, #26519, #18724 ) ) ;
#18835 = EDGE_LOOP ( 'NONE', ( #32120, #7605 ) ) ;
#18836 = CARTESIAN_POINT ( 'NONE',  ( 7.999999999999992895, 0.000000000000000000, 0.000000000000000000 ) ) ;
#18837 = DIRECTION ( 'NONE',  ( -1.000000000000000000, 0.000000000000000000, 0.000000000000000000 ) ) ;
#18838 = CARTESIAN_POINT ( 'NONE',  ( 65.00000000000001421, 46.66021779527611102, 66.80632251401318911 ) ) ;
#18839 = AXIS2_PLACEMENT_3D ( 'NONE', #19837, #8874, #30506 ) ;
#18840 = CARTESIAN_POINT ( 'NONE',  ( 8.000000000000000000, 0.000000000000000000, 0.000000000000000000 ) ) ;
#18841 = CARTESIAN_POINT ( 'NONE',  ( 8.000000000000000000, 13.60411018104320036, 12.96676809804154118 ) ) ;
#18842 = EDGE_CURVE ( 'NONE', #891, #5174, #5653, .T. ) ;
#18843 = AXIS2_PLACEMENT_3D ( 'NONE', #22673, #25584, #9185 ) ;
#18844 = CARTESIAN_POINT ( 'NONE',  ( -37.76916472181487450, -111.9754527089670404, 7.034774454178450043 ) ) ;
#18845 = VECTOR ( 'NONE', #23762, 1000.000000000000000 ) ;
#18846 = CARTESIAN_POINT ( 'NONE',  ( -37.46874999999995737, -115.9929510916434481, 14.11852480586265024 ) ) ;
#18847 = DIRECTION ( 'NONE',  ( 0.000000000000000000, 0.000000000000000000, -1.000000000000000000 ) ) ;
#18848 = AXIS2_PLACEMENT_3D ( 'NONE', #20662, #6821, #15264 ) ;
#18849 = CARTESIAN_POINT ( 'NONE',  ( 8.000000000000000000, -11.11653975335798528, 12.74840161668727134 ) ) ;
#18850 = AXIS2_PLACEMENT_3D ( 'NONE', #7700, #10055, #21022 ) ;
#18851 = DIRECTION ( 'NONE',  ( -0.000000000000000000, 0.000000000000000000, -1.000000000000000000 ) ) ;
#18852 = FACE_OUTER_BOUND ( 'NONE', #9430, .T. ) ;
#18853 = DIRECTION ( 'NONE',  ( -1.000000000000000000, 0.000000000000000000, 0.000000000000000000 ) ) ;
#18854 = ORIENTED_EDGE ( 'NONE', *, *, #17566, .T. ) ;
#18855 = CARTESIAN_POINT ( 'NONE',  ( -34.92058450342249643, -111.8367748094582197, 9.808975545821553510 ) ) ;
#18856 = VECTOR ( 'NONE', #22308, 1000.000000000000000 ) ;
#18857 = DIRECTION ( 'NONE',  ( -1.000000000000000000, 0.000000000000000000, -0.000000000000000000 ) ) ;
#18858 = DIRECTION ( 'NONE',  ( 1.000000000000000000, -5.339440136655823397E-16, 0.000000000000000000 ) ) ;
#18859 = DIRECTION ( 'NONE',  ( 0.000000000000000000, 0.000000000000000000, -1.000000000000000000 ) ) ;
#18860 = ORIENTED_EDGE ( 'NONE', *, *, #5381, .F. ) ;
#18861 = CARTESIAN_POINT ( 'NONE',  ( -34.50000000000000000, -113.0140978167138712, 0.0002176474015659786963 ) ) ;
#18862 = ORIENTED_EDGE ( 'NONE', *, *, #18927, .F. ) ;
#18863 = DIRECTION ( 'NONE',  ( 0.000000000000000000, -0.7705132427757949154, 0.6374239897486827511 ) ) ;
#18864 = CARTESIAN_POINT ( 'NONE',  ( 5.400000000000085620, -1.000000000000049516, -32.00000000000000000 ) ) ;
#18865 = ORIENTED_EDGE ( 'NONE', *, *, #17238, .T. ) ;
#18866 = ORIENTED_EDGE ( 'NONE', *, *, #6321, .T. ) ;
#18867 = CARTESIAN_POINT ( 'NONE',  ( 7.999999999999992895, -11.46872990052412611, 45.56340405422440654 ) ) ;
#18868 = CARTESIAN_POINT ( 'NONE',  ( 0.000000000000000000, 0.000000000000000000, 0.000000000000000000 ) ) ;
#18869 = AXIS2_PLACEMENT_3D ( 'NONE', #1743, #12547, #34514 ) ;
#18870 = CARTESIAN_POINT ( 'NONE',  ( -21.00000000000000355, 0.000000000000000000, 70.00000000000000000 ) ) ;
#18871 = CARTESIAN_POINT ( 'NONE',  ( 8.000000000000000000, -13.55483219355720337, -11.06713717293254362 ) ) ;
#18872 = ORIENTED_EDGE ( 'NONE', *, *, #2748, .T. ) ;
#18873 = ORIENTED_EDGE ( 'NONE', *, *, #28174, .F. ) ;
#18874 = CARTESIAN_POINT ( 'NONE',  ( -35.50000000000000711, -112.6919296022648638, -1.573728109100751116 ) ) ;
#18875 = AXIS2_PLACEMENT_3D ( 'NONE', #16241, #2600, #32832 ) ;
#18876 = DIRECTION ( 'NONE',  ( 1.000000000000000000, -0.000000000000000000, -0.000000000000000000 ) ) ;
#18877 = CYLINDRICAL_SURFACE ( 'NONE', #17811, 8.000000000000000000 ) ;
#18878 = VERTEX_POINT ( 'NONE', #14753 ) ;
#18879 = MECHANICAL_DESIGN_GEOMETRIC_PRESENTATION_REPRESENTATION (  '', ( #29742 ), #7879 ) ;
#18880 = DIRECTION ( 'NONE',  ( 1.000000000000000000, 0.000000000000000000, 0.000000000000000000 ) ) ;
#18881 = CARTESIAN_POINT ( 'NONE',  ( -34.50000000000000000, -114.8474311500471572, -1.624782352598427959 ) ) ;
#18882 = EDGE_CURVE ( 'NONE', #18371, #22842, #9648, .T. ) ;
#18883 = CARTESIAN_POINT ( 'NONE',  ( -35.24442919769869320, -114.9929510916434339, 13.92914543265605509 ) ) ;
#18884 = ADVANCED_FACE ( 'NONE', ( #32398 ), #5048, .T. ) ;
#18885 = CARTESIAN_POINT ( 'NONE',  ( 0.000000000000000000, 0.000000000000000000, 0.000000000000000000 ) ) ;
#18886 = CARTESIAN_POINT ( 'NONE',  ( -35.50000000000000000, -113.9929510916434339, 10.50625754673586876 ) ) ;
#18887 = CYLINDRICAL_SURFACE ( 'NONE', #163, 4.000000000000000000 ) ;
#18888 = CARTESIAN_POINT ( 'NONE',  ( -34.50000000000000000, -114.0371586325023117, 9.504435485030890973 ) ) ;
#18889 = DIRECTION ( 'NONE',  ( -1.000000000000000000, 0.000000000000000000, 0.000000000000000000 ) ) ;
#18890 = DIRECTION ( 'NONE',  ( 1.000000000000000000, 1.734723475976807094E-16, -0.000000000000000000 ) ) ;
#18891 = CARTESIAN_POINT ( 'NONE',  ( 4.000000000000003553, -30.03615769709705319, -42.44795908869020451 ) ) ;
#18892 = ORIENTED_EDGE ( 'NONE', *, *, #30965, .F. ) ;
#18893 = DIRECTION ( 'NONE',  ( 0.000000000000000000, 0.000000000000000000, 1.000000000000000000 ) ) ;
#18894 = DIRECTION ( 'NONE',  ( -0.000000000000000000, -1.000000000000000000, 0.000000000000000000 ) ) ;
#18895 = ORIENTED_EDGE ( 'NONE', *, *, #9462, .F. ) ;
#18896 = CARTESIAN_POINT ( 'NONE',  ( -37.18750000000006395, -114.9929510916434339, 13.11852480586264669 ) ) ;
#18897 = ORIENTED_EDGE ( 'NONE', *, *, #6800, .F. ) ;
#18898 = EDGE_CURVE ( 'NONE', #5903, #15285, #15632, .T. ) ;
#18899 = CARTESIAN_POINT ( 'NONE',  ( -37.88768952767750164, -115.9754527089670262, 6.472274454178450043 ) ) ;
#18900 = AXIS2_PLACEMENT_3D ( 'NONE', #32616, #15856, #5267 ) ;
#18901 = LINE ( 'NONE', #24142, #15687 ) ;
#18902 = ORIENTED_EDGE ( 'NONE', *, *, #25520, .T. ) ;
#18903 = CIRCLE ( 'NONE', #28110, 4.000000000000000000 ) ;
#18904 = ORIENTED_EDGE ( 'NONE', *, *, #10156, .T. ) ;
#18905 = CARTESIAN_POINT ( 'NONE',  ( -55.00000000000000000, -2.726571689596996976E-14, 114.0000000000000000 ) ) ;
#18906 = DIRECTION ( 'NONE',  ( -1.000000000000000000, 0.000000000000000000, 0.000000000000000000 ) ) ;
#18907 = EDGE_LOOP ( 'NONE', ( #32607, #14733, #27657, #3724, #4373, #18041 ) ) ;
#18908 = CARTESIAN_POINT ( 'NONE',  ( -36.94073759706868287, -112.0000000000000142, 8.628524454178448266 ) ) ;
#18909 = CYLINDRICAL_SURFACE ( 'NONE', #18413, 11.00000000000000000 ) ;
#18910 = CARTESIAN_POINT ( 'NONE',  ( 0.000000000000000000, 12.30077720129095553, 50.52416135122086871 ) ) ;
#18911 = ORIENTED_EDGE ( 'NONE', *, *, #31287, .F. ) ;
#18912 = ORIENTED_EDGE ( 'NONE', *, *, #24504, .F. ) ;
#18913 = CARTESIAN_POINT ( 'NONE',  ( -50.00000000000000000, 0.000000000000000000, 0.000000000000000000 ) ) ;
#18914 = EDGE_CURVE ( 'NONE', #11899, #8697, #8074, .T. ) ;
#18915 = DIRECTION ( 'NONE',  ( 0.000000000000000000, 0.000000000000000000, -1.000000000000000000 ) ) ;
#18916 = VERTEX_POINT ( 'NONE', #19057 ) ;
#18917 = VERTEX_POINT ( 'NONE', #26654 ) ;
#18918 = CARTESIAN_POINT ( 'NONE',  ( -34.50000000000000000, -111.0780159515033034, -1.143161139953928762 ) ) ;
#18919 = DIRECTION ( 'NONE',  ( 1.000000000000000000, 0.000000000000000000, -1.691777834109591283E-31 ) ) ;
#18920 = ORIENTED_EDGE ( 'NONE', *, *, #16597, .T. ) ;
#18921 = CARTESIAN_POINT ( 'NONE',  ( -35.50000000000000711, -114.9928438774171582, 10.49113435197128652 ) ) ;
#18922 = EDGE_CURVE ( 'NONE', #22807, #26552, #4511, .T. ) ;
#18923 = CARTESIAN_POINT ( 'NONE',  ( -34.50015059926905536, -113.9929510916434339, 12.64306614848962518 ) ) ;
#18924 = ADVANCED_FACE ( 'NONE', ( #5226 ), #21400, .T. ) ;
#18925 = DIRECTION ( 'NONE',  ( -1.000000000000000000, -0.000000000000000000, -0.000000000000000000 ) ) ;
#18926 = CYLINDRICAL_SURFACE ( 'NONE', #8177, 47.49900000000001654 ) ;
#18927 = EDGE_CURVE ( 'NONE', #21695, #21999, #10249, .T. ) ;
#18928 = VECTOR ( 'NONE', #26619, 1000.000000000000000 ) ;
#18929 = CARTESIAN_POINT ( 'NONE',  ( -37.99959864031216483, -113.9929510916434339, 12.63896776382213538 ) ) ;
#18930 = CARTESIAN_POINT ( 'NONE',  ( -38.00000000000000711, -115.9929510916434481, 12.59652202191340820 ) ) ;
#18931 = DIRECTION ( 'NONE',  ( -1.000000000000000000, 0.000000000000000000, 0.000000000000000000 ) ) ;
#18932 = CARTESIAN_POINT ( 'NONE',  ( -55.00000000000000000, 10.00000000000000888, 110.0000000000000000 ) ) ;
#18933 = ORIENTED_EDGE ( 'NONE', *, *, #10237, .T. ) ;
#18934 = EDGE_CURVE ( 'NONE', #4303, #28364, #26942, .T. ) ;
#18935 = DIRECTION ( 'NONE',  ( 9.266685234918781277E-17, -6.938893903907202493E-17, -1.000000000000000000 ) ) ;
#18936 = CARTESIAN_POINT ( 'NONE',  ( 0.000000000000000000, 0.000000000000000000, 50.00000000000000000 ) ) ;
#18937 = CARTESIAN_POINT ( 'NONE',  ( 4.000000000000003553, 12.30077720129168384, -50.52416135122070528 ) ) ;
#18938 = ADVANCED_FACE ( 'NONE', ( #2352 ), #32222, .T. ) ;
#18939 = ORIENTED_EDGE ( 'NONE', *, *, #4442, .T. ) ;
#18940 = DIRECTION ( 'NONE',  ( 0.000000000000000000, 0.000000000000000000, -1.000000000000000000 ) ) ;
#18941 = ORIENTED_EDGE ( 'NONE', *, *, #35277, .F. ) ;
#18942 = CARTESIAN_POINT ( 'NONE',  ( -35.50000000000000711, -116.0140978167138712, -0.3122823525984417259 ) ) ;
#18943 = CARTESIAN_POINT ( 'NONE',  ( 0.000000000000000000, 0.000000000000000000, 0.000000000000000000 ) ) ;
#18944 = CIRCLE ( 'NONE', #31001, 17.49900000000001654 ) ;
#18945 = CARTESIAN_POINT ( 'NONE',  ( -35.50000000000000711, -114.9929510916434339, 12.26648026267477221 ) ) ;
#18946 = LINE ( 'NONE', #26719, #24570 ) ;
#18947 = ORIENTED_EDGE ( 'NONE', *, *, #20850, .F. ) ;
#18948 = AXIS2_PLACEMENT_3D ( 'NONE', #8423, #13667, #5737 ) ;
#18949 = CARTESIAN_POINT ( 'NONE',  ( 0.000000000000000000, 0.000000000000000000, -53.39999999999999858 ) ) ;
#18950 = CARTESIAN_POINT ( 'NONE',  ( -35.50000000000000000, -111.1162063037085801, -1.269118781493287607 ) ) ;
#18951 = ORIENTED_EDGE ( 'NONE', *, *, #22497, .F. ) ;
#18952 = ORIENTED_EDGE ( 'NONE', *, *, #15178, .T. ) ;
#18953 = CARTESIAN_POINT ( 'NONE',  ( -36.94073759706866156, -113.0000000000000000, 5.628524454178450043 ) ) ;
#18954 = VECTOR ( 'NONE', #20644, 1000.000000000000000 ) ;
#18955 = PRODUCT_DEFINITION_FORMATION_WITH_SPECIFIED_SOURCE ( 'ANY', '', #6342, .NOT_KNOWN. ) ;
#18956 = AXIS2_PLACEMENT_3D ( 'NONE', #29525, #4860, #26821 ) ;
#18957 = EDGE_CURVE ( 'NONE', #29894, #3630, #29699, .T. ) ;
#18958 =( NAMED_UNIT ( * ) PLANE_ANGLE_UNIT ( ) SI_UNIT ( $, .RADIAN. ) );
#18959 = DIRECTION ( 'NONE',  ( 1.000000000000000000, 0.000000000000000000, 0.000000000000000000 ) ) ;
#18960 = ORIENTED_EDGE ( 'NONE', *, *, #26421, .F. ) ;
#18961 = VERTEX_POINT ( 'NONE', #30056 ) ;
#18962 = CARTESIAN_POINT ( 'NONE',  ( -34.50000000000000000, -113.0140978167138996, -0.6247823525984302906 ) ) ;
#18963 = DIRECTION ( 'NONE',  ( 0.000000000000000000, 0.000000000000000000, 1.000000000000000000 ) ) ;
#18964 = PRODUCT_DEFINITION ( 'UNKNOWN', '', #32764, #28142 ) ;
#18965 = ADVANCED_FACE ( 'NONE', ( #15808 ), #10612, .T. ) ;
#18966 = CARTESIAN_POINT ( 'NONE',  ( -34.49999999999998579, -24.48076211353314591, 80.99999999999991473 ) ) ;
#18967 = CARTESIAN_POINT ( 'NONE',  ( 0.000000000000000000, -15.46619997295641369, -1.007799283846847471 ) ) ;
#18968 = CARTESIAN_POINT ( 'NONE',  ( -35.50000000000000000, -113.9883062625807071, 10.50570311110699961 ) ) ;
#18969 = FACE_OUTER_BOUND ( 'NONE', #15753, .T. ) ;
#18970 = EDGE_CURVE ( 'NONE', #15000, #30905, #10794, .T. ) ;
#18971 = DIRECTION ( 'NONE',  ( 1.000000000000000000, 0.000000000000000000, 0.000000000000000000 ) ) ;
#18972 = EDGE_CURVE ( 'NONE', #22936, #19114, #17726, .T. ) ;
#18973 = CARTESIAN_POINT ( 'NONE',  ( -34.50000000000000000, -114.3474311500471430, -1.624782352598427959 ) ) ;
#18974 = CARTESIAN_POINT ( 'NONE',  ( -36.15625000000007816, -115.9929510916434481, 14.11852480586265024 ) ) ;
#18975 = LINE ( 'NONE', #16077, #6519 ) ;
#18976 = CIRCLE ( 'NONE', #34513, 22.00000000000000000 ) ;
#18977 = CARTESIAN_POINT ( 'NONE',  ( 0.000000000000000000, -16.92083251265328769, 4.460989585140905156 ) ) ;
#18978 = ORIENTED_EDGE ( 'NONE', *, *, #4845, .F. ) ;
#18979 = AXIS2_PLACEMENT_3D ( 'NONE', #11163, #8274, #32953 ) ;
#18980 = CARTESIAN_POINT ( 'NONE',  ( -37.97447287825094264, -115.9929510916434481, 12.77960891308616809 ) ) ;
#18981 = DIRECTION ( 'NONE',  ( -1.734723475976807094E-16, 0.8660254037844385966, 0.5000000000000001110 ) ) ;
#18982 = CARTESIAN_POINT ( 'NONE',  ( 8.000000000000007105, -5.908880290975456973, -9.604183132802479150 ) ) ;
#18983 = AXIS2_PLACEMENT_3D ( 'NONE', #5987, #28134, #16944 ) ;
#18984 = FACE_OUTER_BOUND ( 'NONE', #14419, .T. ) ;
#18985 = CARTESIAN_POINT ( 'NONE',  ( 70.00000000000001421, -29.60243954609234507, 93.25429903592612391 ) ) ;
#18986 = EDGE_CURVE ( 'NONE', #30814, #34436, #12961, .T. ) ;
#18987 = EDGE_LOOP ( 'NONE', ( #18000, #15582 ) ) ;
#18988 = FACE_OUTER_BOUND ( 'NONE', #16682, .T. ) ;
#18989 = FACE_OUTER_BOUND ( 'NONE', #21608, .T. ) ;
#18990 = LINE ( 'NONE', #13419, #28597 ) ;
#18991 = DIRECTION ( 'NONE',  ( 0.000000000000000000, 0.000000000000000000, 1.000000000000000000 ) ) ;
#18992 = CARTESIAN_POINT ( 'NONE',  ( 0.000000000000000000, 4.898587196589413815E-16, -4.000000000000000000 ) ) ;
#18993 = FACE_OUTER_BOUND ( 'NONE', #35582, .T. ) ;
#18994 = ORIENTED_EDGE ( 'NONE', *, *, #13509, .F. ) ;
#18995 = ORIENTED_EDGE ( 'NONE', *, *, #13962, .F. ) ;
#18996 = DIRECTION ( 'NONE',  ( -1.000000000000000000, 0.000000000000000000, 0.000000000000000000 ) ) ;
#18997 = FACE_OUTER_BOUND ( 'NONE', #23887, .T. ) ;
#18998 = DIRECTION ( 'NONE',  ( 0.000000000000000000, 0.8660254037844381525, 0.5000000000000006661 ) ) ;
#18999 = VERTEX_POINT ( 'NONE', #21226 ) ;
#19000 = CARTESIAN_POINT ( 'NONE',  ( -37.76916472181486739, -116.0245472910329880, 7.465225545821551734 ) ) ;
#19001 = ORIENTED_EDGE ( 'NONE', *, *, #25082, .T. ) ;
#19002 = EDGE_CURVE ( 'NONE', #31360, #5795, #5121, .T. ) ;
#19003 = VERTEX_POINT ( 'NONE', #18295 ) ;
#19004 = VECTOR ( 'NONE', #12028, 1000.000000000000000 ) ;
#19005 = VERTEX_POINT ( 'NONE', #29470 ) ;
#19006 = DIRECTION ( 'NONE',  ( 1.000000000000000000, -0.000000000000000000, 0.000000000000000000 ) ) ;
#19007 = EDGE_CURVE ( 'NONE', #17557, #8797, #13165, .T. ) ;
#19008 = ADVANCED_FACE ( 'NONE', ( #26051 ), #4811, .T. ) ;
#19009 = CIRCLE ( 'NONE', #31060, 4.000000000000000000 ) ;
#19010 = AXIS2_PLACEMENT_3D ( 'NONE', #21957, #2733, #21781 ) ;
#19011 = VECTOR ( 'NONE', #25572, 1000.000000000000000 ) ;
#19012 = VERTEX_POINT ( 'NONE', #17930 ) ;
#19013 = ORIENTED_EDGE ( 'NONE', *, *, #22731, .F. ) ;
#19014 = DIRECTION ( 'NONE',  ( 0.000000000000000000, 0.000000000000000000, 1.000000000000000000 ) ) ;
#19015 = DIRECTION ( 'NONE',  ( 0.000000000000000000, 0.8090169943749488946, -0.5877852522924709167 ) ) ;
#19016 = EDGE_CURVE ( 'NONE', #26725, #11394, #1641, .T. ) ;
#19017 = DIRECTION ( 'NONE',  ( -1.000000000000000000, 0.000000000000000000, 0.000000000000000000 ) ) ;
#19018 = ADVANCED_FACE ( 'NONE', ( #28927 ), #9476, .T. ) ;
#19019 = CYLINDRICAL_SURFACE ( 'NONE', #24032, 4.000000000000000000 ) ;
#19020 = DIRECTION ( 'NONE',  ( -1.000000000000000000, -0.000000000000000000, 0.000000000000000000 ) ) ;
#19021 = FACE_BOUND ( 'NONE', #3743, .T. ) ;
#19022 = CARTESIAN_POINT ( 'NONE',  ( -36.03906250000000000, -115.9929510916434481, 14.11852480586265024 ) ) ;
#19023 = CARTESIAN_POINT ( 'NONE',  ( 8.000000000000000000, 12.49559743815781587, 9.169462670380628566 ) ) ;
#19024 = DIRECTION ( 'NONE',  ( -1.000000000000000000, 0.000000000000000000, 0.000000000000000000 ) ) ;
#19025 = DIRECTION ( 'NONE',  ( -1.000000000000000000, 0.000000000000000000, 0.000000000000000000 ) ) ;
#19026 = DIRECTION ( 'NONE',  ( 0.000000000000000000, 0.000000000000000000, -1.000000000000000000 ) ) ;
#19027 = DIRECTION ( 'NONE',  ( 0.000000000000000000, -6.938893903907203726E-17, -1.000000000000000000 ) ) ;
#19028 =( NAMED_UNIT ( * ) SI_UNIT ( $, .STERADIAN. ) SOLID_ANGLE_UNIT ( ) );
#19029 = VERTEX_POINT ( 'NONE', #6957 ) ;
#19030 = CARTESIAN_POINT ( 'NONE',  ( -36.33479806579560289, -113.2509883718313262, 3.808975545821551734 ) ) ;
#19031 = PLANE ( 'NONE',  #6606 ) ;
#19032 = CARTESIAN_POINT ( 'NONE',  ( 0.000000000000000000, -12.30077720129063756, -50.52416135122095397 ) ) ;
#19033 = DIRECTION ( 'NONE',  ( 0.000000000000000000, 0.000000000000000000, -1.000000000000000000 ) ) ;
#19034 = PRESENTATION_LAYER_ASSIGNMENT (  '', '', ( #20740 ) ) ;
#19035 = VERTEX_POINT ( 'NONE', #12728 ) ;
#19036 = EDGE_LOOP ( 'NONE', ( #34956, #19791, #12281, #5546 ) ) ;
#19037 = DIRECTION ( 'NONE',  ( -1.000000000000000000, 0.000000000000000000, 0.000000000000000000 ) ) ;
#19038 = CARTESIAN_POINT ( 'NONE',  ( 0.000000000000000000, -2.710505431213761085E-17, -30.90000000000000568 ) ) ;
#19039 = ORIENTED_EDGE ( 'NONE', *, *, #32878, .F. ) ;
#19040 = ORIENTED_EDGE ( 'NONE', *, *, #20535, .T. ) ;
#19041 = ADVANCED_FACE ( 'NONE', ( #34877 ), #26593, .T. ) ;
#19042 = DIRECTION ( 'NONE',  ( -1.000000000000000000, 0.000000000000000000, 0.000000000000000000 ) ) ;
#19043 = DIRECTION ( 'NONE',  ( 1.000000000000000000, -1.110223024625156540E-16, 0.000000000000000000 ) ) ;
#19044 = AXIS2_PLACEMENT_3D ( 'NONE', #24787, #13281, #32350 ) ;
#19045 = PRODUCT_CONTEXT ( 'NONE', #34480, 'mechanical' ) ;
#19046 = DIRECTION ( 'NONE',  ( 1.000000000000000000, 0.000000000000000000, -1.691777834109591064E-31 ) ) ;
#19047 = VERTEX_POINT ( 'NONE', #15400 ) ;
#19048 = EDGE_LOOP ( 'NONE', ( #4561, #17073, #7498, #3728 ) ) ;
#19049 = FACE_OUTER_BOUND ( 'NONE', #34013, .T. ) ;
#19050 = CARTESIAN_POINT ( 'NONE',  ( -44.00000000000000000, -11.00000000000000000, 0.000000000000000000 ) ) ;
#19051 = AXIS2_PLACEMENT_3D ( 'NONE', #27937, #25424, #16763 ) ;
#19052 = ORIENTED_EDGE ( 'NONE', *, *, #11253, .T. ) ;
#19053 = CIRCLE ( 'NONE', #33419, 52.00000000000000711 ) ;
#19054 = DIRECTION ( 'NONE',  ( 1.000000000000000000, -0.000000000000000000, -0.000000000000000000 ) ) ;
#19055 = CARTESIAN_POINT ( 'NONE',  ( -34.50000000000000000, -114.9724313160460696, -1.624792769101446765 ) ) ;
#19056 = CARTESIAN_POINT ( 'NONE',  ( -38.99518666717493431, -114.9929510916434339, 12.74107470552714716 ) ) ;
#19057 = CARTESIAN_POINT ( 'NONE',  ( -0.3000000000000016542, -14.69693845669907439, 0.000000000000000000 ) ) ;
#19058 = CARTESIAN_POINT ( 'NONE',  ( -38.00000000000000711, -114.9929510916434339, 12.26648026267477043 ) ) ;
#19059 = LINE ( 'NONE', #15460, #189 ) ;
#19060 = CARTESIAN_POINT ( 'NONE',  ( -34.50000000000000000, -114.9929510916434339, 12.53051367006571581 ) ) ;
#19061 = DIRECTION ( 'NONE',  ( -0.9914448613738098270, -0.1305261922200566527, 1.108939053204896328E-15 ) ) ;
#19062 = DIRECTION ( 'NONE',  ( -1.000000000000000000, 0.000000000000000000, 0.000000000000000000 ) ) ;
#19063 = DIRECTION ( 'NONE',  ( 0.000000000000000000, 0.000000000000000000, -1.000000000000000000 ) ) ;
#19064 = DIRECTION ( 'NONE',  ( -1.000000000000000000, 0.000000000000000000, 0.000000000000000000 ) ) ;
#19065 = CYLINDRICAL_SURFACE ( 'NONE', #31969, 20.00000000000000355 ) ;
#19066 = CARTESIAN_POINT ( 'NONE',  ( 0.000000000000000000, 0.000000000000000000, 0.000000000000000000 ) ) ;
#19067 = ORIENTED_EDGE ( 'NONE', *, *, #12179, .F. ) ;
#19068 = LINE ( 'NONE', #30762, #33667 ) ;
#19069 = ORIENTED_EDGE ( 'NONE', *, *, #17863, .F. ) ;
#19070 = CARTESIAN_POINT ( 'NONE',  ( -38.97545270896704039, -113.1123104723225197, 5.347274454178449155 ) ) ;
#19071 = DIRECTION ( 'NONE',  ( 0.000000000000000000, 0.000000000000000000, -1.000000000000000000 ) ) ;
#19072 = VERTEX_POINT ( 'NONE', #1383 ) ;
#19073 = ORIENTED_EDGE ( 'NONE', *, *, #6635, .F. ) ;
#19074 = LINE ( 'NONE', #13513, #5637 ) ;
#19075 = CARTESIAN_POINT ( 'NONE',  ( 0.000000000000000000, 0.000000000000000000, 0.000000000000000000 ) ) ;
#19076 = AXIS2_PLACEMENT_3D ( 'NONE', #18209, #26145, #23626 ) ;
#19077 = MECHANICAL_DESIGN_GEOMETRIC_PRESENTATION_REPRESENTATION (  '', ( #30571 ), #31725 ) ;
#19078 = ORIENTED_EDGE ( 'NONE', *, *, #2520, .T. ) ;
#19079 = CIRCLE ( 'NONE', #2997, 14.00000000000000000 ) ;
#19080 = CARTESIAN_POINT ( 'NONE',  ( -39.16322519054179452, -116.0794154965774823, 6.566024454178448266 ) ) ;
#19081 = CARTESIAN_POINT ( 'NONE',  ( 0.1717365941144993746, -6.008326913195982222, -0.7999999999999951594 ) ) ;
#19082 = EDGE_CURVE ( 'NONE', #10765, #26461, #20978, .T. ) ;
#19083 = PLANE ( 'NONE',  #14215 ) ;
#19084 = ORIENTED_EDGE ( 'NONE', *, *, #8066, .F. ) ;
#19085 = ORIENTED_EDGE ( 'NONE', *, *, #25553, .F. ) ;
#19086 = CYLINDRICAL_SURFACE ( 'NONE', #16530, 52.00000000000000711 ) ;
#19087 = DIRECTION ( 'NONE',  ( -1.000000000000000000, 0.000000000000000000, 0.000000000000000000 ) ) ;
#19088 = ORIENTED_EDGE ( 'NONE', *, *, #27956, .T. ) ;
#19089 = VERTEX_POINT ( 'NONE', #23158 ) ;
#19090 = AXIS2_PLACEMENT_3D ( 'NONE', #4707, #27013, #10078 ) ;
#19091 = CARTESIAN_POINT ( 'NONE',  ( -34.50000000000000000, -112.9650106922503170, -2.624765990393421955 ) ) ;
#19092 = EDGE_CURVE ( 'NONE', #26596, #11196, #12359, .T. ) ;
#19093 = DIRECTION ( 'NONE',  ( -1.000000000000000000, 0.000000000000000000, 0.000000000000000000 ) ) ;
#19094 = VERTEX_POINT ( 'NONE', #18106 ) ;
#19095 = CARTESIAN_POINT ( 'NONE',  ( -35.50000000000000711, -114.9860996047076895, 10.38555023491505835 ) ) ;
#19096 = CARTESIAN_POINT ( 'NONE',  ( -36.87500000000098765, -113.9929510916434339, 14.11852480586265024 ) ) ;
#19097 = VECTOR ( 'NONE', #31899, 1000.000000000000000 ) ;
#19098 = FACE_OUTER_BOUND ( 'NONE', #28490, .T. ) ;
#19099 = DIRECTION ( 'NONE',  ( 0.000000000000000000, 0.8660254037844365982, 0.5000000000000035527 ) ) ;
#19100 = VECTOR ( 'NONE', #22985, 1000.000000000000000 ) ;
#19101 = AXIS2_PLACEMENT_3D ( 'NONE', #29474, #11262, #3002 ) ;
#19102 = CARTESIAN_POINT ( 'NONE',  ( -34.50000000000000000, -113.9929510916434339, 10.50763272073269405 ) ) ;
#19103 = CARTESIAN_POINT ( 'NONE',  ( -39.00000000000000711, -114.9929510916434339, 12.53051367006571937 ) ) ;
#19104 = CARTESIAN_POINT ( 'NONE',  ( -35.50000000000000711, -114.1189822439768449, 9.514224058074130852 ) ) ;
#19105 = DIRECTION ( 'NONE',  ( -1.000000000000000000, 0.000000000000000000, 0.000000000000000000 ) ) ;
#19106 = DIRECTION ( 'NONE',  ( 0.000000000000000000, 0.000000000000000000, 1.000000000000000000 ) ) ;
#19107 = ORIENTED_EDGE ( 'NONE', *, *, #9049, .T. ) ;
#19108 = LINE ( 'NONE', #35519, #17186 ) ;
#19109 = CARTESIAN_POINT ( 'NONE',  ( 0.000000000000000000, 0.000000000000000000, 0.000000000000000000 ) ) ;
#19110 = FACE_OUTER_BOUND ( 'NONE', #21680, .T. ) ;
#19111 = ORIENTED_EDGE ( 'NONE', *, *, #20653, .T. ) ;
#19112 = AXIS2_PLACEMENT_3D ( 'NONE', #6531, #17505, #3144 ) ;
#19113 = CARTESIAN_POINT ( 'NONE',  ( 7.999999999999992895, 5.871425383721554425, 51.66745943012285380 ) ) ;
#19114 = VERTEX_POINT ( 'NONE', #15217 ) ;
#19115 = CARTESIAN_POINT ( 'NONE',  ( -35.50000000000000000, -113.1981689815712997, 0.8971895242272823756 ) ) ;
#19116 = CARTESIAN_POINT ( 'NONE',  ( -1.498621416870293155, -4.588090364676976828E-14, 7.020000000000020890 ) ) ;
#19117 = CARTESIAN_POINT ( 'NONE',  ( -36.52652403469556930, -113.0245472910329880, 2.722274454178449155 ) ) ;
#19118 = CARTESIAN_POINT ( 'NONE',  ( -35.50000000000000711, -114.9929510916434339, 12.53051367006571581 ) ) ;
#19119 = VERTEX_POINT ( 'NONE', #10016 ) ;
#19120 = AXIS2_PLACEMENT_3D ( 'NONE', #5837, #25458, #14101 ) ;
#19121 = EDGE_CURVE ( 'NONE', #10004, #20300, #15045, .T. ) ;
#19122 = CARTESIAN_POINT ( 'NONE',  ( -35.50000000000000000, -111.0780159515033034, -1.143161139953928762 ) ) ;
#19123 = AXIS2_PLACEMENT_3D ( 'NONE', #12421, #34575, #900 ) ;
#19124 = VERTEX_POINT ( 'NONE', #23703 ) ;
#19125 = ORIENTED_EDGE ( 'NONE', *, *, #31080, .F. ) ;
#19126 = EDGE_CURVE ( 'NONE', #14743, #4610, #20598, .T. ) ;
#19127 = CARTESIAN_POINT ( 'NONE',  ( -35.97545270896702618, -113.6450488405582604, 7.409774454178449155 ) ) ;
#19128 = CARTESIAN_POINT ( 'NONE',  ( -3.799999999999999822, -2.710505431213761085E-17, -45.10000000000000142 ) ) ;
#19129 = ORIENTED_EDGE ( 'NONE', *, *, #23644, .T. ) ;
#19130 = EDGE_LOOP ( 'NONE', ( #30566, #24152, #26142, #12267 ) ) ;
#19131 = CARTESIAN_POINT ( 'NONE',  ( -34.50000000000000000, -113.0140978167138712, -0.6247823525985405357 ) ) ;
#19132 = DIRECTION ( 'NONE',  ( -1.000000000000000000, 0.000000000000000000, 0.000000000000000000 ) ) ;
#19133 = EDGE_CURVE ( 'NONE', #9066, #11629, #4461, .T. ) ;
#19134 = LINE ( 'NONE', #11050, #5722 ) ;
#19135 = ADVANCED_FACE ( 'NONE', ( #17751 ), #1564, .F. ) ;
#19136 = LINE ( 'NONE', #17090, #24316 ) ;
#19137 = AXIS2_PLACEMENT_3D ( 'NONE', #18160, #29523, #21030 ) ;
#19138 = AXIS2_PLACEMENT_3D ( 'NONE', #30888, #17183, #11445 ) ;
#19139 = CARTESIAN_POINT ( 'NONE',  ( -35.50000000000000000, -113.9929510916434339, 11.73841344789270202 ) ) ;
#19140 = VECTOR ( 'NONE', #30684, 1000.000000000000000 ) ;
#19141 = DIRECTION ( 'NONE',  ( -1.000000000000000000, 0.000000000000000000, 0.000000000000000000 ) ) ;
#19142 = CARTESIAN_POINT ( 'NONE',  ( 8.000000000000007105, 0.000000000000000000, 0.000000000000000000 ) ) ;
#19143 = CARTESIAN_POINT ( 'NONE',  ( -34.50000000000000000, -113.6807644833805995, -1.624782352598427959 ) ) ;
#19144 = CARTESIAN_POINT ( 'NONE',  ( -38.99699093265172678, -115.9929510916434481, 12.71660600561481402 ) ) ;
#19145 = DIRECTION ( 'NONE',  ( -1.000000000000000000, 0.000000000000000000, 0.000000000000000000 ) ) ;
#19146 = AXIS2_PLACEMENT_3D ( 'NONE', #17287, #16926, #732 ) ;
#19147 = CIRCLE ( 'NONE', #22031, 10.00000000000000000 ) ;
#19148 = DIRECTION ( 'NONE',  ( -1.000000000000000000, -0.000000000000000000, 0.000000000000000000 ) ) ;
#19149 = ORIENTED_EDGE ( 'NONE', *, *, #33446, .T. ) ;
#19150 = CARTESIAN_POINT ( 'NONE',  ( -38.00000000000000711, -115.9929510916434481, 12.60752341388803721 ) ) ;
#19151 = DIRECTION ( 'NONE',  ( 0.000000000000000000, 0.000000000000000000, 1.000000000000000000 ) ) ;
#19152 = DIRECTION ( 'NONE',  ( -1.836970198721029934E-16, 1.000000000000000000, 0.000000000000000000 ) ) ;
#19153 = CARTESIAN_POINT ( 'NONE',  ( 4.000000000000000000, 17.56975900509189970, -9.555290079479078713 ) ) ;
#19154 = EDGE_CURVE ( 'NONE', #8803, #27165, #12906, .T. ) ;
#19155 = CYLINDRICAL_SURFACE ( 'NONE', #1565, 13.99999999999999822 ) ;
#19156 = VERTEX_POINT ( 'NONE', #4640 ) ;
#19157 = DIRECTION ( 'NONE',  ( -1.000000000000000000, 0.000000000000000000, 0.000000000000000000 ) ) ;
#19158 = CYLINDRICAL_SURFACE ( 'NONE', #34249, 52.00000000000000711 ) ;
#19159 = DIRECTION ( 'NONE',  ( 0.000000000000000000, 0.000000000000000000, 1.000000000000000000 ) ) ;
#19160 = CARTESIAN_POINT ( 'NONE',  ( 3.872983346207517386, -1.000000000000028644, -32.00000000000000000 ) ) ;
#19161 = ITEM_DEFINED_TRANSFORMATION ( 'NONE', 'NONE', #5180,  #21307 ) ;
#19162 = DIRECTION ( 'NONE',  ( -1.000000000000000000, 0.000000000000000000, 0.000000000000000000 ) ) ;
#19163 = CYLINDRICAL_SURFACE ( 'NONE', #4989, 52.00000000000000711 ) ;
#19164 = AXIS2_PLACEMENT_3D ( 'NONE', #24818, #5219, #16157 ) ;
#19165 = EDGE_LOOP ( 'NONE', ( #18895, #14375, #18424, #33909 ) ) ;
#19166 = LINE ( 'NONE', #13782, #2101 ) ;
#19167 = ADVANCED_FACE ( 'NONE', ( #1929 ), #15573, .T. ) ;
#19168 = CARTESIAN_POINT ( 'NONE',  ( 0.000000000000000000, 0.000000000000000000, 0.000000000000000000 ) ) ;
#19169 = DIRECTION ( 'NONE',  ( 1.000000000000000000, -5.339440136655842133E-16, -1.047965281155519420E-16 ) ) ;
#19170 = ORIENTED_EDGE ( 'NONE', *, *, #8025, .T. ) ;
#19171 = EDGE_CURVE ( 'NONE', #30052, #4766, #7489, .T. ) ;
#19172 = CARTESIAN_POINT ( 'NONE',  ( -35.00000000000000000, -113.9407375970686900, 3.996475545821551290 ) ) ;
#19173 = EDGE_CURVE ( 'NONE', #1617, #9760, #13717, .T. ) ;
#19174 = ORIENTED_EDGE ( 'NONE', *, *, #32878, .T. ) ;
#19175 = FILL_AREA_STYLE_COLOUR ( '', #13843 ) ;
#19176 = VERTEX_POINT ( 'NONE', #35405 ) ;
#19177 = ORIENTED_EDGE ( 'NONE', *, *, #7697, .F. ) ;
#19178 = DIRECTION ( 'NONE',  ( 0.000000000000000000, 0.000000000000000000, -1.000000000000000000 ) ) ;
#19179 = AXIS2_PLACEMENT_3D ( 'NONE', #11679, #3244, #22837 ) ;
#19180 = AXIS2_PLACEMENT_3D ( 'NONE', #19573, #22630, #19227 ) ;
#19181 = AXIS2_PLACEMENT_3D ( 'NONE', #34470, #14831, #1159 ) ;
#19182 = ADVANCED_FACE ( 'NONE', ( #27300 ), #32337, .T. ) ;
#19183 = DIRECTION ( 'NONE',  ( -1.000000000000000000, 0.000000000000000000, 0.000000000000000000 ) ) ;
#19184 = ORIENTED_EDGE ( 'NONE', *, *, #21404, .F. ) ;
#19185 = CARTESIAN_POINT ( 'NONE',  ( -35.50000000000000711, -114.9929510916434339, 10.52000928670414126 ) ) ;
#19186 = PLANE ( 'NONE',  #23546 ) ;
#19187 = CYLINDRICAL_SURFACE ( 'NONE', #21740, 7.000000000000035527 ) ;
#19188 = DIRECTION ( 'NONE',  ( -0.000000000000000000, 0.000000000000000000, -1.000000000000000000 ) ) ;
#19189 = CARTESIAN_POINT ( 'NONE',  ( -50.00000000000000000, 19.99999999999998934, 120.0000000000000000 ) ) ;
#19190 = DIRECTION ( 'NONE',  ( -1.000000000000000000, -0.000000000000000000, 0.000000000000000000 ) ) ;
#19191 = CARTESIAN_POINT ( 'NONE',  ( -38.42182118622945808, -115.9929510916434481, 13.81802396319329773 ) ) ;
#19192 = CARTESIAN_POINT ( 'NONE',  ( 7.999999999999992895, -24.72041153920761758, 40.55929306992680949 ) ) ;
#19193 = ADVANCED_FACE ( 'NONE', ( #10732, #5690 ), #32701, .T. ) ;
#19194 = CARTESIAN_POINT ( 'NONE',  ( -4.000000000000000000, -2.710505431213761085E-17, 45.10000000000000142 ) ) ;
#19195 = CARTESIAN_POINT ( 'NONE',  ( 8.000000000000000000, -1.693188892523641798, -15.40623615209873876 ) ) ;
#19196 = CARTESIAN_POINT ( 'NONE',  ( -21.15833593587365513, -30.19486372867100954, 85.70096189432321410 ) ) ;
#19197 = CIRCLE ( 'NONE', #7147, 8.000000000000001776 ) ;
#19198 = ADVANCED_FACE ( 'NONE', ( #22060 ), #33055, .T. ) ;
#19199 = CARTESIAN_POINT ( 'NONE',  ( 70.00000600000001327, -25.98076211353320986, 88.99999999999994316 ) ) ;
#19200 = ORIENTED_EDGE ( 'NONE', *, *, #35497, .F. ) ;
#19201 = CARTESIAN_POINT ( 'NONE',  ( -38.97545270896704039, -114.8876895276775087, 7.652725545821552622 ) ) ;
#19202 = CYLINDRICAL_SURFACE ( 'NONE', #8327, 11.00000000000000000 ) ;
#19203 = CARTESIAN_POINT ( 'NONE',  ( -36.49999999999999289, -11.52052244843579309, 115.1848168619253698 ) ) ;
#19204 = CARTESIAN_POINT ( 'NONE',  ( 0.000000000000000000, 0.000000000000000000, 0.000000000000000000 ) ) ;
#19205 = EDGE_LOOP ( 'NONE', ( #11124, #15693, #29545, #31136 ) ) ;
#19206 = VERTEX_POINT ( 'NONE', #26958 ) ;
#19207 = CARTESIAN_POINT ( 'NONE',  ( 4.000000000000003553, -36.06787431788704623, 37.45808914225476371 ) ) ;
#19208 = EDGE_LOOP ( 'NONE', ( #21380, #18226, #24067, #22782, #9879, #28045, #5203, #17625 ) ) ;
#19209 = EDGE_CURVE ( 'NONE', #33313, #18606, #10278, .T. ) ;
#19210 = ORIENTED_EDGE ( 'NONE', *, *, #5609, .F. ) ;
#19211 = ADVANCED_FACE ( 'NONE', ( #2299 ), #8369, .T. ) ;
#19212 = DIRECTION ( 'NONE',  ( -1.000000000000000000, 0.000000000000000000, 0.000000000000000000 ) ) ;
#19213 = CARTESIAN_POINT ( 'NONE',  ( 0.000000000000000000, 0.000000000000000000, -49.10000000000000142 ) ) ;
#19214 = CARTESIAN_POINT ( 'NONE',  ( 8.000000000000000000, 12.46108038583334299, -15.64357617738981787 ) ) ;
#19215 = ORIENTED_EDGE ( 'NONE', *, *, #21239, .F. ) ;
#19216 = ORIENTED_EDGE ( 'NONE', *, *, #9739, .T. ) ;
#19217 = AXIS2_PLACEMENT_3D ( 'NONE', #9657, #20790, #31087 ) ;
#19218 = AXIS2_PLACEMENT_3D ( 'NONE', #15468, #1100, #4342 ) ;
#19219 = CARTESIAN_POINT ( 'NONE',  ( -9.999999999999994671, 0.000000000000000000, 0.000000000000000000 ) ) ;
#19220 = DIRECTION ( 'NONE',  ( -1.000000000000000000, 1.502314598737164455E-16, -8.673617379883947958E-17 ) ) ;
#19221 = ORIENTED_EDGE ( 'NONE', *, *, #18685, .T. ) ;
#19222 = CARTESIAN_POINT ( 'NONE',  ( 50.00000000000000000, 9.797174393178825657E-16, 8.000000000000000000 ) ) ;
#19223 = CIRCLE ( 'NONE', #3723, 47.49900000000000944 ) ;
#19224 = CARTESIAN_POINT ( 'NONE',  ( -34.50000000000000000, -113.0557643173828524, -1.624792769101735868 ) ) ;
#19225 = CARTESIAN_POINT ( 'NONE',  ( -37.34375000000001421, -114.9929510916434339, 14.11852480586264846 ) ) ;
#19226 = CARTESIAN_POINT ( 'NONE',  ( -38.00000000000000711, -114.9929510916434339, 12.53051367006571937 ) ) ;
#19227 = DIRECTION ( 'NONE',  ( 0.000000000000000000, -6.245004513516508695E-15, -1.000000000000000000 ) ) ;
#19228 = CARTESIAN_POINT ( 'NONE',  ( -35.24442919769869320, -114.9929510916434339, 13.92914543265605509 ) ) ;
#19229 = DIRECTION ( 'NONE',  ( 0.000000000000000000, 0.000000000000000000, -1.000000000000000000 ) ) ;
#19230 = ADVANCED_FACE ( 'NONE', ( #27488 ), #13271, .F. ) ;
#19231 = CYLINDRICAL_SURFACE ( 'NONE', #31618, 52.00000000000000711 ) ;
#19232 = FILL_AREA_STYLE ('',( #27363 ) ) ;
#19233 = DIRECTION ( 'NONE',  ( -1.000000000000000000, 0.000000000000000000, -0.000000000000000000 ) ) ;
#19234 = FACE_OUTER_BOUND ( 'NONE', #348, .T. ) ;
#19235 = FACE_OUTER_BOUND ( 'NONE', #21544, .T. ) ;
#19236 = EDGE_CURVE ( 'NONE', #15285, #17135, #19348, .T. ) ;
#19237 = VERTEX_POINT ( 'NONE', #26773 ) ;
#19238 = CARTESIAN_POINT ( 'NONE',  ( 0.000000000000000000, 0.000000000000000000, 55.00000000000000000 ) ) ;
#19239 = VERTEX_POINT ( 'NONE', #13436 ) ;
#19240 = CARTESIAN_POINT ( 'NONE',  ( -34.02454729103298092, -115.3019030900506294, 4.597274454178449155 ) ) ;
#19241 = FACE_BOUND ( 'NONE', #23099, .T. ) ;
#19242 = VERTEX_POINT ( 'NONE', #5343 ) ;
#19243 = ORIENTED_EDGE ( 'NONE', *, *, #25928, .T. ) ;
#19244 = CLOSED_SHELL ( 'NONE', ( #2866, #10402, #24391, #4457, #10380, #22326, #11412, #31116, #28190, #29801, #6244, #1136, #28439, #23407, #29472, #23074, #19397, #16439, #29009, #18597, #23265, #15916, #29263, #13617, #1530, #12565, #4239, #26674, #11276, #35098, #27835, #4208, #14205, #19875, #15211, #239, #11221, #30159, #17623, #19018, #24480, #31460, #19230, #5378, #29664, #30841, #17454, #35023, #7069, #30995, #30033, #30999, #35329, #17597, #18201, #18924, #7582, #20553, #34597, #8237, #1912, #24229, #19135, #29717, #6198, #16101, #28397, #34516, #27525 ) ) ;
#19245 = CARTESIAN_POINT ( 'NONE',  ( 7.999999999999992895, 17.50309955389674954, -43.60271849949345579 ) ) ;
#19246 = AXIS2_PLACEMENT_3D ( 'NONE', #30939, #16543, #30760 ) ;
#19247 = CARTESIAN_POINT ( 'NONE',  ( 4.000000000000003553, -21.63912866391137868, -3.968388925835035330 ) ) ;
#19248 = VERTEX_POINT ( 'NONE', #2645 ) ;
#19249 = CARTESIAN_POINT ( 'NONE',  ( -39.97545270896702618, -112.6980969099493990, 6.847274454178448266 ) ) ;
#19250 = CIRCLE ( 'NONE', #2604, 8.000000000000007105 ) ;
#19251 = AXIS2_PLACEMENT_3D ( 'NONE', #33604, #12008, #18423 ) ;
#19252 = DIRECTION ( 'NONE',  ( 1.000000000000000000, 1.734723475976807094E-16, 0.000000000000000000 ) ) ;
#19253 = CARTESIAN_POINT ( 'NONE',  ( 55.00000000000000711, -25.98076211353320986, 84.99999999999994316 ) ) ;
#19254 = EDGE_LOOP ( 'NONE', ( #32644, #21249, #23284, #23598 ) ) ;
#19255 = ORIENTED_EDGE ( 'NONE', *, *, #31053, .F. ) ;
#19256 = CARTESIAN_POINT ( 'NONE',  ( 7.999999999999992895, 2.123073309835863842, -47.45152853935333326 ) ) ;
#19257 =( LENGTH_UNIT ( ) NAMED_UNIT ( * ) SI_UNIT ( .MILLI., .METRE. ) );
#19258 = DIRECTION ( 'NONE',  ( 1.000000000000000000, -0.000000000000000000, -0.000000000000000000 ) ) ;
#19260 = VERTEX_POINT ( 'NONE', #24603 ) ;
#19259 = VECTOR ( 'NONE', #19466, 1000.000000000000000 ) ;
#19261 = ORIENTED_EDGE ( 'NONE', *, *, #23155, .F. ) ;
#19262 = CARTESIAN_POINT ( 'NONE',  ( -34.50000000000000000, -115.2751396785629510, -2.608751991713152307 ) ) ;
#19263 = CARTESIAN_POINT ( 'NONE',  ( 0.9999999999999870104, -5.408326913195881325, 0.000000000000000000 ) ) ;
#19264 = ORIENTED_EDGE ( 'NONE', *, *, #9258, .F. ) ;
#19265 = CARTESIAN_POINT ( 'NONE',  ( -35.50000000000000711, -114.9929510916434339, 12.50851088611648088 ) ) ;
#19266 = CIRCLE ( 'NONE', #7760, 20.00000000000000000 ) ;
#19267 = CARTESIAN_POINT ( 'NONE',  ( -35.75562914091914024, -113.9929510916434339, 14.09929883582542409 ) ) ;
#19268 = CIRCLE ( 'NONE', #6599, 9.999999999999994671 ) ;
#19269 = CARTESIAN_POINT ( 'NONE',  ( 8.000000000000000000, 0.000000000000000000, 0.000000000000000000 ) ) ;
#19270 = DIRECTION ( 'NONE',  ( 1.000000000000000000, -0.000000000000000000, -0.000000000000000000 ) ) ;
#19271 = CARTESIAN_POINT ( 'NONE',  ( -34.50000000000000000, -113.9929510916433060, 10.50625754673589540 ) ) ;
#19272 = CARTESIAN_POINT ( 'NONE',  ( -39.00000000000000711, -114.9929510916434339, 12.60752341388803721 ) ) ;
#19273 = VECTOR ( 'NONE', #30514, 1000.000000000000000 ) ;
#19274 = CARTESIAN_POINT ( 'NONE',  ( -35.50000000000000711, -114.9929510916434339, 10.56126450660895699 ) ) ;
#19275 = DIRECTION ( 'NONE',  ( -1.000000000000000000, 0.000000000000000000, 0.000000000000000000 ) ) ;
#19276 = DIRECTION ( 'NONE',  ( 0.000000000000000000, 0.000000000000000000, -1.000000000000000000 ) ) ;
#19277 = EDGE_CURVE ( 'NONE', #6546, #251, #495, .T. ) ;
#19278 = VERTEX_POINT ( 'NONE', #11091 ) ;
#19279 = ORIENTED_EDGE ( 'NONE', *, *, #35310, .T. ) ;
#19280 = LINE ( 'NONE', #8128, #32087 ) ;
#19281 = CYLINDRICAL_SURFACE ( 'NONE', #18589, 22.00000000000000000 ) ;
#19282 = AXIS2_PLACEMENT_3D ( 'NONE', #9782, #25196, #8084 ) ;
#19283 = EDGE_LOOP ( 'NONE', ( #25918, #24707, #845, #5719 ) ) ;
#19284 = LINE ( 'NONE', #210, #28535 ) ;
#19285 = ORIENTED_EDGE ( 'NONE', *, *, #34210, .F. ) ;
#19286 = CARTESIAN_POINT ( 'NONE',  ( -35.50000000000000000, -113.0140978167138712, -0.3747823525984258497 ) ) ;
#19287 = DIRECTION ( 'NONE',  ( 0.000000000000000000, -0.000000000000000000, 1.000000000000000000 ) ) ;
#19288 = CARTESIAN_POINT ( 'NONE',  ( -38.02454729103296671, -114.3549511594417396, 3.659774454178448710 ) ) ;
#19289 = ADVANCED_FACE ( 'NONE', ( #24248 ), #21510, .T. ) ;
#19290 = DIRECTION ( 'NONE',  ( -1.000000000000000000, -1.836970198721029934E-16, -0.000000000000000000 ) ) ;
#19291 = ORIENTED_EDGE ( 'NONE', *, *, #27810, .F. ) ;
#19292 = CARTESIAN_POINT ( 'NONE',  ( -55.00000000000000000, -2.775557561562891351E-14, 110.0000000000000000 ) ) ;
#19293 = CARTESIAN_POINT ( 'NONE',  ( -35.50000000000000711, -113.3557509229967764, 1.923098431109107054 ) ) ;
#19294 = ORIENTED_EDGE ( 'NONE', *, *, #32404, .F. ) ;
#19295 = VERTEX_POINT ( 'NONE', #5512 ) ;
#19296 = CARTESIAN_POINT ( 'NONE',  ( -39.02454729103295961, -114.7691647218148745, 5.159774454178448266 ) ) ;
#19297 = CIRCLE ( 'NONE', #27374, 20.00000000000000711 ) ;
#19298 = CARTESIAN_POINT ( 'NONE',  ( 0.1085714285714300953, -3.798448662927791819, -0.7999999999999951594 ) ) ;
#19299 = ORIENTED_EDGE ( 'NONE', *, *, #5962, .F. ) ;
#19300 = ORIENTED_EDGE ( 'NONE', *, *, #32651, .F. ) ;
#19301 = CARTESIAN_POINT ( 'NONE',  ( -34.50000000000000000, -115.0140978167138712, -0.3747823525984421145 ) ) ;
#19302 = AXIS2_PLACEMENT_3D ( 'NONE', #17245, #17778, #28251 ) ;
#19303 = CARTESIAN_POINT ( 'NONE',  ( 0.000000000000000000, 10.62435788049461571, -13.16139124467909483 ) ) ;
#19304 = AXIS2_PLACEMENT_3D ( 'NONE', #22219, #16812, #3157 ) ;
#19305 = FACE_OUTER_BOUND ( 'NONE', #10431, .T. ) ;
#19306 = DIRECTION ( 'NONE',  ( -1.000000000000000000, 0.000000000000000000, 0.000000000000000000 ) ) ;
#19307 = CIRCLE ( 'NONE', #33680, 7.199999999999993960 ) ;
#19308 =( REPRESENTATION_RELATIONSHIP ('NONE','NONE', #26607, #31430 ) REPRESENTATION_RELATIONSHIP_WITH_TRANSFORMATION ( #27648 )SHAPE_REPRESENTATION_RELATIONSHIP( ) );
#19309 = CARTESIAN_POINT ( 'NONE',  ( -35.50160444427493189, -113.9929510916434339, 12.65937477241749853 ) ) ;
#19310 = DIRECTION ( 'NONE',  ( 1.000000000000000000, 0.000000000000000000, 0.000000000000000000 ) ) ;
#19311 = DIRECTION ( 'NONE',  ( -1.000000000000000000, -0.000000000000000000, 0.000000000000000000 ) ) ;
#19312 = CARTESIAN_POINT ( 'NONE',  ( -34.50000000000000000, -111.0140821919592327, -0.5779076015960634694 ) ) ;
#19313 = CARTESIAN_POINT ( 'NONE',  ( -35.50000000000000000, -114.1835524127412924, 8.514811007161055656 ) ) ;
#19314 = CARTESIAN_POINT ( 'NONE',  ( 7.999999999999992895, 0.000000000000000000, 0.000000000000000000 ) ) ;
#19315 = CARTESIAN_POINT ( 'NONE',  ( 8.000000000000000000, -14.18878633068154826, -6.236773481718229206 ) ) ;
#19316 = ADVANCED_FACE ( 'NONE', ( #30359 ), #32508, .T. ) ;
#19317 = AXIS2_PLACEMENT_3D ( 'NONE', #21991, #10672, #8496 ) ;
#19318 = EDGE_CURVE ( 'NONE', #7742, #15404, #5169, .T. ) ;
#19319 = DIRECTION ( 'NONE',  ( 0.000000000000000000, -1.000000000000000000, 0.000000000000000000 ) ) ;
#19320 = ORIENTED_EDGE ( 'NONE', *, *, #14942, .F. ) ;
#19321 = CARTESIAN_POINT ( 'NONE',  ( -35.50000000000000711, -114.0185793162512908, 9.502217742515812304 ) ) ;
#19322 = CARTESIAN_POINT ( 'NONE',  ( -0.1717365941144438635, -6.008326913195953800, -0.7999999999999951594 ) ) ;
#19323 =( NAMED_UNIT ( * ) SI_UNIT ( $, .STERADIAN. ) SOLID_ANGLE_UNIT ( ) );
#19324 = DIRECTION ( 'NONE',  ( 5.339440136655842133E-16, 1.000000000000000000, -1.918536189538073087E-16 ) ) ;
#19325 = AXIS2_PLACEMENT_3D ( 'NONE', #17277, #201, #25232 ) ;
#19326 = AXIS2_PLACEMENT_3D ( 'NONE', #26080, #9688, #1411 ) ;
#19327 = DIRECTION ( 'NONE',  ( 1.000000000000000000, 0.000000000000000000, 0.000000000000000000 ) ) ;
#19328 = EDGE_LOOP ( 'NONE', ( #21180, #23377, #25893, #12579, #16142, #11875, #8713, #12135 ) ) ;
#19329 = VECTOR ( 'NONE', #33039, 1000.000000000000000 ) ;
#19330 = LINE ( 'NONE', #5671, #7293 ) ;
#19331 = DIRECTION ( 'NONE',  ( -1.000000000000000000, 0.000000000000000000, 0.000000000000000000 ) ) ;
#19332 = LINE ( 'NONE', #30512, #26893 ) ;
#19333 = CARTESIAN_POINT ( 'NONE',  ( -37.49999999999999289, -11.24969279549607748, 111.5585998451919778 ) ) ;
#19334 = EDGE_CURVE ( 'NONE', #24482, #8803, #35064, .T. ) ;
#19335 = VECTOR ( 'NONE', #26721, 1000.000000000000000 ) ;
#19336 = DIRECTION ( 'NONE',  ( -1.174092375852890260E-15, 4.222049128630259891E-16, 1.000000000000000000 ) ) ;
#19337 = DIRECTION ( 'NONE',  ( -1.000000000000000000, -0.000000000000000000, -0.000000000000000000 ) ) ;
#19338 = VERTEX_POINT ( 'NONE', #11970 ) ;
#19339 = DIRECTION ( 'NONE',  ( 1.000000000000000000, -0.000000000000000000, -0.000000000000000000 ) ) ;
#19340 = DIRECTION ( 'NONE',  ( -1.000000000000000000, 0.000000000000000000, 0.000000000000000000 ) ) ;
#19341 = ORIENTED_EDGE ( 'NONE', *, *, #10593, .F. ) ;
#19342 = CARTESIAN_POINT ( 'NONE',  ( -35.97545270896705460, -114.3549511594417680, 7.090225545821551734 ) ) ;
#19343 = ORIENTED_EDGE ( 'NONE', *, *, #18350, .T. ) ;
#19344 = SURFACE_STYLE_USAGE ( .BOTH. , #451 ) ;
#19345 = AXIS2_PLACEMENT_3D ( 'NONE', #5744, #30580, #5913 ) ;
#19346 = EDGE_LOOP ( 'NONE', ( #11566, #34409, #23129, #3627 ) ) ;
#19347 = ORIENTED_EDGE ( 'NONE', *, *, #11069, .F. ) ;
#19348 = LINE ( 'NONE', #30177, #31551 ) ;
#19349 = AXIS2_PLACEMENT_3D ( 'NONE', #17289, #22517, #34049 ) ;
#19350 = VECTOR ( 'NONE', #12427, 1000.000000000000000 ) ;
#19351 = ADVANCED_FACE ( 'NONE', ( #25661 ), #14302, .T. ) ;
#19352 = VECTOR ( 'NONE', #31252, 1000.000000000000000 ) ;
#19353 = DIRECTION ( 'NONE',  ( 1.000000000000000000, -5.339440136655842133E-16, -1.047965281155519420E-16 ) ) ;
#19354 = AXIS2_PLACEMENT_3D ( 'NONE', #12450, #31179, #28481 ) ;
#19355 = CARTESIAN_POINT ( 'NONE',  ( -35.50000000000000711, -114.1861579685891712, 9.524983039397698192 ) ) ;
#19356 = LINE ( 'NONE', #33060, #21820 ) ;
#19357 = CIRCLE ( 'NONE', #31418, 47.49900000000001654 ) ;
#19358 = CARTESIAN_POINT ( 'NONE',  ( 8.000000000000000000, 0.000000000000000000, 0.000000000000000000 ) ) ;
#19359 = AXIS2_PLACEMENT_3D ( 'NONE', #6681, #17299, #9566 ) ;
#19360 = AXIS2_PLACEMENT_3D ( 'NONE', #6937, #34674, #31428 ) ;
#19361 = LINE ( 'NONE', #16658, #22278 ) ;
#19362 = DIRECTION ( 'NONE',  ( 0.000000000000000000, 0.000000000000000000, 1.000000000000000000 ) ) ;
#19363 = EDGE_CURVE ( 'NONE', #423, #17460, #22937, .T. ) ;
#19364 = ADVANCED_FACE ( 'NONE', ( #6033 ), #14471, .T. ) ;
#19365 = CARTESIAN_POINT ( 'NONE',  ( -55.00000000000000000, -25.98076211353320275, 90.99999999999994316 ) ) ;
#19366 = ADVANCED_FACE ( 'NONE', ( #33934 ), #11604, .T. ) ;
#19367 = CARTESIAN_POINT ( 'NONE',  ( -36.06250000000000711, -115.9929510916434481, 14.11852480586265024 ) ) ;
#19368 = DIRECTION ( 'NONE',  ( -1.000000000000000000, -1.836970198721029934E-16, -0.000000000000000000 ) ) ;
#19369 = CARTESIAN_POINT ( 'NONE',  ( 0.000000000000000000, 13.42368113696682030, 3.975523202428055125 ) ) ;
#19370 = AXIS2_PLACEMENT_3D ( 'NONE', #4483, #35080, #7338 ) ;
#19371 = CARTESIAN_POINT ( 'NONE',  ( 8.000000000000000000, 0.000000000000000000, 4.000000000000000000 ) ) ;
#19372 = DIRECTION ( 'NONE',  ( 1.000000000000000000, 0.000000000000000000, -0.000000000000000000 ) ) ;
#19373 = VECTOR ( 'NONE', #15903, 1000.000000000000000 ) ;
#19374 = DIRECTION ( 'NONE',  ( 0.000000000000000000, 0.4999999999999951150, 0.8660254037844414832 ) ) ;
#19375 = DIRECTION ( 'NONE',  ( -1.000000000000000000, 0.000000000000000000, 0.000000000000000000 ) ) ;
#19376 = VERTEX_POINT ( 'NONE', #20221 ) ;
#19377 = EDGE_CURVE ( 'NONE', #17248, #7480, #14125, .T. ) ;
#19378 = CARTESIAN_POINT ( 'NONE',  ( -36.23083527818512550, -111.9754527089670404, 8.215225545821549957 ) ) ;
#19379 = DIRECTION ( 'NONE',  ( 0.000000000000000000, 0.000000000000000000, 1.000000000000000000 ) ) ;
#19380 = LINE ( 'NONE', #27686, #3285 ) ;
#19381 = CIRCLE ( 'NONE', #5040, 20.00000000000000355 ) ;
#19382 = CARTESIAN_POINT ( 'NONE',  ( -34.49999999999998579, -14.17619866229204106, 93.62476896299857287 ) ) ;
#19383 = EDGE_CURVE ( 'NONE', #6413, #15079, #33853, .T. ) ;
#19384 = ORIENTED_EDGE ( 'NONE', *, *, #31450, .F. ) ;
#19385 = ORIENTED_EDGE ( 'NONE', *, *, #9409, .T. ) ;
#19386 = EDGE_CURVE ( 'NONE', #34028, #32406, #16994, .T. ) ;
#19387 = AXIS2_PLACEMENT_3D ( 'NONE', #8804, #27388, #16729 ) ;
#19388 = DIRECTION ( 'NONE',  ( 0.000000000000000000, 0.000000000000000000, 1.000000000000000000 ) ) ;
#19389 = CARTESIAN_POINT ( 'NONE',  ( 8.000000000000000000, -6.336799421339700977, -16.31134495048491573 ) ) ;
#19390 = VERTEX_POINT ( 'NONE', #13959 ) ;
#19391 = AXIS2_PLACEMENT_3D ( 'NONE', #16087, #27466, #8002 ) ;
#19392 = AXIS2_PLACEMENT_3D ( 'NONE', #2108, #13083, #2289 ) ;
#19393 = ORIENTED_EDGE ( 'NONE', *, *, #12143, .F. ) ;
#19394 = AXIS2_PLACEMENT_3D ( 'NONE', #27992, #3687, #30866 ) ;
#19395 = CARTESIAN_POINT ( 'NONE',  ( 8.000000000000007105, 9.604183132802424083, -1.108880290975567950 ) ) ;
#19396 = CARTESIAN_POINT ( 'NONE',  ( 50.00005079999998969, 3.872983346207420574, -1.000000000000000888 ) ) ;
#19397 = ADVANCED_FACE ( 'NONE', ( #11258 ), #19861, .F. ) ;
#19398 = CYLINDRICAL_SURFACE ( 'NONE', #20187, 9.499000000000000554 ) ;
#19399 = VERTEX_POINT ( 'NONE', #28180 ) ;
#19400 = VERTEX_POINT ( 'NONE', #22576 ) ;
#19401 = CIRCLE ( 'NONE', #2202, 52.00000000000000711 ) ;
#19402 = EDGE_CURVE ( 'NONE', #3377, #32945, #6212, .T. ) ;
#19403 = DIRECTION ( 'NONE',  ( -1.000000000000000000, 0.000000000000000000, 0.000000000000000000 ) ) ;
#19404 = AXIS2_PLACEMENT_3D ( 'NONE', #20143, #11180, #14567 ) ;
#19405 = CARTESIAN_POINT ( 'NONE',  ( -50.00000000000000000, 19.99999999999998934, 110.0000000000000000 ) ) ;
#19406 = EDGE_CURVE ( 'NONE', #16080, #25525, #18331, .T. ) ;
#19407 = ORIENTED_EDGE ( 'NONE', *, *, #6529, .F. ) ;
#19408 = DIRECTION ( 'NONE',  ( 0.000000000000000000, 0.000000000000000000, 1.000000000000000000 ) ) ;
#19409 = CIRCLE ( 'NONE', #6764, 4.000000000000000000 ) ;
#19410 = VECTOR ( 'NONE', #14912, 1000.000000000000000 ) ;
#19411 = CARTESIAN_POINT ( 'NONE',  ( -34.50000000000000000, -115.1770117227680998, -1.611965039240062181 ) ) ;
#19412 = AXIS2_PLACEMENT_3D ( 'NONE', #31840, #26457, #5213 ) ;
#19413 = CARTESIAN_POINT ( 'NONE',  ( -36.12500000000014211, -114.9929510916434339, 14.11852480586264846 ) ) ;
#19414 = EDGE_CURVE ( 'NONE', #15405, #10684, #455, .T. ) ;
#19415 = CARTESIAN_POINT ( 'NONE',  ( -35.50000000000000000, -113.9929510916434339, 10.50625754673587409 ) ) ;
#19416 = DIRECTION ( 'NONE',  ( 0.000000000000000000, -0.8660254037844385966, -0.5000000000000001110 ) ) ;
#19417 = EDGE_CURVE ( 'NONE', #17643, #18383, #30971, .T. ) ;
#19418 = CARTESIAN_POINT ( 'NONE',  ( -34.50300906734827322, -114.9929510916434339, 12.71660600561482468 ) ) ;
#19419 = FACE_OUTER_BOUND ( 'NONE', #28524, .T. ) ;
#19421 = ORIENTED_EDGE ( 'NONE', *, *, #31080, .T. ) ;
#19420 = AXIS2_PLACEMENT_3D ( 'NONE', #26265, #17602, #32020 ) ;
#19422 = DIRECTION ( 'NONE',  ( 0.000000000000000000, 0.000000000000000000, -1.000000000000000000 ) ) ;
#19423 = CYLINDRICAL_SURFACE ( 'NONE', #30213, 47.49900000000001654 ) ;
#19424 = DIRECTION ( 'NONE',  ( 1.000000000000000000, -0.000000000000000000, -0.000000000000000000 ) ) ;
#19425 = FACE_OUTER_BOUND ( 'NONE', #11086, .T. ) ;
#19426 = EDGE_LOOP ( 'NONE', ( #5315, #8945 ) ) ;
#19427 = DIRECTION ( 'NONE',  ( -1.000000000000000000, -0.000000000000000000, 0.000000000000000000 ) ) ;
#19428 = ORIENTED_EDGE ( 'NONE', *, *, #107, .F. ) ;
#19429 = CARTESIAN_POINT ( 'NONE',  ( -34.00000000000000000, -114.0592624029313242, 6.003524454178450043 ) ) ;
#19430 = CARTESIAN_POINT ( 'NONE',  ( -42.49999999999999289, -27.48076211353330578, 101.9999999999999432 ) ) ;
#19431 = CARTESIAN_POINT ( 'NONE',  ( -35.50000000000000711, -114.8057644833805568, -1.624782352598427959 ) ) ;
#19432 = EDGE_CURVE ( 'NONE', #33467, #35153, #17173, .T. ) ;
#19433 = AXIS2_PLACEMENT_3D ( 'NONE', #1680, #7066, #18042 ) ;
#19434 = ORIENTED_EDGE ( 'NONE', *, *, #3703, .T. ) ;
#19435 = ORIENTED_EDGE ( 'NONE', *, *, #11982, .T. ) ;
#19436 = DIRECTION ( 'NONE',  ( -1.000000000000000000, 0.000000000000000000, 0.000000000000000000 ) ) ;
#19437 = CARTESIAN_POINT ( 'NONE',  ( 7.999999999999992895, 9.744342220503382279, 46.48873837489803407 ) ) ;
#19438 = AXIS2_PLACEMENT_3D ( 'NONE', #32045, #7188, #18167 ) ;
#19439 = VERTEX_POINT ( 'NONE', #9086 ) ;
#19440 = AXIS2_PLACEMENT_3D ( 'NONE', #15401, #4279, #27084 ) ;
#19441 = DIRECTION ( 'NONE',  ( 0.000000000000000000, 0.000000000000000000, 1.000000000000000000 ) ) ;
#19442 = DIRECTION ( 'NONE',  ( 1.000000000000000000, 0.000000000000000000, -0.000000000000000000 ) ) ;
#19443 = ORIENTED_EDGE ( 'NONE', *, *, #34135, .T. ) ;
#19444 = ORIENTED_EDGE ( 'NONE', *, *, #13903, .T. ) ;
#19445 = DIRECTION ( 'NONE',  ( -1.000000000000000000, -0.000000000000000000, 0.000000000000000000 ) ) ;
#19446 = EDGE_CURVE ( 'NONE', #9156, #28748, #25480, .T. ) ;
#19447 = CARTESIAN_POINT ( 'NONE',  ( 8.000000000000000000, -4.460989585140847424, -16.92083251265332322 ) ) ;
#19448 = ORIENTED_EDGE ( 'NONE', *, *, #32426, .F. ) ;
#19449 = ORIENTED_EDGE ( 'NONE', *, *, #23108, .F. ) ;
#19450 = CARTESIAN_POINT ( 'NONE',  ( -35.50000000000000000, -113.1451905347060460, 2.905063584339864668 ) ) ;
#19451 = ADVANCED_FACE ( 'NONE', ( #27830 ), #8900, .T. ) ;
#19452 = DIRECTION ( 'NONE',  ( 0.000000000000000000, 0.000000000000000000, 1.000000000000000000 ) ) ;
#19453 = ORIENTED_EDGE ( 'NONE', *, *, #16705, .T. ) ;
#19454 = CARTESIAN_POINT ( 'NONE',  ( -35.50000102263782509, -114.9929510916434339, 12.62466071271731316 ) ) ;
#19455 = CARTESIAN_POINT ( 'NONE',  ( -36.12500000000014211, -113.9929510916434339, 14.11852480586265024 ) ) ;
#19456 = CARTESIAN_POINT ( 'NONE',  ( 0.000000000000000000, 0.000000000000000000, -43.60000000000000142 ) ) ;
#19457 = ADVANCED_FACE ( 'NONE', ( #17348 ), #28350, .T. ) ;
#19458 = AXIS2_PLACEMENT_3D ( 'NONE', #7900, #4700, #13152 ) ;
#19459 = CARTESIAN_POINT ( 'NONE',  ( 0.000000000000000000, 0.000000000000000000, 0.000000000000000000 ) ) ;
#19460 = EDGE_CURVE ( 'NONE', #6849, #11426, #1574, .T. ) ;
#19461 = CARTESIAN_POINT ( 'NONE',  ( -34.50000000000000000, -113.9929510916434339, 11.73841344789270202 ) ) ;
#19462 = CARTESIAN_POINT ( 'NONE',  ( -39.00000000000000711, -114.9929510916434339, 12.17846912687782179 ) ) ;
#19463 = AXIS2_PLACEMENT_3D ( 'NONE', #22762, #11785, #33766 ) ;
#19464 = CARTESIAN_POINT ( 'NONE',  ( -35.50000000000000711, -114.9928438774171582, 10.49113435197128652 ) ) ;
#19465 = AXIS2_PLACEMENT_3D ( 'NONE', #7092, #12502, #34292 ) ;
#19466 = DIRECTION ( 'NONE',  ( 1.000000000000000000, 0.000000000000000000, 0.000000000000000000 ) ) ;
#19467 = VERTEX_POINT ( 'NONE', #32170 ) ;
#19468 = ORIENTED_EDGE ( 'NONE', *, *, #9991, .F. ) ;
#19469 = CARTESIAN_POINT ( 'NONE',  ( 0.000000000000000000, 0.000000000000000000, -39.50000000000000711 ) ) ;
#19470 = CYLINDRICAL_SURFACE ( 'NONE', #12844, 22.00000000000000000 ) ;
#19471 = VERTEX_POINT ( 'NONE', #12196 ) ;
#19472 = CARTESIAN_POINT ( 'NONE',  ( 0.000000000000000000, 18.62763138773855687, 2.494040418455418351 ) ) ;
#19473 = ORIENTED_EDGE ( 'NONE', *, *, #10240, .T. ) ;
#19474 = CARTESIAN_POINT ( 'NONE',  ( -35.50000000000000711, -116.0140978167138712, 0.0002176474015577116276 ) ) ;
#19475 = CARTESIAN_POINT ( 'NONE',  ( -0.2142857142857362840, -10.49781318335649161, 0.000000000000000000 ) ) ;
#19476 = CARTESIAN_POINT ( 'NONE',  ( -38.37230871539094323, -112.5438815906447729, 3.941024454178448710 ) ) ;
#19477 = CARTESIAN_POINT ( 'NONE',  ( 7.999999999999992895, 0.000000000000000000, 0.000000000000000000 ) ) ;
#19478 = VERTEX_POINT ( 'NONE', #23528 ) ;
#19479 = CARTESIAN_POINT ( 'NONE',  ( 7.999999999999992895, 47.49120266317496686, 0.8606222198176832761 ) ) ;
#19480 = CARTESIAN_POINT ( 'NONE',  ( -35.50000000000000000, -117.0108842342086888, -0.7556348869410856040 ) ) ;
#19481 = ORIENTED_EDGE ( 'NONE', *, *, #24454, .T. ) ;
#19482 = VERTEX_POINT ( 'NONE', #12554 ) ;
#19483 = CARTESIAN_POINT ( 'NONE',  ( -34.97545270896703329, -113.2308352781851539, 8.909774454178450043 ) ) ;
#19484 = VECTOR ( 'NONE', #33230, 1000.000000000000000 ) ;
#19485 = DIRECTION ( 'NONE',  ( 1.226634733346697831E-16, 0.9659258262890698665, -0.2588190451025151884 ) ) ;
#19486 = VERTEX_POINT ( 'NONE', #23170 ) ;
#19487 = ORIENTED_EDGE ( 'NONE', *, *, #5094, .T. ) ;
#19488 = CARTESIAN_POINT ( 'NONE',  ( -34.50000000000000000, -114.0000000000000853, 2.000000000000001776 ) ) ;
#19489 = DIRECTION ( 'NONE',  ( 1.000000000000000000, -0.000000000000000000, 0.000000000000000000 ) ) ;
#19490 = EDGE_CURVE ( 'NONE', #30962, #13123, #31628, .T. ) ;
#19491 = DIRECTION ( 'NONE',  ( 0.000000000000000000, 0.000000000000000000, 1.000000000000000000 ) ) ;
#19492 = CARTESIAN_POINT ( 'NONE',  ( -35.50000000000000000, -113.9929510916432207, 10.50625754673563250 ) ) ;
#19493 = DIRECTION ( 'NONE',  ( 0.000000000000000000, 0.000000000000000000, 1.000000000000000000 ) ) ;
#19494 = DIRECTION ( 'NONE',  ( 0.000000000000000000, 0.000000000000000000, -1.000000000000000000 ) ) ;
#19495 = CARTESIAN_POINT ( 'NONE',  ( -34.50000000000000000, -116.0124910254613297, -0.6902086197697608894 ) ) ;
#19496 = CARTESIAN_POINT ( 'NONE',  ( -37.98325232167028531, -115.9929510916434481, 14.04194344061727584 ) ) ;
#19497 = DIRECTION ( 'NONE',  ( -1.000000000000000000, 0.000000000000000000, 0.000000000000000000 ) ) ;
#19498 = DIRECTION ( 'NONE',  ( 0.000000000000000000, 0.000000000000000000, 1.000000000000000000 ) ) ;
#19499 = ORIENTED_EDGE ( 'NONE', *, *, #13327, .F. ) ;
#19500 = VECTOR ( 'NONE', #27837, 1000.000000000000000 ) ;
#19501 = CARTESIAN_POINT ( 'NONE',  ( 75.00000000000001421, -25.99649394950417047, 81.00003093645244689 ) ) ;
#19502 = FACE_OUTER_BOUND ( 'NONE', #13889, .T. ) ;
#19503 = CARTESIAN_POINT ( 'NONE',  ( 0.000000000000000000, 8.725776631572825792, 3.753907720749072308 ) ) ;
#19504 = ORIENTED_EDGE ( 'NONE', *, *, #2300, .F. ) ;
#19505 = AXIS2_PLACEMENT_3D ( 'NONE', #6605, #28762, #34166 ) ;
#19506 = CARTESIAN_POINT ( 'NONE',  ( 50.00000000000000000, 0.000000000000000000, 61.99999999999999289 ) ) ;
#19507 = DIRECTION ( 'NONE',  ( 0.000000000000000000, 0.000000000000000000, -1.000000000000000000 ) ) ;
#19508 = CARTESIAN_POINT ( 'NONE',  ( -55.00000000000000000, 7.347880794884119736E-16, 76.00000000000001421 ) ) ;
#19509 = CARTESIAN_POINT ( 'NONE',  ( -35.00000000000000000, -114.0000000000003411, 9.500000000000035527 ) ) ;
#19510 = VECTOR ( 'NONE', #29584, 1000.000000000000000 ) ;
#19511 = DIRECTION ( 'NONE',  ( 1.000000000000000000, -4.607758420995283758E-15, -1.196244974681468005E-15 ) ) ;
#19512 = LINE ( 'NONE', #22390, #32576 ) ;
#19513 = ORIENTED_EDGE ( 'NONE', *, *, #27912, .F. ) ;
#19514 = DIRECTION ( 'NONE',  ( 0.000000000000000000, 0.000000000000000000, -1.000000000000000000 ) ) ;
#19515 = FACE_OUTER_BOUND ( 'NONE', #21057, .T. ) ;
#19516 = VERTEX_POINT ( 'NONE', #12735 ) ;
#19517 = CARTESIAN_POINT ( 'NONE',  ( -36.52652403469559061, -114.9754527089670262, 4.277725545821552622 ) ) ;
#19518 = VERTEX_POINT ( 'NONE', #23710 ) ;
#19519 = EDGE_LOOP ( 'NONE', ( #29864, #5118, #20832, #24447 ) ) ;
#19520 = ORIENTED_EDGE ( 'NONE', *, *, #23938, .T. ) ;
#19521 = DIRECTION ( 'NONE',  ( 0.000000000000000000, 0.000000000000000000, 1.000000000000000000 ) ) ;
#19522 = ADVANCED_FACE ( 'NONE', ( #26062 ), #1752, .F. ) ;
#19523 = CARTESIAN_POINT ( 'NONE',  ( -35.50000000000000711, -113.1807644833805426, -1.624782352598427959 ) ) ;
#19524 = CARTESIAN_POINT ( 'NONE',  ( 0.000000000000000000, -2.710505431213761085E-17, -30.90000000000000568 ) ) ;
#19525 = CARTESIAN_POINT ( 'NONE',  ( -35.50000000000000711, -114.9656200615856818, 10.26631071845107179 ) ) ;
#19526 = CARTESIAN_POINT ( 'NONE',  ( -34.49999999999998579, -14.67619866229204284, 104.0227405789415371 ) ) ;
#19527 = ADVANCED_FACE ( 'NONE', ( #34523 ), #9840, .F. ) ;
#19528 = AXIS2_PLACEMENT_3D ( 'NONE', #3906, #19886, #22596 ) ;
#19529 = DIRECTION ( 'NONE',  ( -1.000000000000000000, -0.000000000000000000, -0.000000000000000000 ) ) ;
#19530 = DIRECTION ( 'NONE',  ( -1.000000000000000000, 0.000000000000000000, 0.000000000000000000 ) ) ;
#19531 = CARTESIAN_POINT ( 'NONE',  ( -34.50000000000000000, -114.1152303497977414, 9.513755561829650986 ) ) ;
#19532 = DIRECTION ( 'NONE',  ( -1.000000000000000000, -0.000000000000000000, 0.000000000000000000 ) ) ;
#19533 = DIRECTION ( 'NONE',  ( 0.000000000000000000, -1.000000000000000000, -1.049160758270772931E-14 ) ) ;
#19534 = CARTESIAN_POINT ( 'NONE',  ( -35.95093014754292682, -115.9929510916434481, 14.11777216781842625 ) ) ;
#19535 = CYLINDRICAL_SURFACE ( 'NONE', #7331, 4.000000000000000000 ) ;
#19536 = DIRECTION ( 'NONE',  ( 0.000000000000000000, -0.5000000000000068834, 0.8660254037844347108 ) ) ;
#19537 = FACE_OUTER_BOUND ( 'NONE', #8933, .T. ) ;
#19538 = FACE_OUTER_BOUND ( 'NONE', #5321, .T. ) ;
#19539 = CARTESIAN_POINT ( 'NONE',  ( 0.000000000000000000, 0.000000000000000000, -55.00000000000000000 ) ) ;
#19540 =( LENGTH_UNIT ( ) NAMED_UNIT ( * ) SI_UNIT ( .MILLI., .METRE. ) );
#19541 = EDGE_LOOP ( 'NONE', ( #19980, #919, #32728, #2632 ) ) ;
#19542 = AXIS2_PLACEMENT_3D ( 'NONE', #7454, #23851, #13232 ) ;
#19543 = CARTESIAN_POINT ( 'NONE',  ( -38.45611840935523418, -112.6276912846090568, 6.433975545821550845 ) ) ;
#19544 = DIRECTION ( 'NONE',  ( 1.000000000000000000, 0.000000000000000000, -1.691777834109590845E-31 ) ) ;
#19545 = CARTESIAN_POINT ( 'NONE',  ( -34.49999999999998579, -25.01350700525237514, 84.74619386235816876 ) ) ;
#19546 = ADVANCED_FACE ( 'NONE', ( #6963 ), #21179, .T. ) ;
#19547 = LINE ( 'NONE', #20072, #9629 ) ;
#19548 = ORIENTED_EDGE ( 'NONE', *, *, #11056, .T. ) ;
#19549 = EDGE_LOOP ( 'NONE', ( #28652, #20839, #32017, #2114 ) ) ;
#19550 = CARTESIAN_POINT ( 'NONE',  ( 1.599999999999990319, 0.000000000000000000, 0.000000000000000000 ) ) ;
#19551 = DIRECTION ( 'NONE',  ( 0.000000000000000000, 0.000000000000000000, 1.000000000000000000 ) ) ;
#19552 = ORIENTED_EDGE ( 'NONE', *, *, #32795, .F. ) ;
#19553 = ORIENTED_EDGE ( 'NONE', *, *, #2077, .T. ) ;
#19554 = VECTOR ( 'NONE', #8350, 1000.000000000000000 ) ;
#19555 = VECTOR ( 'NONE', #30257, 1000.000000000000000 ) ;
#19556 = ADVANCED_FACE ( 'NONE', ( #28583 ), #29299, .T. ) ;
#19557 = CARTESIAN_POINT ( 'NONE',  ( 7.999999999999992895, -46.19362259308826424, -8.585149169758999221 ) ) ;
#19558 = EDGE_CURVE ( 'NONE', #2086, #17954, #14898, .T. ) ;
#19559 = CARTESIAN_POINT ( 'NONE',  ( 55.00000000000000711, -25.98076211353320986, 84.99999999999994316 ) ) ;
#19560 = EDGE_CURVE ( 'NONE', #34584, #17460, #27578, .T. ) ;
#19561 = LINE ( 'NONE', #316, #32843 ) ;
#19562 = ORIENTED_EDGE ( 'NONE', *, *, #26966, .F. ) ;
#19563 = ORIENTED_EDGE ( 'NONE', *, *, #10563, .T. ) ;
#19564 = DIRECTION ( 'NONE',  ( -0.000000000000000000, 0.000000000000000000, -1.000000000000000000 ) ) ;
#19565 = EDGE_CURVE ( 'NONE', #18178, #24515, #18944, .T. ) ;
#19566 = CARTESIAN_POINT ( 'NONE',  ( -39.49999999999999289, -14.67619866229204284, 93.25874355921412473 ) ) ;
#19567 = ORIENTED_EDGE ( 'NONE', *, *, #4481, .T. ) ;
#19568 = DIRECTION ( 'NONE',  ( 1.000000000000000000, 0.000000000000000000, 0.000000000000000000 ) ) ;
#19569 = EDGE_CURVE ( 'NONE', #24798, #16647, #21791, .T. ) ;
#19570 = CARTESIAN_POINT ( 'NONE',  ( -34.49999999999998579, -25.98076211353322051, 84.99999999999992895 ) ) ;
#19571 = CARTESIAN_POINT ( 'NONE',  ( -36.15625000000007816, -114.9929510916434339, 14.11852480586264846 ) ) ;
#19572 = DIRECTION ( 'NONE',  ( 0.000000000000000000, 0.000000000000000000, 1.000000000000000000 ) ) ;
#19573 = CARTESIAN_POINT ( 'NONE',  ( -36.49999999999999289, -4.676198662292047281, 104.0227405789415798 ) ) ;
#19574 = AXIS2_PLACEMENT_3D ( 'NONE', #33169, #21459, #5635 ) ;
#19575 = CARTESIAN_POINT ( 'NONE',  ( -36.50000000000011369, -114.9929510916434339, 14.11852480586264846 ) ) ;
#19577 = DIRECTION ( 'NONE',  ( -1.000000000000000000, 0.000000000000000000, 0.000000000000000000 ) ) ;
#19576 = VECTOR ( 'NONE', #24334, 1000.000000000000000 ) ;
#19578 = DIRECTION ( 'NONE',  ( -1.000000000000000000, -0.000000000000000000, -0.000000000000000000 ) ) ;
#19579 = AXIS2_PLACEMENT_3D ( 'NONE', #1970, #9876, #2340 ) ;
#19580 = DIRECTION ( 'NONE',  ( -1.000000000000000000, -1.836970198721029934E-16, -0.000000000000000000 ) ) ;
#19581 = DIRECTION ( 'NONE',  ( 1.000000000000000000, -4.524158825347490025E-15, -1.169797080839617330E-15 ) ) ;
#19582 = CARTESIAN_POINT ( 'NONE',  ( 3.872983346207489852, 0.9999999999999522604, -40.00000000000000000 ) ) ;
#19583 = ORIENTED_EDGE ( 'NONE', *, *, #18291, .F. ) ;
#19584 = CARTESIAN_POINT ( 'NONE',  ( 0.000000000000000000, 0.000000000000000000, 11.00000000000000000 ) ) ;
#19585 = ORIENTED_EDGE ( 'NONE', *, *, #22765, .F. ) ;
#19586 = CARTESIAN_POINT ( 'NONE',  ( -38.18337828418795965, -110.9754527089670546, 5.534774454178449155 ) ) ;
#19587 = DIRECTION ( 'NONE',  ( -1.000000000000000000, 0.000000000000000000, -0.000000000000000000 ) ) ;
#19588 = ADVANCED_FACE ( 'NONE', ( #4286 ), #15226, .T. ) ;
#19589 = CARTESIAN_POINT ( 'NONE',  ( -35.50000000000000711, -115.0468226098135744, -1.624774171496087716 ) ) ;
#19590 = VERTEX_POINT ( 'NONE', #34164 ) ;
#19591 = ORIENTED_EDGE ( 'NONE', *, *, #11371, .T. ) ;
#19592 = DIRECTION ( 'NONE',  ( 1.000000000000000000, -0.000000000000000000, -0.000000000000000000 ) ) ;
#19593 = ADVANCED_FACE ( 'NONE', ( #4469 ), #15407, .T. ) ;
#19594 = DIRECTION ( 'NONE',  ( -1.000000000000000000, 0.000000000000000000, 0.000000000000000000 ) ) ;
#19595 = AXIS2_PLACEMENT_3D ( 'NONE', #7333, #4475, #12915 ) ;
#19596 = VERTEX_POINT ( 'NONE', #20445 ) ;
#19597 = CARTESIAN_POINT ( 'NONE',  ( -3.799999999999999822, 4.653657836759942730E-16, -32.00000000000000000 ) ) ;
#19598 = EDGE_CURVE ( 'NONE', #13434, #34100, #22944, .T. ) ;
#19599 = FACE_OUTER_BOUND ( 'NONE', #22009, .T. ) ;
#19600 = ORIENTED_EDGE ( 'NONE', *, *, #25166, .F. ) ;
#19601 = VERTEX_POINT ( 'NONE', #15580 ) ;
#19602 = EDGE_CURVE ( 'NONE', #8628, #5884, #22375, .T. ) ;
#19603 = DIRECTION ( 'NONE',  ( 0.000000000000000000, 0.000000000000000000, 1.000000000000000000 ) ) ;
#19604 = EDGE_CURVE ( 'NONE', #30986, #1640, #4991, .T. ) ;
#19605 = AXIS2_PLACEMENT_3D ( 'NONE', #31532, #26496, #26130 ) ;
#19606 = CARTESIAN_POINT ( 'NONE',  ( 0.000000000000000000, 12.96676809804150565, 13.60411018104323411 ) ) ;
#19607 = EDGE_LOOP ( 'NONE', ( #22509, #33691, #7449, #15298 ) ) ;
#19608 = EDGE_LOOP ( 'NONE', ( #24178, #33160 ) ) ;
#19609 = CARTESIAN_POINT ( 'NONE',  ( -35.50000000000000000, -111.6790780953339066, 2.383953864837686343 ) ) ;
#19610 = PRODUCT_DEFINITION_SHAPE ( 'NONE', 'NONE',  #35647 ) ;
#19611 = EDGE_LOOP ( 'NONE', ( #5017, #20551, #17381, #13597, #17713, #2585, #18647, #1472, #30040, #28037, #21706, #11397, #1085, #26548, #25473, #17475 ) ) ;
#19612 = CARTESIAN_POINT ( 'NONE',  ( -35.50000000000000711, -114.9929510916434339, 12.44250253426871033 ) ) ;
#19613 = EDGE_CURVE ( 'NONE', #23209, #21050, #24689, .T. ) ;
#19614 = CARTESIAN_POINT ( 'NONE',  ( -35.97545865737298953, -113.9929510916434339, 14.11837420659365527 ) ) ;
#19615 = DIRECTION ( 'NONE',  ( -1.000000000000000000, 0.000000000000000000, 0.000000000000000000 ) ) ;
#19616 = FACE_OUTER_BOUND ( 'NONE', #16867, .T. ) ;
#19617 = CARTESIAN_POINT ( 'NONE',  ( -34.49999793727135966, -113.9929510916434339, 12.61164896875036767 ) ) ;
#19618 = CARTESIAN_POINT ( 'NONE',  ( -34.49999999999998579, -12.06135120645816627, 83.49999999999992895 ) ) ;
#19619 = CARTESIAN_POINT ( 'NONE',  ( -35.50000000000000711, -114.9929510916434339, 11.73841344789270202 ) ) ;
#19620 = CYLINDRICAL_SURFACE ( 'NONE', #23368, 15.49899999999998457 ) ;
#19621 = DIRECTION ( 'NONE',  ( -1.174092375852890260E-15, 4.222049128630259891E-16, 1.000000000000000000 ) ) ;
#19622 = ORIENTED_EDGE ( 'NONE', *, *, #15581, .F. ) ;
#19623 = VERTEX_POINT ( 'NONE', #16119 ) ;
#19624 = AXIS2_PLACEMENT_3D ( 'NONE', #26693, #31893, #9931 ) ;
#19625 = DIRECTION ( 'NONE',  ( 1.000000000000000000, -5.339440136655842133E-16, -1.047965281155519420E-16 ) ) ;
#19626 = AXIS2_PLACEMENT_3D ( 'NONE', #3562, #17570, #12192 ) ;
#19627 = DIRECTION ( 'NONE',  ( 0.000000000000000000, 0.000000000000000000, 1.000000000000000000 ) ) ;
#19628 = EDGE_CURVE ( 'NONE', #10539, #18156, #35240, .T. ) ;
#19629 = EDGE_LOOP ( 'NONE', ( #21010, #1979 ) ) ;
#19630 = DIRECTION ( 'NONE',  ( -1.000000000000000000, 0.000000000000000000, 0.000000000000000000 ) ) ;
#19631 = ORIENTED_EDGE ( 'NONE', *, *, #8352, .F. ) ;
#19632 = CARTESIAN_POINT ( 'NONE',  ( -35.50000000000000000, -113.6807644833805995, -0.6247823525984269599 ) ) ;
#19633 = EDGE_CURVE ( 'NONE', #24757, #12141, #7497, .T. ) ;
#19634 = CARTESIAN_POINT ( 'NONE',  ( -35.00000000000000000, -114.0592624029313242, 6.003524454178450043 ) ) ;
#19635 = ORIENTED_EDGE ( 'NONE', *, *, #6021, .T. ) ;
#19636 = FACE_OUTER_BOUND ( 'NONE', #18646, .T. ) ;
#19637 = VERTEX_POINT ( 'NONE', #35413 ) ;
#19638 = AXIS2_PLACEMENT_3D ( 'NONE', #5232, #8082, #18359 ) ;
#19639 = CARTESIAN_POINT ( 'NONE',  ( -39.49999999999999289, -4.633167542791596816, 143.9590043477703887 ) ) ;
#19640 = CARTESIAN_POINT ( 'NONE',  ( -35.50000000000000000, -117.0140978167138854, -0.4685323525984309012 ) ) ;
#19641 = VERTEX_POINT ( 'NONE', #32882 ) ;
#19642 = ORIENTED_EDGE ( 'NONE', *, *, #8200, .T. ) ;
#19643 = EDGE_CURVE ( 'NONE', #9129, #11554, #20646, .T. ) ;
#19644 = CARTESIAN_POINT ( 'NONE',  ( -36.94073759706868287, -112.0000000000000142, 5.628524454178449155 ) ) ;
#19645 = ADVANCED_FACE ( 'NONE', ( #32706 ), #13795, .T. ) ;
#19646 = CYLINDRICAL_SURFACE ( 'NONE', #18983, 10.49999999999999645 ) ;
#19647 = ORIENTED_EDGE ( 'NONE', *, *, #6555, .F. ) ;
#19648 = ORIENTED_EDGE ( 'NONE', *, *, #13427, .F. ) ;
#19649 = CARTESIAN_POINT ( 'NONE',  ( -34.50000000000000000, -115.0140978167138712, 0.8752176474015623819 ) ) ;
#19650 = CARTESIAN_POINT ( 'NONE',  ( -0.1374368770859779598, -4.808326913195978491, -0.7999999999999951594 ) ) ;
#19651 = ORIENTED_EDGE ( 'NONE', *, *, #7348, .T. ) ;
#19652 = CIRCLE ( 'NONE', #21955, 14.00000000000000000 ) ;
#19653 = FACE_OUTER_BOUND ( 'NONE', #9577, .T. ) ;
#19654 = CARTESIAN_POINT ( 'NONE',  ( -35.50040135968784938, -113.9929510916434339, 12.63896776382214071 ) ) ;
#19655 = CARTESIAN_POINT ( 'NONE',  ( 0.000000000000000000, 0.000000000000000000, 0.000000000000000000 ) ) ;
#19656 = DIRECTION ( 'NONE',  ( 0.000000000000000000, 0.000000000000000000, -1.000000000000000000 ) ) ;
#19657 = CARTESIAN_POINT ( 'NONE',  ( -34.50000000000000000, -116.0140978167138712, 0.3752176474015736507 ) ) ;
#19658 = CARTESIAN_POINT ( 'NONE',  ( -35.50000000000000000, -114.2183886307118428, 8.518969274377507617 ) ) ;
#19659 = DIRECTION ( 'NONE',  ( 1.783119874454246424E-31, 1.187911941725854497E-31, -1.000000000000000000 ) ) ;
#19660 = CIRCLE ( 'NONE', #16217, 0.9999999999999974465 ) ;
#19661 = FACE_OUTER_BOUND ( 'NONE', #7537, .T. ) ;
#19662 = ORIENTED_EDGE ( 'NONE', *, *, #3532, .F. ) ;
#19663 = CARTESIAN_POINT ( 'NONE',  ( 7.999999999999992895, 0.000000000000000000, 0.000000000000000000 ) ) ;
#19664 = DIRECTION ( 'NONE',  ( 0.000000000000000000, 0.000000000000000000, -1.000000000000000000 ) ) ;
#19665 = FACE_OUTER_BOUND ( 'NONE', #11809, .T. ) ;
#19666 = EDGE_CURVE ( 'NONE', #2565, #28758, #29838, .T. ) ;
#19667 = ORIENTED_EDGE ( 'NONE', *, *, #8110, .T. ) ;
#19668 = DIRECTION ( 'NONE',  ( 1.000000000000000000, -0.000000000000000000, -0.000000000000000000 ) ) ;
#19669 = DIRECTION ( 'NONE',  ( 0.000000000000000000, 0.000000000000000000, -1.000000000000000000 ) ) ;
#19670 = EDGE_CURVE ( 'NONE', #2896, #19816, #9750, .T. ) ;
#19671 = CIRCLE ( 'NONE', #5350, 6.000000000000005329 ) ;
#19672 = FACE_OUTER_BOUND ( 'NONE', #2948, .T. ) ;
#19673 = FACE_OUTER_BOUND ( 'NONE', #24669, .T. ) ;
#19674 = AXIS2_PLACEMENT_3D ( 'NONE', #34655, #1522, #18252 ) ;
#19675 = DIRECTION ( 'NONE',  ( -1.000000000000000000, 0.000000000000000000, 0.000000000000000000 ) ) ;
#19676 = DIRECTION ( 'NONE',  ( -1.000000000000000000, 0.000000000000000000, 0.000000000000000000 ) ) ;
#19677 = VERTEX_POINT ( 'NONE', #8032 ) ;
#19678 = CARTESIAN_POINT ( 'NONE',  ( 5.400000000000071410, 0.9999999999999662492, -40.00000000000000000 ) ) ;
#19679 = LINE ( 'NONE', #22927, #25758 ) ;
#19680 = CARTESIAN_POINT ( 'NONE',  ( 7.999999999999992895, -44.75336757549789013, 14.30704879393590545 ) ) ;
#19681 = VERTEX_POINT ( 'NONE', #15759 ) ;
#19682 = CARTESIAN_POINT ( 'NONE',  ( -37.47347596530441649, -113.0245472910329880, 3.527725545821551734 ) ) ;
#19683 = EDGE_LOOP ( 'NONE', ( #14761, #21913 ) ) ;
#19685 = ORIENTED_EDGE ( 'NONE', *, *, #20121, .T. ) ;
#19684 = VECTOR ( 'NONE', #12840, 1000.000000000000000 ) ;
#19686 = VERTEX_POINT ( 'NONE', #11098 ) ;
#19687 = DIRECTION ( 'NONE',  ( -1.783119874454246424E-31, -1.187911941725854497E-31, 1.000000000000000000 ) ) ;
#19688 = AXIS2_PLACEMENT_3D ( 'NONE', #14656, #33577, #33406 ) ;
#19689 = CARTESIAN_POINT ( 'NONE',  ( -35.50000000000000711, -116.0140978167138712, 0.6252176474015648244 ) ) ;
#19690 = FACE_OUTER_BOUND ( 'NONE', #619, .T. ) ;
#19691 = CARTESIAN_POINT ( 'NONE',  ( -35.50000000000000711, -114.2305202833893816, 9.534416457224700991 ) ) ;
#19692 = AXIS2_PLACEMENT_3D ( 'NONE', #20509, #3983, #14927 ) ;
#19693 = CARTESIAN_POINT ( 'NONE',  ( 7.999999999999992895, 35.20873326984081331, 31.88259874184044662 ) ) ;
#19694 = CIRCLE ( 'NONE', #28932, 4.800000000000000711 ) ;
#19695 = CARTESIAN_POINT ( 'NONE',  ( 0.000000000000000000, -4.460989585140847424, -16.92083251265332322 ) ) ;
#19696 = CARTESIAN_POINT ( 'NONE',  ( -34.50000000000000000, -114.9929510916434339, 10.51725893871048889 ) ) ;
#19697 = CARTESIAN_POINT ( 'NONE',  ( 0.000000000000000000, 42.60732521687570795, 19.80331771201672453 ) ) ;
#19698 = FACE_BOUND ( 'NONE', #30264, .T. ) ;
#19699 = CARTESIAN_POINT ( 'NONE',  ( -35.50000000000000000, -115.1342778146718473, 8.846135899190283425 ) ) ;
#19700 = CARTESIAN_POINT ( 'NONE',  ( -35.50000000000000711, -112.1859307030124739, 1.448610958621386224 ) ) ;
#19701 = DIRECTION ( 'NONE',  ( -1.000000000000000000, -0.000000000000000000, -0.000000000000000000 ) ) ;
#19702 = AXIS2_PLACEMENT_3D ( 'NONE', #20496, #1621, #7541 ) ;
#19703 = CIRCLE ( 'NONE', #765, 19.99999999999998579 ) ;
#19704 = LINE ( 'NONE', #20415, #22217 ) ;
#19705 = CARTESIAN_POINT ( 'NONE',  ( 0.000000000000000000, 0.000000000000000000, 0.000000000000000000 ) ) ;
#19706 = ADVANCED_FACE ( 'NONE', ( #10922, #21517 ), #19186, .F. ) ;
#19707 = PLANE ( 'NONE',  #21639 ) ;
#19708 = DIRECTION ( 'NONE',  ( -1.000000000000000000, 0.000000000000000000, 0.000000000000000000 ) ) ;
#19709 = ORIENTED_EDGE ( 'NONE', *, *, #30788, .T. ) ;
#19710 = CARTESIAN_POINT ( 'NONE',  ( -36.94073759706868287, -115.0000000000000000, 2.871475545821551290 ) ) ;
#19711 = LINE ( 'NONE', #30726, #880 ) ;
#19712 = CARTESIAN_POINT ( 'NONE',  ( -4.000000000000000000, 0.000000000000000000, 49.10000000000000142 ) ) ;
#19713 = DIRECTION ( 'NONE',  ( -1.000000000000000000, 0.000000000000000000, 0.000000000000000000 ) ) ;
#19714 = ORIENTED_EDGE ( 'NONE', *, *, #7577, .F. ) ;
#19715 = ORIENTED_EDGE ( 'NONE', *, *, #26955, .T. ) ;
#19716 = UNCERTAINTY_MEASURE_WITH_UNIT (LENGTH_MEASURE( 1.000000000000000082E-05 ), #26510, 'distance_accuracy_value', 'NONE');
#19717 = APPLICATION_CONTEXT ( 'automotive_design' ) ;
#19718 = AXIS2_PLACEMENT_3D ( 'NONE', #24882, #11192, #22515 ) ;
#19719 = DIRECTION ( 'NONE',  ( 1.000000000000000000, -4.607758420995283758E-15, -1.174092375852883160E-15 ) ) ;
#19720 = AXIS2_PLACEMENT_3D ( 'NONE', #31289, #14708, #15062 ) ;
#19721 = CARTESIAN_POINT ( 'NONE',  ( 0.000000000000000000, 9.604183132802452505, 5.908880290975567995 ) ) ;
#19722 = ORIENTED_EDGE ( 'NONE', *, *, #4659, .F. ) ;
#19723 = EDGE_CURVE ( 'NONE', #1815, #15127, #23522, .T. ) ;
#19724 = ORIENTED_EDGE ( 'NONE', *, *, #21736, .F. ) ;
#19725 = DIRECTION ( 'NONE',  ( -1.000000000000000000, -0.000000000000000000, -0.000000000000000000 ) ) ;
#19726 = APPLICATION_PROTOCOL_DEFINITION ( 'draft international standard', 'automotive_design', 1998, #35176 ) ;
#19727 = FACE_OUTER_BOUND ( 'NONE', #12482, .T. ) ;
#19728 = VERTEX_POINT ( 'NONE', #30013 ) ;
#19729 = ORIENTED_EDGE ( 'NONE', *, *, #4438, .F. ) ;
#19730 = AXIS2_PLACEMENT_3D ( 'NONE', #29656, #8872, #11410 ) ;
#19731 = CARTESIAN_POINT ( 'NONE',  ( 8.000000000000007105, 7.613867765417669631, 5.679790370316101011 ) ) ;
#19732 = CARTESIAN_POINT ( 'NONE',  ( -42.49999999999999289, -12.00833024919776371, 94.79903810567661537 ) ) ;
#19733 = ORIENTED_EDGE ( 'NONE', *, *, #8119, .F. ) ;
#19734 = DIRECTION ( 'NONE',  ( 1.000000000000000000, -0.000000000000000000, -0.000000000000000000 ) ) ;
#19735 = CARTESIAN_POINT ( 'NONE',  ( -34.50000000000000000, -115.0140978167138712, 0.8752176474015623819 ) ) ;
#19736 = CARTESIAN_POINT ( 'NONE',  ( 0.000000000000000000, 5.908880290975762506, -9.604183132802354805 ) ) ;
#19737 = DIRECTION ( 'NONE',  ( 0.000000000000000000, -1.000000000000000000, 0.000000000000000000 ) ) ;
#19738 = AXIS2_PLACEMENT_3D ( 'NONE', #29373, #12982, #32948 ) ;
#19739 = CARTESIAN_POINT ( 'NONE',  ( -34.50000000000000000, -115.9929081983957104, 10.49113315946066294 ) ) ;
#19740 = AXIS2_PLACEMENT_3D ( 'NONE', #32131, #1712, #7461 ) ;
#19741 = DIRECTION ( 'NONE',  ( 0.000000000000000000, -1.000000000000000000, 0.000000000000000000 ) ) ;
#19742 = CARTESIAN_POINT ( 'NONE',  ( 0.000000000000000000, 0.000000000000000000, 0.000000000000000000 ) ) ;
#19743 = CARTESIAN_POINT ( 'NONE',  ( -37.42187499999997158, -114.9929510916434339, 14.11852480586264846 ) ) ;
#19744 = CARTESIAN_POINT ( 'NONE',  ( 7.999999999999992895, 36.34385289850631295, -29.77717097092039111 ) ) ;
#19745 = DIRECTION ( 'NONE',  ( -1.000000000000000000, 0.000000000000000000, 0.000000000000000000 ) ) ;
#19746 = DIRECTION ( 'NONE',  ( -1.000000000000000000, 0.000000000000000000, 0.000000000000000000 ) ) ;
#19747 = DIRECTION ( 'NONE',  ( 0.000000000000000000, -6.983129352544641692E-15, 1.000000000000000000 ) ) ;
#19748 = ADVANCED_FACE ( 'NONE', ( #109 ), #21891, .T. ) ;
#19749 = ORIENTED_EDGE ( 'NONE', *, *, #35217, .T. ) ;
#19750 = ADVANCED_FACE ( 'NONE', ( #2127 ), #24087, .T. ) ;
#19751 = CARTESIAN_POINT ( 'NONE',  ( 70.00000000000001421, -37.13120097615721704, 79.35042362907756797 ) ) ;
#19752 = VERTEX_POINT ( 'NONE', #8207 ) ;
#19753 = CARTESIAN_POINT ( 'NONE',  ( -34.02454729103298092, -115.3019030900506294, 6.097274454178449155 ) ) ;
#19754 = CARTESIAN_POINT ( 'NONE',  ( -90.00000000000002842, -4.694161725993254197E-16, -6.765000000000038760 ) ) ;
#19755 = CARTESIAN_POINT ( 'NONE',  ( -35.50000000000000711, -112.0157046079661995, -0.6902086197697556713 ) ) ;
#19756 = ORIENTED_EDGE ( 'NONE', *, *, #28725, .T. ) ;
#19757 = EDGE_LOOP ( 'NONE', ( #2194, #26333, #4632, #34929 ) ) ;
#19758 = LINE ( 'NONE', #1070, #3356 ) ;
#19759 = DIRECTION ( 'NONE',  ( -1.000000000000000000, 0.000000000000000000, 0.000000000000000000 ) ) ;
#19760 = EDGE_CURVE ( 'NONE', #12141, #4193, #28131, .T. ) ;
#19761 = VERTEX_POINT ( 'NONE', #10393 ) ;
#19762 =( REPRESENTATION_RELATIONSHIP ('NONE','NONE', #26607, #31430 ) REPRESENTATION_RELATIONSHIP_WITH_TRANSFORMATION ( #25284 )SHAPE_REPRESENTATION_RELATIONSHIP( ) );
#19763 = CARTESIAN_POINT ( 'NONE',  ( 0.000000000000000000, 0.000000000000000000, 0.000000000000000000 ) ) ;
#19764 = AXIS2_PLACEMENT_3D ( 'NONE', #8055, #5021, #15606 ) ;
#19765 = FACE_OUTER_BOUND ( 'NONE', #9039, .T. ) ;
#19766 = AXIS2_PLACEMENT_3D ( 'NONE', #10702, #27273, #16622 ) ;
#19767 = VERTEX_POINT ( 'NONE', #29652 ) ;
#19768 = ORIENTED_EDGE ( 'NONE', *, *, #18842, .T. ) ;
#19769 = DIRECTION ( 'NONE',  ( 0.000000000000000000, 0.7535859266250380939, 0.6573494133204066392 ) ) ;
#19770 = CYLINDRICAL_SURFACE ( 'NONE', #15011, 0.5000000000000004441 ) ;
#19771 = ORIENTED_EDGE ( 'NONE', *, *, #28656, .F. ) ;
#19772 = ORIENTED_EDGE ( 'NONE', *, *, #23228, .T. ) ;
#19773 = CARTESIAN_POINT ( 'NONE',  ( -35.50000000000000000, -112.8115600290184801, 2.865251044451027074 ) ) ;
#19774 = ADVANCED_BREP_SHAPE_REPRESENTATION ( '', ( #22590, #21307 ), #32842 ) ;
#19775 = ORIENTED_EDGE ( 'NONE', *, *, #3862, .F. ) ;
#19776 = CARTESIAN_POINT ( 'NONE',  ( -35.50000000000000711, -114.9929510916434339, 12.17846912687782712 ) ) ;
#19777 = EDGE_CURVE ( 'NONE', #574, #23561, #15458, .T. ) ;
#19778 = CARTESIAN_POINT ( 'NONE',  ( -38.99699093265172678, -113.9929510916434339, 12.71660600561481402 ) ) ;
#19779 = PLANE ( 'NONE',  #33785 ) ;
#19780 = CARTESIAN_POINT ( 'NONE',  ( -21.15833593587365513, -16.18172400785637777, 71.02756813566458050 ) ) ;
#19781 = CARTESIAN_POINT ( 'NONE',  ( -34.50000000000000000, -113.9929510916434339, 10.72628538622835670 ) ) ;
#19782 = CARTESIAN_POINT ( 'NONE',  ( 1.479000000000008086, 0.000000000000000000, 0.000000000000000000 ) ) ;
#19783 = CARTESIAN_POINT ( 'NONE',  ( -35.50000000000000711, -114.1152303497977414, 9.513755561829650986 ) ) ;
#19784 = DIRECTION ( 'NONE',  ( -1.000000000000000000, 0.000000000000000000, -0.000000000000000000 ) ) ;
#19786 = CIRCLE ( 'NONE', #29607, 20.00000000000000711 ) ;
#19785 = CARTESIAN_POINT ( 'NONE',  ( 7.999999999999992895, -13.85708833600001277, 45.43276465116660745 ) ) ;
#19787 = ADVANCED_FACE ( 'NONE', ( #24784 ), #9093, .T. ) ;
#19788 = VECTOR ( 'NONE', #14195, 1000.000000000000000 ) ;
#19789 = ORIENTED_EDGE ( 'NONE', *, *, #14595, .T. ) ;
#19790 = EDGE_CURVE ( 'NONE', #5839, #9669, #10324, .T. ) ;
#19791 = ORIENTED_EDGE ( 'NONE', *, *, #30883, .T. ) ;
#19792 = EDGE_CURVE ( 'NONE', #24314, #25036, #5720, .T. ) ;
#19793 = CARTESIAN_POINT ( 'NONE',  ( 8.000000000000000000, 13.55483219355729396, 11.06713717293245658 ) ) ;
#19794 = DIRECTION ( 'NONE',  ( -1.000000000000000000, 0.000000000000000000, 0.000000000000000000 ) ) ;
#19795 = VECTOR ( 'NONE', #6765, 1000.000000000000000 ) ;
#19796 = ORIENTED_EDGE ( 'NONE', *, *, #13656, .F. ) ;
#19797 = CARTESIAN_POINT ( 'NONE',  ( -10.00000000000000178, 0.000000000000000000, 0.000000000000000000 ) ) ;
#19798 = ORIENTED_EDGE ( 'NONE', *, *, #28005, .T. ) ;
#19799 = CARTESIAN_POINT ( 'NONE',  ( -35.50000000000000000, -115.0140978167137860, -0.6247823525984403936 ) ) ;
#19800 = DIRECTION ( 'NONE',  ( 0.000000000000000000, 0.9980267284282713369, 0.06279051952931692659 ) ) ;
#19801 = CARTESIAN_POINT ( 'NONE',  ( -37.88768952767750164, -115.9754527089670262, 4.972274454178448266 ) ) ;
#19802 = EDGE_CURVE ( 'NONE', #20350, #33969, #5694, .T. ) ;
#19803 = ORIENTED_EDGE ( 'NONE', *, *, #17281, .T. ) ;
#19804 = DIRECTION ( 'NONE',  ( 1.000000000000000000, 0.000000000000000000, -0.000000000000000000 ) ) ;
#19805 = EDGE_CURVE ( 'NONE', #9366, #10551, #13208, .T. ) ;
#19806 = AXIS2_PLACEMENT_3D ( 'NONE', #34624, #9944, #26528 ) ;
#19807 = ORIENTED_EDGE ( 'NONE', *, *, #20217, .F. ) ;
#19808 = DIRECTION ( 'NONE',  ( 1.000000000000000000, 0.000000000000000000, 0.000000000000000000 ) ) ;
#19809 = CARTESIAN_POINT ( 'NONE',  ( -35.50000000000000711, -112.0209493036498287, 0.9959249592223760050 ) ) ;
#19810 = ORIENTED_EDGE ( 'NONE', *, *, #1981, .T. ) ;
#19811 = ORIENTED_EDGE ( 'NONE', *, *, #13745, .F. ) ;
#19812 = CARTESIAN_POINT ( 'NONE',  ( 8.000000000000000000, 0.000000000000000000, 0.000000000000000000 ) ) ;
#19813 = SURFACE_STYLE_USAGE ( .BOTH. , #16774 ) ;
#19814 = CYLINDRICAL_SURFACE ( 'NONE', #27378, 47.49900000000001654 ) ;
#19815 = ORIENTED_EDGE ( 'NONE', *, *, #29832, .F. ) ;
#19816 = VERTEX_POINT ( 'NONE', #11784 ) ;
#19817 = CARTESIAN_POINT ( 'NONE',  ( -34.50000000000000000, -113.0796441757086939, 1.890140615870383956 ) ) ;
#19818 = DIRECTION ( 'NONE',  ( -1.000000000000000000, 0.000000000000000000, 0.000000000000000000 ) ) ;
#19819 = PRODUCT_DEFINITION_SHAPE ( 'NONE', 'NONE',  #34383 ) ;
#19820 = EDGE_LOOP ( 'NONE', ( #18302, #12455, #32062, #30783, #25776, #33050 ) ) ;
#19821 = ORIENTED_EDGE ( 'NONE', *, *, #282, .F. ) ;
#19822 = LINE ( 'NONE', #17311, #28704 ) ;
#19823 = EDGE_CURVE ( 'NONE', #10826, #12629, #3005, .T. ) ;
#19824 = VECTOR ( 'NONE', #20248, 1000.000000000000000 ) ;
#19825 = AXIS2_PLACEMENT_3D ( 'NONE', #19557, #13653, #30735 ) ;
#19826 = CARTESIAN_POINT ( 'NONE',  ( -35.50000000000000000, -113.9929510916434339, 10.50625754673588474 ) ) ;
#19827 = EDGE_CURVE ( 'NONE', #9833, #13647, #30709, .T. ) ;
#19828 = CARTESIAN_POINT ( 'NONE',  ( -90.00000000000002842, 0.000000000000000000, 6.938893903907228378E-15 ) ) ;
#19829 = LINE ( 'NONE', #3315, #25126 ) ;
#19830 = ADVANCED_FACE ( 'NONE', ( #804 ), #25487, .T. ) ;
#19831 = CARTESIAN_POINT ( 'NONE',  ( -34.50000000000000000, -111.0360125565790383, 1.176611260687384419 ) ) ;
#19832 = CARTESIAN_POINT ( 'NONE',  ( -38.99924736195577424, -115.9929510916434481, 12.66759465831984599 ) ) ;
#19833 = AXIS2_PLACEMENT_3D ( 'NONE', #22866, #727, #1267 ) ;
#19834 = DIRECTION ( 'NONE',  ( 0.000000000000000000, -0.8090169943749533354, 0.5877852522924649215 ) ) ;
#19835 = CARTESIAN_POINT ( 'NONE',  ( 0.000000000000000000, 0.000000000000000000, 0.000000000000000000 ) ) ;
#19836 = ADVANCED_FACE ( 'NONE', ( #28186 ), #17354, .T. ) ;
#19837 = CARTESIAN_POINT ( 'NONE',  ( 0.000000000000000000, -2.710505431213761085E-17, 45.89999999999999858 ) ) ;
#19838 = CARTESIAN_POINT ( 'NONE',  ( 50.00000000000000000, 1.347111479062090574E-15, 81.00000000000001421 ) ) ;
#19839 = EDGE_CURVE ( 'NONE', #4766, #34692, #4583, .T. ) ;
#19840 = CARTESIAN_POINT ( 'NONE',  ( 4.000000000000003553, 46.77034588191304465, 22.72740077717247331 ) ) ;
#19841 = VERTEX_POINT ( 'NONE', #3702 ) ;
#19842 = LINE ( 'NONE', #3149, #30082 ) ;
#19843 = DIRECTION ( 'NONE',  ( 0.000000000000000000, 0.000000000000000000, -1.000000000000000000 ) ) ;
#19844 = AXIS2_PLACEMENT_3D ( 'NONE', #16263, #16631, #8005 ) ;
#19845 = CARTESIAN_POINT ( 'NONE',  ( -42.49999999999999289, -37.28532556477433246, 76.74125644078564790 ) ) ;
#19846 = CARTESIAN_POINT ( 'NONE',  ( 0.000000000000000000, 16.71027810728552154, -2.620268201066000113 ) ) ;
#19847 = FACE_OUTER_BOUND ( 'NONE', #30265, .T. ) ;
#19848 = CARTESIAN_POINT ( 'NONE',  ( 4.872650870659739120, 0.4273491293402878477, 5.720942237434551585E-15 ) ) ;
#19849 = AXIS2_PLACEMENT_3D ( 'NONE', #27632, #6005, #22910 ) ;
#19850 = ADVANCED_FACE ( 'NONE', ( #3528 ), #3175, .F. ) ;
#19851 = ORIENTED_EDGE ( 'NONE', *, *, #12600, .F. ) ;
#19852 = DIRECTION ( 'NONE',  ( -1.000000000000000000, 0.000000000000000000, 0.000000000000000000 ) ) ;
#19853 = CARTESIAN_POINT ( 'NONE',  ( -39.49999999999999289, -14.67619866229204284, 104.0227405789415371 ) ) ;
#19854 = DIRECTION ( 'NONE',  ( 0.000000000000000000, -1.000000000000000000, 0.000000000000000000 ) ) ;
#19855 = VERTEX_POINT ( 'NONE', #11978 ) ;
#19856 = CARTESIAN_POINT ( 'NONE',  ( -37.99999999999998579, -114.0592624029313242, 6.246475545821551734 ) ) ;
#19857 = EDGE_LOOP ( 'NONE', ( #19932, #14199, #32542, #22099 ) ) ;
#19858 = VECTOR ( 'NONE', #28417, 1000.000000000000000 ) ;
#19859 = ORIENTED_EDGE ( 'NONE', *, *, #30824, .F. ) ;
#19860 = ORIENTED_EDGE ( 'NONE', *, *, #8593, .F. ) ;
#19861 = CYLINDRICAL_SURFACE ( 'NONE', #6836, 6.000000000000005329 ) ;
#19862 = CARTESIAN_POINT ( 'NONE',  ( -35.50000000000000711, -113.6807644833805995, -1.624782352598427959 ) ) ;
#19863 = EDGE_CURVE ( 'NONE', #10643, #34202, #14653, .T. ) ;
#19864 = DIRECTION ( 'NONE',  ( -1.000000000000000000, 0.000000000000000000, 0.000000000000000000 ) ) ;
#19865 = EDGE_CURVE ( 'NONE', #27467, #34112, #19356, .T. ) ;
#19866 = CIRCLE ( 'NONE', #34269, 52.00000000000000711 ) ;
#19867 = DIRECTION ( 'NONE',  ( -1.000000000000000000, 0.000000000000000000, 0.000000000000000000 ) ) ;
#19868 = DIRECTION ( 'NONE',  ( -1.000000000000000000, 0.000000000000000000, 0.000000000000000000 ) ) ;
#19869 = FACE_OUTER_BOUND ( 'NONE', #33461, .T. ) ;
#19870 = VECTOR ( 'NONE', #2398, 1000.000000000000000 ) ;
#19871 = CONICAL_SURFACE ( 'NONE', #18743, 4.980000000000017302, 0.5675376247847534472 ) ;
#19872 = CARTESIAN_POINT ( 'NONE',  ( -34.50000000000000000, -114.1264797827112574, 9.515205387299289441 ) ) ;
#19873 = CARTESIAN_POINT ( 'NONE',  ( 0.000000000000000000, 0.000000000000000000, 65.00000000000000000 ) ) ;
#19874 = CIRCLE ( 'NONE', #6663, 20.00000000000000355 ) ;
#19875 = ADVANCED_FACE ( 'NONE', ( #6040, #461, #30364, #25307, #13966 ), #24957, .F. ) ;
#19876 = FACE_OUTER_BOUND ( 'NONE', #28916, .T. ) ;
#19877 = CARTESIAN_POINT ( 'NONE',  ( -35.50000000000000000, -114.2600084737790809, 8.524153227862690585 ) ) ;
#19878 = CARTESIAN_POINT ( 'NONE',  ( -35.50000000000000711, -112.0140900043112282, 0.8439677466545482121 ) ) ;
#19879 = CARTESIAN_POINT ( 'NONE',  ( -39.49999999999999289, -11.24969279549607748, 111.5585998451919778 ) ) ;
#19880 = CIRCLE ( 'NONE', #34892, 4.999999999999990230 ) ;
#19881 = CARTESIAN_POINT ( 'NONE',  ( 1.398397006337009918, -6.091550361990587525, -0.7999999999999951594 ) ) ;
#19882 = AXIS2_PLACEMENT_3D ( 'NONE', #17369, #28371, #5874 ) ;
#19883 = CARTESIAN_POINT ( 'NONE',  ( 7.999999999999992895, -15.49408907645203470, 44.90087086784588877 ) ) ;
#19884 = PLANE ( 'NONE',  #29629 ) ;
#19885 = CARTESIAN_POINT ( 'NONE',  ( -9.999999999999994671, 0.000000000000000000, 0.000000000000000000 ) ) ;
#19886 = DIRECTION ( 'NONE',  ( -1.000000000000000000, -0.000000000000000000, -0.000000000000000000 ) ) ;
#19887 = VERTEX_POINT ( 'NONE', #19526 ) ;
#19888 = CARTESIAN_POINT ( 'NONE',  ( -37.05926240293131713, -113.0000000000000000, 6.621475545821551734 ) ) ;
#19889 = CARTESIAN_POINT ( 'NONE',  ( 4.000000000000003553, -35.11945359308084846, -38.34871548466050939 ) ) ;
#19890 = CARTESIAN_POINT ( 'NONE',  ( 3.799999999999999822, 0.000000000000000000, 49.10000000000000142 ) ) ;
#19891 = ORIENTED_EDGE ( 'NONE', *, *, #26825, .T. ) ;
#19892 = AXIS2_PLACEMENT_3D ( 'NONE', #35123, #15281, #26296 ) ;
#19893 = ORIENTED_EDGE ( 'NONE', *, *, #23520, .T. ) ;
#19894 = DIRECTION ( 'NONE',  ( 1.174092375852890260E-15, -4.222049128630259891E-16, -1.000000000000000000 ) ) ;
#19895 = AXIS2_PLACEMENT_3D ( 'NONE', #19797, #11900, #25241 ) ;
#19896 = CARTESIAN_POINT ( 'NONE',  ( 112.0000000000000000, 81.48267994499606459, 30.15054357219658954 ) ) ;
#19897 = VERTEX_POINT ( 'NONE', #22583 ) ;
#19898 = CARTESIAN_POINT ( 'NONE',  ( -39.07941549657749647, -116.1632251905417803, 4.558975545821549957 ) ) ;
#19899 = ORIENTED_EDGE ( 'NONE', *, *, #4028, .T. ) ;
#19900 = AXIS2_PLACEMENT_3D ( 'NONE', #25907, #23190, #3955 ) ;
#19901 = DIRECTION ( 'NONE',  ( -1.000000000000000000, 0.000000000000000000, 0.000000000000000000 ) ) ;
#19902 = AXIS2_PLACEMENT_3D ( 'NONE', #5189, #16488, #5530 ) ;
#19903 = DIRECTION ( 'NONE',  ( -1.000000000000000000, 0.000000000000000000, 0.000000000000000000 ) ) ;
#19904 = AXIS2_PLACEMENT_3D ( 'NONE', #25064, #14423, #14251 ) ;
#19905 = APPLICATION_PROTOCOL_DEFINITION ( 'draft international standard', 'automotive_design', 1998, #25960 ) ;
#19906 = DIRECTION ( 'NONE',  ( 0.000000000000000000, 0.000000000000000000, -1.000000000000000000 ) ) ;
#19907 = ORIENTED_EDGE ( 'NONE', *, *, #31972, .F. ) ;
#19908 = ORIENTED_EDGE ( 'NONE', *, *, #16808, .F. ) ;
#19909 = EDGE_CURVE ( 'NONE', #27440, #12176, #33574, .T. ) ;
#19910 = CARTESIAN_POINT ( 'NONE',  ( 0.000000000000000000, 0.000000000000000000, 65.00000000000000000 ) ) ;
#19911 = ORIENTED_EDGE ( 'NONE', *, *, #24261, .F. ) ;
#19912 = DIRECTION ( 'NONE',  ( 1.000000000000000000, 0.000000000000000000, 0.000000000000000000 ) ) ;
#19913 = VECTOR ( 'NONE', #11147, 1000.000000000000000 ) ;
#19914 = CARTESIAN_POINT ( 'NONE',  ( -34.50000000000000000, -114.6807644833805000, -0.6247823525984269599 ) ) ;
#19915 = CARTESIAN_POINT ( 'NONE',  ( 8.000000000000007105, 8.725776631572825792, 3.753907720749072308 ) ) ;
#19916 = DIRECTION ( 'NONE',  ( 0.000000000000000000, 0.000000000000000000, 1.000000000000000000 ) ) ;
#19917 = CARTESIAN_POINT ( 'NONE',  ( -34.50000000000000000, -115.9929510916434481, 10.52826033068511435 ) ) ;
#19918 = CIRCLE ( 'NONE', #16520, 9.999999999999994671 ) ;
#19919 = CARTESIAN_POINT ( 'NONE',  ( 7.999999999999992895, 42.03146605346787368, 22.12489237027333289 ) ) ;
#19920 = CARTESIAN_POINT ( 'NONE',  ( 8.000000000000000000, 10.46102064772367868, -19.35373470438973698 ) ) ;
#19921 = CARTESIAN_POINT ( 'NONE',  ( -37.88878409051687868, -114.9929510916434339, 14.07058620477052102 ) ) ;
#19922 = FACE_BOUND ( 'NONE', #26951, .T. ) ;
#19923 = AXIS2_PLACEMENT_3D ( 'NONE', #20098, #3744, #26064 ) ;
#19924 = CIRCLE ( 'NONE', #14749, 8.000000000000000000 ) ;
#19925 = FACE_OUTER_BOUND ( 'NONE', #29551, .T. ) ;
#19926 = VECTOR ( 'NONE', #25253, 1000.000000000000000 ) ;
#19927 = CARTESIAN_POINT ( 'NONE',  ( -9.999999999999994671, 0.000000000000000000, 0.000000000000000000 ) ) ;
#19928 = DIRECTION ( 'NONE',  ( 0.000000000000000000, 0.4817536741017100499, 0.8763066800438663595 ) ) ;
#19929 = ORIENTED_EDGE ( 'NONE', *, *, #3954, .T. ) ;
#19930 = AXIS2_PLACEMENT_3D ( 'NONE', #31601, #23313, #31956 ) ;
#19931 = CARTESIAN_POINT ( 'NONE',  ( 0.000000000000000000, 0.000000000000000000, 0.000000000000000000 ) ) ;
#19932 = ORIENTED_EDGE ( 'NONE', *, *, #18559, .F. ) ;
#19933 = COLOUR_RGB ( '', 0.31764706, 0.68627451, 0.89019608) ;
#19934 = CARTESIAN_POINT ( 'NONE',  ( -35.81662171581204746, -117.0245472910329738, 7.784774454178449155 ) ) ;
#19935 = VECTOR ( 'NONE', #3645, 1000.000000000000000 ) ;
#19936 = DIRECTION ( 'NONE',  ( -1.000000000000000000, 0.000000000000000000, 0.000000000000000000 ) ) ;
#19937 = CARTESIAN_POINT ( 'NONE',  ( -35.50000000000000711, -115.1446187476384040, -1.616767172155725740 ) ) ;
#19938 = ORIENTED_EDGE ( 'NONE', *, *, #1450, .T. ) ;
#19939 = ORIENTED_EDGE ( 'NONE', *, *, #26584, .T. ) ;
#19940 = CARTESIAN_POINT ( 'NONE',  ( -1.600000000000004086, -12.74999999999999822, 0.000000000000000000 ) ) ;
#19941 = CARTESIAN_POINT ( 'NONE',  ( 46.00000000000000000, 0.000000000000000000, 0.000000000000000000 ) ) ;
#19942 = ORIENTED_EDGE ( 'NONE', *, *, #2447, .F. ) ;
#19943 = AXIS2_PLACEMENT_3D ( 'NONE', #31817, #12922, #21189 ) ;
#19944 = AXIS2_PLACEMENT_3D ( 'NONE', #15584, #26782, #20993 ) ;
#19945 = DIRECTION ( 'NONE',  ( 0.000000000000000000, -1.000000000000000000, 0.000000000000000000 ) ) ;
#19946 = ORIENTED_EDGE ( 'NONE', *, *, #8852, .F. ) ;
#19947 = ORIENTED_EDGE ( 'NONE', *, *, #5784, .T. ) ;
#19948 = CARTESIAN_POINT ( 'NONE',  ( -38.37230871539094323, -115.4561184093552413, 4.558975545821550845 ) ) ;
#19949 = CIRCLE ( 'NONE', #33226, 52.00000000000000711 ) ;
#19950 = CIRCLE ( 'NONE', #10199, 47.49900000000001654 ) ;
#19951 = DIRECTION ( 'NONE',  ( 0.000000000000000000, 0.000000000000000000, 1.000000000000000000 ) ) ;
#19952 = ORIENTED_EDGE ( 'NONE', *, *, #34596, .T. ) ;
#19953 = ORIENTED_EDGE ( 'NONE', *, *, #19209, .F. ) ;
#19954 = CARTESIAN_POINT ( 'NONE',  ( -35.50000000000000000, -111.0140978167138570, 0.6252176474015680441 ) ) ;
#19955 = AXIS2_PLACEMENT_3D ( 'NONE', #20172, #34063, #22890 ) ;
#19956 = EDGE_CURVE ( 'NONE', #6860, #16883, #30881, .T. ) ;
#19957 = EDGE_CURVE ( 'NONE', #14155, #21171, #33342, .T. ) ;
#19958 = CARTESIAN_POINT ( 'NONE',  ( 50.00000000000000000, 0.000000000000000000, 70.00000000000000000 ) ) ;
#19959 = ORIENTED_EDGE ( 'NONE', *, *, #10820, .T. ) ;
#19960 = AXIS2_PLACEMENT_3D ( 'NONE', #33385, #30350, #5683 ) ;
#19961 = CARTESIAN_POINT ( 'NONE',  ( -35.50000000000000711, -114.9929510916434339, 12.26648026267477221 ) ) ;
#19962 = CARTESIAN_POINT ( 'NONE',  ( -39.00000000000000000, -113.9929510916434339, 11.21034663311206181 ) ) ;
#19963 = PLANE ( 'NONE',  #18334 ) ;
#19964 = DIRECTION ( 'NONE',  ( -1.000000000000000000, 0.000000000000000000, 0.000000000000000000 ) ) ;
#19965 = EDGE_CURVE ( 'NONE', #30730, #34251, #28181, .T. ) ;
#19966 = CARTESIAN_POINT ( 'NONE',  ( -36.62499999999902656, -113.9929510916434339, 14.11852480586265024 ) ) ;
#19967 = DIRECTION ( 'NONE',  ( -1.000000000000000000, -1.836970198721029934E-16, -0.000000000000000000 ) ) ;
#19968 = CARTESIAN_POINT ( 'NONE',  ( -35.91854304697313438, -114.9929510916434339, 13.11211614918345703 ) ) ;
#19969 = CARTESIAN_POINT ( 'NONE',  ( 3.799999999999999822, 4.382607293638566128E-16, 45.89999999999999858 ) ) ;
#19970 = CARTESIAN_POINT ( 'NONE',  ( 7.999999999999992895, 39.78933988720114456, 24.98727647985016276 ) ) ;
#19971 = DIRECTION ( 'NONE',  ( 1.000000000000000000, 0.000000000000000000, 0.000000000000000000 ) ) ;
#19972 = VECTOR ( 'NONE', #19967, 1000.000000000000000 ) ;
#19973 = ORIENTED_EDGE ( 'NONE', *, *, #28326, .F. ) ;
#19974 = CARTESIAN_POINT ( 'NONE',  ( -37.99839555572501837, -115.9929510916434481, 12.65937477241749143 ) ) ;
#19975 = ORIENTED_EDGE ( 'NONE', *, *, #26088, .F. ) ;
#19976 = VECTOR ( 'NONE', #32748, 1000.000000000000000 ) ;
#19977 = CARTESIAN_POINT ( 'NONE',  ( -4.000000000000000000, 0.000000000000000000, -50.00000000000000000 ) ) ;
#19978 = FACE_OUTER_BOUND ( 'NONE', #651, .T. ) ;
#19979 = AXIS2_PLACEMENT_3D ( 'NONE', #7532, #7173, #18509 ) ;
#19980 = ORIENTED_EDGE ( 'NONE', *, *, #31241, .T. ) ;
#19981 = AXIS2_PLACEMENT_3D ( 'NONE', #25882, #19903, #15047 ) ;
#19982 = DIRECTION ( 'NONE',  ( 0.000000000000000000, 0.9980267284282717810, -0.06279051952930990443 ) ) ;
#19983 = VERTEX_POINT ( 'NONE', #20398 ) ;
#19984 = CARTESIAN_POINT ( 'NONE',  ( -35.50000000000000000, -115.0140978167138712, -0.4685323525984309012 ) ) ;
#19985 = DIRECTION ( 'NONE',  ( 1.000000000000000000, -5.339440136655842133E-16, -1.047965281155519420E-16 ) ) ;
#19986 = CARTESIAN_POINT ( 'NONE',  ( -36.25098837183129774, -113.3347980657956242, 8.816024454178446490 ) ) ;
#19987 = ORIENTED_EDGE ( 'NONE', *, *, #19092, .F. ) ;
#19988 = CARTESIAN_POINT ( 'NONE',  ( -36.23083527818512550, -116.0245472910329880, 3.284774454178449155 ) ) ;
#19989 = EDGE_CURVE ( 'NONE', #14995, #1331, #16649, .T. ) ;
#19990 = DIRECTION ( 'NONE',  ( 1.734723475976807094E-16, -1.000000000000000000, 0.000000000000000000 ) ) ;
#19991 = CARTESIAN_POINT ( 'NONE',  ( -35.50000000000000000, -115.3399256288223569, -2.599147725881697291 ) ) ;
#19992 = ORIENTED_EDGE ( 'NONE', *, *, #23566, .T. ) ;
#19993 = ORIENTED_EDGE ( 'NONE', *, *, #10425, .T. ) ;
#19994 = CARTESIAN_POINT ( 'NONE',  ( -38.37230871539094323, -112.5438815906447729, 6.941024454178449155 ) ) ;
#19995 = CONTEXT_DEPENDENT_SHAPE_REPRESENTATION ( #27176, #11003 ) ;
#19996 = CARTESIAN_POINT ( 'NONE',  ( -42.49999999999999289, -35.77980021920998155, 98.97243186433534845 ) ) ;
#19997 = ORIENTED_EDGE ( 'NONE', *, *, #28678, .T. ) ;
#19998 = ORIENTED_EDGE ( 'NONE', *, *, #12303, .F. ) ;
#19999 = CARTESIAN_POINT ( 'NONE',  ( -34.50000000000000000, -115.0140978167137860, -0.6247823525984403936 ) ) ;
#20000 = CYLINDRICAL_SURFACE ( 'NONE', #20587, 4.000000000000000000 ) ;
#20001 = EDGE_CURVE ( 'NONE', #33264, #16768, #26440, .T. ) ;
#20002 = EDGE_CURVE ( 'NONE', #10849, #10711, #15489, .T. ) ;
#20003 = EDGE_CURVE ( 'NONE', #31128, #10764, #5195, .T. ) ;
#20004 = ORIENTED_EDGE ( 'NONE', *, *, #1871, .T. ) ;
#20005 = VERTEX_POINT ( 'NONE', #23123 ) ;
#20006 = DIRECTION ( 'NONE',  ( 0.000000000000000000, 0.000000000000000000, 1.000000000000000000 ) ) ;
#20007 = CIRCLE ( 'NONE', #14286, 52.00000000000000711 ) ;
#20008 = CIRCLE ( 'NONE', #10257, 7.199999999999994849 ) ;
#20009 = CARTESIAN_POINT ( 'NONE',  ( -36.62499999999902656, -113.9929510916434339, 13.11852480586264846 ) ) ;
#20010 = CARTESIAN_POINT ( 'NONE',  ( 50.00005079999999680, 5.400000000000000355, 0.9999999999999985567 ) ) ;
#20011 = CARTESIAN_POINT ( 'NONE',  ( 7.999999999999992895, 32.32520163883631170, -34.09746168776000985 ) ) ;
#20012 = ADVANCED_FACE ( 'NONE', ( #23298 ), #9628, .T. ) ;
#20013 = CARTESIAN_POINT ( 'NONE',  ( -34.50000000000000000, -116.0140896356112989, -0.6575071456984549201 ) ) ;
#20014 = EDGE_CURVE ( 'NONE', #32626, #24291, #1526, .T. ) ;
#20015 = CARTESIAN_POINT ( 'NONE',  ( -35.50000000000000000, -115.9929510916434481, 10.59426868253284226 ) ) ;
#20016 = UNCERTAINTY_MEASURE_WITH_UNIT (LENGTH_MEASURE( 1.000000000000000082E-05 ), #33391, 'distance_accuracy_value', 'NONE');
#20017 = CARTESIAN_POINT ( 'NONE',  ( 0.000000000000000000, 17.56975900509189970, -9.555290079479078713 ) ) ;
#20018 = DIRECTION ( 'NONE',  ( 1.226634733346698078E-16, -0.2588190451025185190, -0.9659258262890689783 ) ) ;
#20019 = CYLINDRICAL_SURFACE ( 'NONE', #4507, 4.000000000000000000 ) ;
#20020 = DIRECTION ( 'NONE',  ( 0.000000000000000000, -1.000000000000000000, -1.040834085586082363E-14 ) ) ;
#20021 = CARTESIAN_POINT ( 'NONE',  ( 7.999999999999992895, 0.000000000000000000, 11.00000000000000000 ) ) ;
#20022 = ORIENTED_EDGE ( 'NONE', *, *, #11087, .T. ) ;
#20023 = DIRECTION ( 'NONE',  ( -0.000000000000000000, 0.000000000000000000, -1.000000000000000000 ) ) ;
#20024 = CARTESIAN_POINT ( 'NONE',  ( -1.387778780781445676E-14, 0.4273491293403097746, -0.7999999999999951594 ) ) ;
#20025 = DIRECTION ( 'NONE',  ( -1.000000000000000000, 0.000000000000000000, 0.000000000000000000 ) ) ;
#20026 = LINE ( 'NONE', #17699, #18434 ) ;
#20027 = AXIS2_PLACEMENT_3D ( 'NONE', #27662, #9264, #33394 ) ;
#20028 = CONTEXT_DEPENDENT_SHAPE_REPRESENTATION ( #24171, #24213 ) ;
#20029 = CIRCLE ( 'NONE', #9105, 4.872650870659778199 ) ;
#20030 = DIRECTION ( 'NONE',  ( 1.000000000000000000, -4.524158825347490025E-15, -1.177133787269970298E-15 ) ) ;
#20031 = DIRECTION ( 'NONE',  ( -1.000000000000000000, 0.000000000000000000, -0.000000000000000000 ) ) ;
#20032 = EDGE_CURVE ( 'NONE', #21122, #29583, #25899, .T. ) ;
#20033 = VERTEX_POINT ( 'NONE', #31589 ) ;
#20034 = VECTOR ( 'NONE', #33011, 1000.000000000000000 ) ;
#20035 = CARTESIAN_POINT ( 'NONE',  ( 7.999999999999992895, 32.32520163883582853, 34.09746168776048592 ) ) ;
#20036 = DIRECTION ( 'NONE',  ( 1.000000000000000000, 0.000000000000000000, 0.000000000000000000 ) ) ;
#20037 = PRODUCT_DEFINITION ( 'UNKNOWN', '', #10355, #11926 ) ;
#20038 = CARTESIAN_POINT ( 'NONE',  ( 7.999999999999992895, 25.61928775981044026, 45.25098998563487385 ) ) ;
#20039 = ORIENTED_EDGE ( 'NONE', *, *, #25810, .T. ) ;
#20040 = VERTEX_POINT ( 'NONE', #6744 ) ;
#20041 = CARTESIAN_POINT ( 'NONE',  ( -35.00000000000000000, -113.9407375970686900, 9.996475545821549957 ) ) ;
#20042 = ORIENTED_EDGE ( 'NONE', *, *, #15018, .T. ) ;
#20043 = EDGE_LOOP ( 'NONE', ( #17599, #31481, #18674, #16704 ) ) ;
#20044 = ORIENTED_EDGE ( 'NONE', *, *, #24243, .F. ) ;
#20045 = DIRECTION ( 'NONE',  ( 1.000000000000000000, 0.000000000000000000, 0.000000000000000000 ) ) ;
#20046 = ADVANCED_FACE ( 'NONE', ( #31410 ), #31765, .T. ) ;
#20047 = EDGE_CURVE ( 'NONE', #8021, #27298, #15510, .T. ) ;
#20048 = CARTESIAN_POINT ( 'NONE',  ( -35.50000000000000711, -115.1446187476384040, -1.616767172155725740 ) ) ;
#20049 = CARTESIAN_POINT ( 'NONE',  ( 0.000000000000000000, 0.000000000000000000, 0.000000000000000000 ) ) ;
#20050 = CARTESIAN_POINT ( 'NONE',  ( -35.50100302244946704, -114.9929510916434339, 12.65121853911337269 ) ) ;
#20051 = CARTESIAN_POINT ( 'NONE',  ( 0.000000000000000000, 0.000000000000000000, 0.000000000000000000 ) ) ;
#20052 = AXIS2_PLACEMENT_3D ( 'NONE', #35072, #16476, #30181 ) ;
#20053 = DIRECTION ( 'NONE',  ( -1.000000000000000000, 0.000000000000000000, 0.000000000000000000 ) ) ;
#20054 = EDGE_CURVE ( 'NONE', #23013, #18917, #15363, .T. ) ;
#20055 = CARTESIAN_POINT ( 'NONE',  ( -34.50000000000000000, -114.9929510916434339, 10.59426868253284226 ) ) ;
#20056 = CARTESIAN_POINT ( 'NONE',  ( 0.000000000000000000, 0.000000000000000000, -53.39999999999999858 ) ) ;
#20057 = VECTOR ( 'NONE', #28848, 1000.000000000000000 ) ;
#20058 = UNCERTAINTY_MEASURE_WITH_UNIT (LENGTH_MEASURE( 1.000000000000000082E-05 ), #24441, 'distance_accuracy_value', 'NONE');
#20059 = CARTESIAN_POINT ( 'NONE',  ( 7.999999999999992895, 0.000000000000000000, 0.000000000000000000 ) ) ;
#20060 = ORIENTED_EDGE ( 'NONE', *, *, #19956, .T. ) ;
#20061 = STYLED_ITEM ( 'NONE', ( #15597 ), #10186 ) ;
#20062 = CARTESIAN_POINT ( 'NONE',  ( -35.50000000000000000, -115.3279708130221479, 8.997521329298534098 ) ) ;
#20063 = CARTESIAN_POINT ( 'NONE',  ( -35.50000000000000711, -113.3557509229967764, 1.923098431109107054 ) ) ;
#20064 = CARTESIAN_POINT ( 'NONE',  ( 55.00000000000000000, 10.00000000000000888, -15.00000000000000178 ) ) ;
#20065 = DIRECTION ( 'NONE',  ( -1.000000000000000000, -1.836970198721029934E-16, -0.000000000000000000 ) ) ;
#20066 = DIRECTION ( 'NONE',  ( 0.000000000000000000, 0.000000000000000000, 1.000000000000000000 ) ) ;
#20067 = DIRECTION ( 'NONE',  ( 0.000000000000000000, 0.000000000000000000, 1.000000000000000000 ) ) ;
#20068 = FACE_OUTER_BOUND ( 'NONE', #19130, .T. ) ;
#20069 = ORIENTED_EDGE ( 'NONE', *, *, #4841, .F. ) ;
#20070 = CARTESIAN_POINT ( 'NONE',  ( -37.74901162816868805, -113.3347980657955958, 6.433975545821551734 ) ) ;
#20071 = LINE ( 'NONE', #31082, #32493 ) ;
#20072 = CARTESIAN_POINT ( 'NONE',  ( 8.000000000000000000, 13.55483219355744673, -11.06713717293225407 ) ) ;
#20073 = EDGE_CURVE ( 'NONE', #6031, #2681, #28718, .T. ) ;
#20074 = ORIENTED_EDGE ( 'NONE', *, *, #26001, .F. ) ;
#20075 = ORIENTED_EDGE ( 'NONE', *, *, #30871, .T. ) ;
#20076 = EDGE_CURVE ( 'NONE', #27224, #4610, #23671, .T. ) ;
#20077 = FACE_OUTER_BOUND ( 'NONE', #17818, .T. ) ;
#20078 = EDGE_CURVE ( 'NONE', #17645, #22530, #26020, .T. ) ;
#20079 = CARTESIAN_POINT ( 'NONE',  ( 0.000000000000000000, 0.000000000000000000, -1.200000000000006617 ) ) ;
#20080 = VERTEX_POINT ( 'NONE', #6557 ) ;
#20081 = CARTESIAN_POINT ( 'NONE',  ( -38.30190309005061522, -116.9754527089670546, 6.472274454178449155 ) ) ;
#20082 = EDGE_LOOP ( 'NONE', ( #11772, #35190, #21514, #27747 ) ) ;
#20083 = VECTOR ( 'NONE', #22107, 1000.000000000000000 ) ;
#20084 = LINE ( 'NONE', #658, #31934 ) ;
#20085 = CARTESIAN_POINT ( 'NONE',  ( 0.000000000000000000, -35.20873326984057883, -31.88259874184068465 ) ) ;
#20086 = EDGE_CURVE ( 'NONE', #17996, #15848, #26561, .T. ) ;
#20087 =( GEOMETRIC_REPRESENTATION_CONTEXT ( 3 ) GLOBAL_UNCERTAINTY_ASSIGNED_CONTEXT ( ( #9635 ) ) GLOBAL_UNIT_ASSIGNED_CONTEXT ( ( #19540, #5193, #19028 ) ) REPRESENTATION_CONTEXT ( 'NONE', 'WORKASPACE' ) );
#20088 = DIRECTION ( 'NONE',  ( 0.000000000000000000, 0.2486898871648553222, -0.9685831611286309650 ) ) ;
#20089 = EDGE_CURVE ( 'NONE', #19242, #31708, #23605, .T. ) ;
#20090 = VECTOR ( 'NONE', #24647, 1000.000000000000000 ) ;
#20091 = APPLICATION_PROTOCOL_DEFINITION ( 'draft international standard', 'automotive_design', 1998, #34261 ) ;
#20092 = DIRECTION ( 'NONE',  ( -1.000000000000000000, 0.000000000000000000, 0.000000000000000000 ) ) ;
#20093 = ORIENTED_EDGE ( 'NONE', *, *, #32436, .T. ) ;
#20094 = ORIENTED_EDGE ( 'NONE', *, *, #14571, .T. ) ;
#20095 = LINE ( 'NONE', #20444, #1272 ) ;
#20096 = DIRECTION ( 'NONE',  ( -1.000000000000000000, 0.000000000000000000, 0.000000000000000000 ) ) ;
#20097 = ORIENTED_EDGE ( 'NONE', *, *, #2381, .T. ) ;
#20098 = CARTESIAN_POINT ( 'NONE',  ( 50.00000000000000000, 0.000000000000000000, 70.00000000000000000 ) ) ;
#20099 = CARTESIAN_POINT ( 'NONE',  ( -34.50000000000000000, -113.2637153405686519, 1.912112492696748989 ) ) ;
#20100 = CARTESIAN_POINT ( 'NONE',  ( 8.000000000000000000, 0.000000000000000000, 0.000000000000000000 ) ) ;
#20101 = DIRECTION ( 'NONE',  ( 0.000000000000000000, 0.000000000000000000, -1.000000000000000000 ) ) ;
#20102 = CARTESIAN_POINT ( 'NONE',  ( -34.50000000000000000, -114.5266723804073195, 8.577838247824468354 ) ) ;
#20103 = CARTESIAN_POINT ( 'NONE',  ( 8.000000000000007105, -11.27190672109260028, -0.3151488735048807444 ) ) ;
#20104 = CARTESIAN_POINT ( 'NONE',  ( 65.00000000000001421, 0.000000000000000000, 0.000000000000000000 ) ) ;
#20105 = CARTESIAN_POINT ( 'NONE',  ( -34.50000000000000000, -114.3793648455349654, 8.543708532059524074 ) ) ;
#20106 = LINE ( 'NONE', #28070, #1553 ) ;
#20107 = CARTESIAN_POINT ( 'NONE',  ( 7.999999999999992895, 36.34385289850589373, 29.77717097092089205 ) ) ;
#20108 = AXIS2_PLACEMENT_3D ( 'NONE', #7722, #18706, #29706 ) ;
#20109 = DIRECTION ( 'NONE',  ( 0.000000000000000000, -0.3090169943749350723, -0.9510565162951575280 ) ) ;
#20110 = CARTESIAN_POINT ( 'NONE',  ( 1.599999999999990985, -4.771817072227796402E-14, 6.765000000000020997 ) ) ;
#20111 = VERTEX_POINT ( 'NONE', #28537 ) ;
#20112 = LINE ( 'NONE', #10579, #2685 ) ;
#20113 = VERTEX_POINT ( 'NONE', #25850 ) ;
#20114 = AXIS2_PLACEMENT_3D ( 'NONE', #4968, #1914, #10183 ) ;
#20115 = CARTESIAN_POINT ( 'NONE',  ( -40.02454729103296671, -112.8166217158120332, 7.840225545821554398 ) ) ;
#20116 = CARTESIAN_POINT ( 'NONE',  ( 0.000000000000000000, 0.000000000000000000, -1.200000000000006617 ) ) ;
#20117 = CARTESIAN_POINT ( 'NONE',  ( -35.50000000000000711, -115.0795240838853886, -1.623175561345890472 ) ) ;
#20118 = EDGE_CURVE ( 'NONE', #28617, #25119, #5476, .T. ) ;
#20119 = ORIENTED_EDGE ( 'NONE', *, *, #21511, .T. ) ;
#20120 = EDGE_LOOP ( 'NONE', ( #30802, #9433, #29862, #22138 ) ) ;
#20121 = EDGE_CURVE ( 'NONE', #27197, #35019, #7625, .T. ) ;
#20123 = CARTESIAN_POINT ( 'NONE',  ( 7.999999999999992895, -34.03046037009280411, 33.13733193845794034 ) ) ;
#20122 = PRODUCT_DEFINITION_SHAPE ( 'NONE', 'NONE',  #20037 ) ;
#20124 = DIRECTION ( 'NONE',  ( 0.000000000000000000, 0.000000000000000000, 1.000000000000000000 ) ) ;
#20125 = VERTEX_POINT ( 'NONE', #4777 ) ;
#20126 = EDGE_LOOP ( 'NONE', ( #8685, #27770, #16568, #10111 ) ) ;
#20127 = CARTESIAN_POINT ( 'NONE',  ( 7.999999999999992895, 8.053585752061906078, 46.81126742072027014 ) ) ;
#20128 = ORIENTED_EDGE ( 'NONE', *, *, #14595, .F. ) ;
#20129 = EDGE_LOOP ( 'NONE', ( #6338, #24724 ) ) ;
#20130 = CARTESIAN_POINT ( 'NONE',  ( -38.37230871539094323, -115.4561184093552413, 7.558975545821551734 ) ) ;
#20131 = DIRECTION ( 'NONE',  ( 0.000000000000000000, 0.000000000000000000, 1.000000000000000000 ) ) ;
#20132 = CARTESIAN_POINT ( 'NONE',  ( 4.000000000000003553, -51.85248208264521708, 3.914090171286008335 ) ) ;
#20133 = VERTEX_POINT ( 'NONE', #16247 ) ;
#20134 = ORIENTED_EDGE ( 'NONE', *, *, #15343, .F. ) ;
#20135 = AXIS2_PLACEMENT_3D ( 'NONE', #17235, #19745, #11663 ) ;
#20136 = CARTESIAN_POINT ( 'NONE',  ( -35.50000000000000000, -113.4307644833805142, -2.624782352598442614 ) ) ;
#20137 = CARTESIAN_POINT ( 'NONE',  ( 8.000000000000000000, 16.59870953437680896, 3.253005020243904255 ) ) ;
#20138 = CIRCLE ( 'NONE', #35147, 8.000000000000000000 ) ;
#20139 = EDGE_LOOP ( 'NONE', ( #27027, #31536, #7887, #17525 ) ) ;
#20140 = AXIS2_PLACEMENT_3D ( 'NONE', #31887, #27217, #13182 ) ;
#20141 = DIRECTION ( 'NONE',  ( 1.783119874454246424E-31, 1.187911941725854497E-31, -1.000000000000000000 ) ) ;
#20142 = CARTESIAN_POINT ( 'NONE',  ( -37.46874999999995737, -113.9929510916434339, 14.11852480586265024 ) ) ;
#20143 = CARTESIAN_POINT ( 'NONE',  ( -44.00000000000000000, 0.000000000000000000, 0.000000000000000000 ) ) ;
#20144 = CYLINDRICAL_SURFACE ( 'NONE', #33519, 9.499000000000000554 ) ;
#20145 = CARTESIAN_POINT ( 'NONE',  ( -35.07817881376918479, -113.9929510916434339, 13.81802396319203474 ) ) ;
#20146 = CARTESIAN_POINT ( 'NONE',  ( 46.00000000000000000, -25.98076211353320275, 84.99999999999992895 ) ) ;
#20147 = CARTESIAN_POINT ( 'NONE',  ( -36.12500000000014211, -114.9929510916434339, 13.11852480586264669 ) ) ;
#20148 = DIRECTION ( 'NONE',  ( 0.000000000000000000, 0.000000000000000000, 1.000000000000000000 ) ) ;
#20149 = EDGE_LOOP ( 'NONE', ( #29419, #31225 ) ) ;
#20150 = CARTESIAN_POINT ( 'NONE',  ( 2.000000000000001776, 0.000000000000000000, 0.000000000000000000 ) ) ;
#20151 = CARTESIAN_POINT ( 'NONE',  ( 0.000000000000000000, 0.000000000000000000, 0.000000000000000000 ) ) ;
#20152 = ORIENTED_EDGE ( 'NONE', *, *, #19092, .T. ) ;
#20153 = CARTESIAN_POINT ( 'NONE',  ( -35.91854304697313438, -114.9929510916434339, 13.11211614918345703 ) ) ;
#20154 =( BOUNDED_SURFACE ( )  B_SPLINE_SURFACE ( 3, 3, ( 
 ( #12459, #23073, #29020, #20352, #6694, #33889, #17676, #28844, #34247, #28675, #7046, #4021, #31550, #23253, #14965, #9580, #20549, #22896, #31184, #4195, #26330, #34439, #6513, #15137, #26144, #4369, #23445, #18023, #9757, #20718, #31715, #15317, #9220, #28424, #6102, #33829, #3423, #3067, #5927, #25204, #33465, #17071, #30767, #3766, #19755, #25379, #28080, #8789, #30945, #526, #14202, #17246, #14373, #3239, #27893, #867, #14023, #691, #5759, #33298, #11675, #16716, #11506, #14723, #22642, #25016, #28252, #22305, #6453, #8619, #16889, #19431, #22476, #33636, #8970, #19589, #20117, #19937, #6278, #3591, #14539, #30592, #341, #8450, #30429, #11339, #17423, #25554, #27727, #11852, #22833, #31126, #9153, #25737, #1067, #12036, #23011, #34188, #34546, #18325, #31651, #23733 ),
 ( #25913, #4673, #6626, #9693, #1240, #15602, #7163, #29146, #6985, #12578, #29323, #6808, #32014, #1600, #9863, #10044, #34371, #20649, #31486, #31828, #21009, #7354, #17779, #12933, #23370, #9335, #3959, #9511, #26624, #20294, #34724, #1957, #14902, #34011, #17957, #26261, #31300, #17598, #28608, #1778, #12217, #23194, #20472, #28783, #4133, #28960, #18137, #23550, #20825, #15430, #4306, #15072, #12755, #26084, #1415, #12392, #4498, #26443, #15250, #6737, #12500, #31585, #34291, #26554, #23482, #7089, #1340, #26184, #18062, #17527, #34477, #12142, #28886, #9434, #1519, #34830, #4236, #9796, #29254, #12319, #6916, #3879, #17888, #20757, #34113, #12865, #14839, #15176, #20392, #23841, #15356, #1702, #31757, #29064, #1892, #15006, #4599, #4414, #26370, #18249, #12687, #23664 ),
 ( #31404, #17715, #34653, #23291, #23116, #28714, #9973, #20933, #31933, #7271, #4063, #15533, #10153, #26011, #21123, #9621, #6551, #28531, #25844, #1168, #20588, #21299, #35362, #29425, #30131, #18608, #13045, #10691, #2424, #5127, #13393, #24734, #13226, #32656, #27442, #18784, #24031, #24375, #32295, #21655, #21472, #24200, #16421, #7981, #18962, #26914, #16064, #29958, #7450, #5299, #2070, #29786, #35022, #27083, #59, #16240, #27259, #19131, #2258, #4773, #7617, #7798, #15716, #35192, #2789, #32468, #10340, #2599, #29606, #5467, #4945, #15894, #18426, #10510, #13567, #24557, #35549, #8149, #10876, #21838, #32831, #13752, #11046, #32122, #26730, #8322, #2958, #19999, #17131, #33008, #16779, #33529, #9041, #8857, #22709, #19301, #24904, #33186, #22184, #22536, #6340, #19649 ),
 ( #19488, #11212, #228, #30492, #28138, #3306, #19817, #582, #16947, #27953, #942, #14431, #5650, #3481, #405, #25618, #25439, #3127, #27791, #22011, #14079, #27623, #757, #5821, #25075, #8513, #5991, #11399, #22360, #33356, #30313, #30829, #31006, #16611, #8681, #14605, #11737, #14260, #6166, #13916, #30659, #33703, #3657, #25260, #17307, #11568, #28310, #1474, #23624, #12282, #9219, #1295, #17846, #3836, #18206, #20177, #23252, #14795, #29215, #20717, #7045, #20548, #26143, #7224, #20351, #9928, #15136, #23444, #34612, #34246, #9578, #9395, #9756, #20891, #31890, #31362, #26514, #31549, #22895, #17488, #12098, #4562, #33888, #1663, #15495, #28485, #12644, #6874, #4194, #31183, #11923, #6512, #15315, #25801, #1127, #23072, #34069, #6692, #28843, #31714, #12457, #34438 ),
 ( #17675, #28674, #18022, #4020, #29019, #14964, #4368, #25969, #26329, #26867, #29569, #21790, #18737, #2388, #32260, #21434, #13356, #12821, #7755, #23982, #18386, #16024, #29740, #10474, #5084, #30090, #18565, #24337, #32786, #24159, #29390, #27044, #2024, #35328, #2217, #4904, #8109, #10649, #21605, #7581, #32432, #32608, #23802, #7939, #7412, #35154, #4735, #18918, #5430, #29916, #5261, #24510, #15845, #34785, #26692, #13185, #10105, #16199, #19091, #27220, #15671, #2563, #12996, #35502, #34978, #10300, #21075, #13529, #10835, #16378, #21261, #1848, #32082, #30614, #11356, #5779, #2915, #19262, #27393, #13710, #8284, #25397, #22496, #2746, #22146, #3258, #14389, #14220, #28097, #24688, #30266, #13875, #27577, #27911, #11692, #25037, #17087, #22323, #21967, #24861, #8469, #16737 ),
 ( #8639, #14038, #27745, #25222, #19450, #33140, #541, #3085, #30448, #11174, #19773, #32965, #33315, #16, #710, #358, #16570, #186, #19609, #5946, #5607, #16906, #11525, #33485, #8810, #30785, #6119, #3440, #22665, #33655, #8988, #19954, #30964, #6297, #11002, #17265, #14745, #6471, #20494, #14557, #15270, #3976, #9880, #20670, #9531, #17797, #11873, #31144, #31666, #34565, #17441, #26279, #23210, #25754, #6829, #28976, #17620, #25575, #6647, #34203, #9171, #23571, #893, #28629, #20136, #20842, #26101, #12410, #25927, #31504, #12597, #1083, #1618, #28799, #4149, #4325, #14918, #1253, #12052, #15089, #31845, #28270, #23027, #3611, #12237, #22850, #33846, #28444, #3788, #34029, #7001, #9353, #20309, #17974, #1432, #23393, #31319, #34391, #9711, #10601, #276, #10061 ),
 ( #5218, #29342, #23750, #21391, #13142, #15798, #24120, #11260, #23937, #7706, #2515, #29521, #34740, #35109, #7371, #10432, #32211, #34931, #27175, #32385, #18692, #1974, #26819, #29689, #18158, #5033, #12774, #4856, #21029, #2170, #22233, #15983, #26999, #29872, #12950, #4517, #32034, #18518, #15448, #10256, #13481, #7539, #18343, #2344, #4688, #16156, #15621, #26645, #29166, #21219, #13314, #24293, #35282, #18874, #21558, #32557, #7889, #24463, #7180, #26462, #1797, #19523, #14128, #33756, #28533, #19862, #25128, #3524, #33398, #14472, #22578, #25302, #17529, #25482, #9089, #28006, #17175, #20048, #8551, #801, #3171, #30878, #458, #28182, #25845, #6216, #11780, #20222, #3357, #30531, #22402, #8901, #5861, #14303, #3881, #33571, #11438, #17349, #8722, #31229, #19689, #6034 ) ),
 .UNSPECIFIED., .T., .F., .F. ) 
 B_SPLINE_SURFACE_WITH_KNOTS ( ( 4, 3, 4 ),
 ( 4, 2, 2, 2, 2, 2, 2, 2, 2, 2, 2, 2, 2, 2, 2, 2, 2, 2, 2, 2, 2, 2, 2, 2, 2, 2, 2, 2, 2, 2, 2, 2, 2, 2, 2, 2, 2, 2, 2, 2, 2, 2, 2, 2, 2, 2, 2, 2, 2, 2, 4 ),
 ( 0.000000000000000000, 0.5000000000000000000, 1.000000000000000000 ),
 ( 0.000000000000000000, 0.05194669433742771930, 0.07792004150614158242, 0.09090671509049851051, 0.09740005188267697456, 0.1038933886748554386, 0.1123700156520060500, 0.1208466426291566476, 0.1377998965834578704, 0.1717064044920602883, 0.2056129124006627062, 0.2225661663549639291, 0.2310427933321145266, 0.2395194203092651519, 0.2482763131408625423, 0.2570332059724599327, 0.2745469916356546580, 0.3095745629620442196, 0.3446021342884337813, 0.3621159199516285621, 0.3708728127832259247, 0.3796297056148233429, 0.3887999023441631730, 0.3979700990735030031, 0.4163104925321826633, 0.4529912794495420392, 0.4896720663669014151, 0.5080124598255810753, 0.5171826565549209054, 0.5263528532842607355, 0.5380287103930572190, 0.5497045675018538136, 0.5730562817194468916, 0.6197597101546329368, 0.6664631385898189819, 0.6898148528074120600, 0.7014907099162086546, 0.7131665670250051381, 0.7223367637543449682, 0.7315069604836847983, 0.7498473539423643475, 0.7865281408597235568, 0.8232089277770826552, 0.8415493212357623154, 0.8507195179651021455, 0.8598897146944418646, 0.8686466075260392827, 0.8774035003576365899, 0.8949172860208314262, 0.9299448573472208768, 1.000000000000000000 ),
 .UNSPECIFIED. ) 
 GEOMETRIC_REPRESENTATION_ITEM ( )  RATIONAL_B_SPLINE_SURFACE ( (
 ( 1.000000000000000000, 1.000000000000000000, 1.000000000000000000, 1.000000000000000000, 1.000000000000000000, 1.000000000000000000, 1.000000000000000000, 1.000000000000000000, 1.000000000000000000, 1.000000000000000000, 1.000000000000000000, 1.000000000000000000, 1.000000000000000000, 1.000000000000000000, 1.000000000000000000, 1.000000000000000000, 1.000000000000000000, 1.000000000000000000, 1.000000000000000000, 1.000000000000000000, 1.000000000000000000, 1.000000000000000000, 1.000000000000000000, 1.000000000000000000, 1.000000000000000000, 1.000000000000000000, 1.000000000000000000, 1.000000000000000000, 1.000000000000000000, 1.000000000000000000, 1.000000000000000000, 1.000000000000000000, 1.000000000000000000, 1.000000000000000000, 1.000000000000000000, 1.000000000000000000, 1.000000000000000000, 1.000000000000000000, 1.000000000000000000, 1.000000000000000000, 1.000000000000000000, 1.000000000000000000, 1.000000000000000000, 1.000000000000000000, 1.000000000000000000, 1.000000000000000000, 1.000000000000000000, 1.000000000000000000, 1.000000000000000000, 1.000000000000000000, 1.000000000000000000, 1.000000000000000000, 1.000000000000000000, 1.000000000000000000, 1.000000000000000000, 1.000000000000000000, 1.000000000000000000, 1.000000000000000000, 1.000000000000000000, 1.000000000000000000, 1.000000000000000000, 1.000000000000000000, 1.000000000000000000, 1.000000000000000000, 1.000000000000000000, 1.000000000000000000, 1.000000000000000000, 1.000000000000000000, 1.000000000000000000, 1.000000000000000000, 1.000000000000000000, 1.000000000000000000, 1.000000000000000000, 1.000000000000000000, 1.000000000000000000, 1.000000000000000000, 1.000000000000000000, 1.000000000000000000, 1.000000000000000000, 1.000000000000000000, 1.000000000000000000, 1.000000000000000000, 1.000000000000000000, 1.000000000000000000, 1.000000000000000000, 1.000000000000000000, 1.000000000000000000, 1.000000000000000000, 1.000000000000000000, 1.000000000000000000, 1.000000000000000000, 1.000000000000000000, 1.000000000000000000, 1.000000000000000000, 1.000000000000000000, 1.000000000000000000, 1.000000000000000000, 1.000000000000000000, 1.000000000000000000, 1.000000000000000000, 1.000000000000000000, 1.000000000000000000),
 ( 0.3333333333333333703, 0.3333333333333333703, 0.3333333333333333703, 0.3333333333333333703, 0.3333333333333333703, 0.3333333333333333703, 0.3333333333333333703, 0.3333333333333333703, 0.3333333333333333703, 0.3333333333333333703, 0.3333333333333333703, 0.3333333333333333703, 0.3333333333333333703, 0.3333333333333333703, 0.3333333333333333703, 0.3333333333333333703, 0.3333333333333333703, 0.3333333333333333703, 0.3333333333333333703, 0.3333333333333333703, 0.3333333333333333703, 0.3333333333333333703, 0.3333333333333333703, 0.3333333333333333703, 0.3333333333333333703, 0.3333333333333333703, 0.3333333333333333703, 0.3333333333333333703, 0.3333333333333333703, 0.3333333333333333703, 0.3333333333333333703, 0.3333333333333333703, 0.3333333333333333703, 0.3333333333333333703, 0.3333333333333333703, 0.3333333333333333703, 0.3333333333333333703, 0.3333333333333333703, 0.3333333333333333703, 0.3333333333333333703, 0.3333333333333333703, 0.3333333333333333703, 0.3333333333333333703, 0.3333333333333333703, 0.3333333333333333703, 0.3333333333333333703, 0.3333333333333333703, 0.3333333333333333703, 0.3333333333333333703, 0.3333333333333333703, 0.3333333333333333703, 0.3333333333333333703, 0.3333333333333333703, 0.3333333333333333703, 0.3333333333333333703, 0.3333333333333333703, 0.3333333333333333703, 0.3333333333333333703, 0.3333333333333333703, 0.3333333333333333703, 0.3333333333333333703, 0.3333333333333333703, 0.3333333333333333703, 0.3333333333333333703, 0.3333333333333333703, 0.3333333333333333703, 0.3333333333333333703, 0.3333333333333333703, 0.3333333333333333703, 0.3333333333333333703, 0.3333333333333333703, 0.3333333333333333703, 0.3333333333333333703, 0.3333333333333333703, 0.3333333333333333703, 0.3333333333333333703, 0.3333333333333333703, 0.3333333333333333703, 0.3333333333333333703, 0.3333333333333333703, 0.3333333333333333703, 0.3333333333333333703, 0.3333333333333333703, 0.3333333333333333703, 0.3333333333333333703, 0.3333333333333333703, 0.3333333333333333703, 0.3333333333333333703, 0.3333333333333333703, 0.3333333333333333703, 0.3333333333333333703, 0.3333333333333333703, 0.3333333333333333703, 0.3333333333333333703, 0.3333333333333333703, 0.3333333333333333703, 0.3333333333333333703, 0.3333333333333333703, 0.3333333333333333703, 0.3333333333333333703, 0.3333333333333333703, 0.3333333333333333703),
 ( 0.3333333333333333703, 0.3333333333333333703, 0.3333333333333333703, 0.3333333333333333703, 0.3333333333333333703, 0.3333333333333333703, 0.3333333333333333703, 0.3333333333333333703, 0.3333333333333333703, 0.3333333333333333703, 0.3333333333333333703, 0.3333333333333333703, 0.3333333333333333703, 0.3333333333333333703, 0.3333333333333333703, 0.3333333333333333703, 0.3333333333333333703, 0.3333333333333333703, 0.3333333333333333703, 0.3333333333333333703, 0.3333333333333333703, 0.3333333333333333703, 0.3333333333333333703, 0.3333333333333333703, 0.3333333333333333703, 0.3333333333333333703, 0.3333333333333333703, 0.3333333333333333703, 0.3333333333333333703, 0.3333333333333333703, 0.3333333333333333703, 0.3333333333333333703, 0.3333333333333333703, 0.3333333333333333703, 0.3333333333333333703, 0.3333333333333333703, 0.3333333333333333703, 0.3333333333333333703, 0.3333333333333333703, 0.3333333333333333703, 0.3333333333333333703, 0.3333333333333333703, 0.3333333333333333703, 0.3333333333333333703, 0.3333333333333333703, 0.3333333333333333703, 0.3333333333333333703, 0.3333333333333333703, 0.3333333333333333703, 0.3333333333333333703, 0.3333333333333333703, 0.3333333333333333703, 0.3333333333333333703, 0.3333333333333333703, 0.3333333333333333703, 0.3333333333333333703, 0.3333333333333333703, 0.3333333333333333703, 0.3333333333333333703, 0.3333333333333333703, 0.3333333333333333703, 0.3333333333333333703, 0.3333333333333333703, 0.3333333333333333703, 0.3333333333333333703, 0.3333333333333333703, 0.3333333333333333703, 0.3333333333333333703, 0.3333333333333333703, 0.3333333333333333703, 0.3333333333333333703, 0.3333333333333333703, 0.3333333333333333703, 0.3333333333333333703, 0.3333333333333333703, 0.3333333333333333703, 0.3333333333333333703, 0.3333333333333333703, 0.3333333333333333703, 0.3333333333333333703, 0.3333333333333333703, 0.3333333333333333703, 0.3333333333333333703, 0.3333333333333333703, 0.3333333333333333703, 0.3333333333333333703, 0.3333333333333333703, 0.3333333333333333703, 0.3333333333333333703, 0.3333333333333333703, 0.3333333333333333703, 0.3333333333333333703, 0.3333333333333333703, 0.3333333333333333703, 0.3333333333333333703, 0.3333333333333333703, 0.3333333333333333703, 0.3333333333333333703, 0.3333333333333333703, 0.3333333333333333703, 0.3333333333333333703, 0.3333333333333333703),
 ( 1.000000000000000000, 1.000000000000000000, 1.000000000000000000, 1.000000000000000000, 1.000000000000000000, 1.000000000000000000, 1.000000000000000000, 1.000000000000000000, 1.000000000000000000, 1.000000000000000000, 1.000000000000000000, 1.000000000000000000, 1.000000000000000000, 1.000000000000000000, 1.000000000000000000, 1.000000000000000000, 1.000000000000000000, 1.000000000000000000, 1.000000000000000000, 1.000000000000000000, 1.000000000000000000, 1.000000000000000000, 1.000000000000000000, 1.000000000000000000, 1.000000000000000000, 1.000000000000000000, 1.000000000000000000, 1.000000000000000000, 1.000000000000000000, 1.000000000000000000, 1.000000000000000000, 1.000000000000000000, 1.000000000000000000, 1.000000000000000000, 1.000000000000000000, 1.000000000000000000, 1.000000000000000000, 1.000000000000000000, 1.000000000000000000, 1.000000000000000000, 1.000000000000000000, 1.000000000000000000, 1.000000000000000000, 1.000000000000000000, 1.000000000000000000, 1.000000000000000000, 1.000000000000000000, 1.000000000000000000, 1.000000000000000000, 1.000000000000000000, 1.000000000000000000, 1.000000000000000000, 1.000000000000000000, 1.000000000000000000, 1.000000000000000000, 1.000000000000000000, 1.000000000000000000, 1.000000000000000000, 1.000000000000000000, 1.000000000000000000, 1.000000000000000000, 1.000000000000000000, 1.000000000000000000, 1.000000000000000000, 1.000000000000000000, 1.000000000000000000, 1.000000000000000000, 1.000000000000000000, 1.000000000000000000, 1.000000000000000000, 1.000000000000000000, 1.000000000000000000, 1.000000000000000000, 1.000000000000000000, 1.000000000000000000, 1.000000000000000000, 1.000000000000000000, 1.000000000000000000, 1.000000000000000000, 1.000000000000000000, 1.000000000000000000, 1.000000000000000000, 1.000000000000000000, 1.000000000000000000, 1.000000000000000000, 1.000000000000000000, 1.000000000000000000, 1.000000000000000000, 1.000000000000000000, 1.000000000000000000, 1.000000000000000000, 1.000000000000000000, 1.000000000000000000, 1.000000000000000000, 1.000000000000000000, 1.000000000000000000, 1.000000000000000000, 1.000000000000000000, 1.000000000000000000, 1.000000000000000000, 1.000000000000000000, 1.000000000000000000),
 ( 0.3333333333333333703, 0.3333333333333333703, 0.3333333333333333703, 0.3333333333333333703, 0.3333333333333333703, 0.3333333333333333703, 0.3333333333333333703, 0.3333333333333333703, 0.3333333333333333703, 0.3333333333333333703, 0.3333333333333333703, 0.3333333333333333703, 0.3333333333333333703, 0.3333333333333333703, 0.3333333333333333703, 0.3333333333333333703, 0.3333333333333333703, 0.3333333333333333703, 0.3333333333333333703, 0.3333333333333333703, 0.3333333333333333703, 0.3333333333333333703, 0.3333333333333333703, 0.3333333333333333703, 0.3333333333333333703, 0.3333333333333333703, 0.3333333333333333703, 0.3333333333333333703, 0.3333333333333333703, 0.3333333333333333703, 0.3333333333333333703, 0.3333333333333333703, 0.3333333333333333703, 0.3333333333333333703, 0.3333333333333333703, 0.3333333333333333703, 0.3333333333333333703, 0.3333333333333333703, 0.3333333333333333703, 0.3333333333333333703, 0.3333333333333333703, 0.3333333333333333703, 0.3333333333333333703, 0.3333333333333333703, 0.3333333333333333703, 0.3333333333333333703, 0.3333333333333333703, 0.3333333333333333703, 0.3333333333333333703, 0.3333333333333333703, 0.3333333333333333703, 0.3333333333333333703, 0.3333333333333333703, 0.3333333333333333703, 0.3333333333333333703, 0.3333333333333333703, 0.3333333333333333703, 0.3333333333333333703, 0.3333333333333333703, 0.3333333333333333703, 0.3333333333333333703, 0.3333333333333333703, 0.3333333333333333703, 0.3333333333333333703, 0.3333333333333333703, 0.3333333333333333703, 0.3333333333333333703, 0.3333333333333333703, 0.3333333333333333703, 0.3333333333333333703, 0.3333333333333333703, 0.3333333333333333703, 0.3333333333333333703, 0.3333333333333333703, 0.3333333333333333703, 0.3333333333333333703, 0.3333333333333333703, 0.3333333333333333703, 0.3333333333333333703, 0.3333333333333333703, 0.3333333333333333703, 0.3333333333333333703, 0.3333333333333333703, 0.3333333333333333703, 0.3333333333333333703, 0.3333333333333333703, 0.3333333333333333703, 0.3333333333333333703, 0.3333333333333333703, 0.3333333333333333703, 0.3333333333333333703, 0.3333333333333333703, 0.3333333333333333703, 0.3333333333333333703, 0.3333333333333333703, 0.3333333333333333703, 0.3333333333333333703, 0.3333333333333333703, 0.3333333333333333703, 0.3333333333333333703, 0.3333333333333333703, 0.3333333333333333703),
 ( 0.3333333333333333703, 0.3333333333333333703, 0.3333333333333333703, 0.3333333333333333703, 0.3333333333333333703, 0.3333333333333333703, 0.3333333333333333703, 0.3333333333333333703, 0.3333333333333333703, 0.3333333333333333703, 0.3333333333333333703, 0.3333333333333333703, 0.3333333333333333703, 0.3333333333333333703, 0.3333333333333333703, 0.3333333333333333703, 0.3333333333333333703, 0.3333333333333333703, 0.3333333333333333703, 0.3333333333333333703, 0.3333333333333333703, 0.3333333333333333703, 0.3333333333333333703, 0.3333333333333333703, 0.3333333333333333703, 0.3333333333333333703, 0.3333333333333333703, 0.3333333333333333703, 0.3333333333333333703, 0.3333333333333333703, 0.3333333333333333703, 0.3333333333333333703, 0.3333333333333333703, 0.3333333333333333703, 0.3333333333333333703, 0.3333333333333333703, 0.3333333333333333703, 0.3333333333333333703, 0.3333333333333333703, 0.3333333333333333703, 0.3333333333333333703, 0.3333333333333333703, 0.3333333333333333703, 0.3333333333333333703, 0.3333333333333333703, 0.3333333333333333703, 0.3333333333333333703, 0.3333333333333333703, 0.3333333333333333703, 0.3333333333333333703, 0.3333333333333333703, 0.3333333333333333703, 0.3333333333333333703, 0.3333333333333333703, 0.3333333333333333703, 0.3333333333333333703, 0.3333333333333333703, 0.3333333333333333703, 0.3333333333333333703, 0.3333333333333333703, 0.3333333333333333703, 0.3333333333333333703, 0.3333333333333333703, 0.3333333333333333703, 0.3333333333333333703, 0.3333333333333333703, 0.3333333333333333703, 0.3333333333333333703, 0.3333333333333333703, 0.3333333333333333703, 0.3333333333333333703, 0.3333333333333333703, 0.3333333333333333703, 0.3333333333333333703, 0.3333333333333333703, 0.3333333333333333703, 0.3333333333333333703, 0.3333333333333333703, 0.3333333333333333703, 0.3333333333333333703, 0.3333333333333333703, 0.3333333333333333703, 0.3333333333333333703, 0.3333333333333333703, 0.3333333333333333703, 0.3333333333333333703, 0.3333333333333333703, 0.3333333333333333703, 0.3333333333333333703, 0.3333333333333333703, 0.3333333333333333703, 0.3333333333333333703, 0.3333333333333333703, 0.3333333333333333703, 0.3333333333333333703, 0.3333333333333333703, 0.3333333333333333703, 0.3333333333333333703, 0.3333333333333333703, 0.3333333333333333703, 0.3333333333333333703, 0.3333333333333333703),
 ( 1.000000000000000000, 1.000000000000000000, 1.000000000000000000, 1.000000000000000000, 1.000000000000000000, 1.000000000000000000, 1.000000000000000000, 1.000000000000000000, 1.000000000000000000, 1.000000000000000000, 1.000000000000000000, 1.000000000000000000, 1.000000000000000000, 1.000000000000000000, 1.000000000000000000, 1.000000000000000000, 1.000000000000000000, 1.000000000000000000, 1.000000000000000000, 1.000000000000000000, 1.000000000000000000, 1.000000000000000000, 1.000000000000000000, 1.000000000000000000, 1.000000000000000000, 1.000000000000000000, 1.000000000000000000, 1.000000000000000000, 1.000000000000000000, 1.000000000000000000, 1.000000000000000000, 1.000000000000000000, 1.000000000000000000, 1.000000000000000000, 1.000000000000000000, 1.000000000000000000, 1.000000000000000000, 1.000000000000000000, 1.000000000000000000, 1.000000000000000000, 1.000000000000000000, 1.000000000000000000, 1.000000000000000000, 1.000000000000000000, 1.000000000000000000, 1.000000000000000000, 1.000000000000000000, 1.000000000000000000, 1.000000000000000000, 1.000000000000000000, 1.000000000000000000, 1.000000000000000000, 1.000000000000000000, 1.000000000000000000, 1.000000000000000000, 1.000000000000000000, 1.000000000000000000, 1.000000000000000000, 1.000000000000000000, 1.000000000000000000, 1.000000000000000000, 1.000000000000000000, 1.000000000000000000, 1.000000000000000000, 1.000000000000000000, 1.000000000000000000, 1.000000000000000000, 1.000000000000000000, 1.000000000000000000, 1.000000000000000000, 1.000000000000000000, 1.000000000000000000, 1.000000000000000000, 1.000000000000000000, 1.000000000000000000, 1.000000000000000000, 1.000000000000000000, 1.000000000000000000, 1.000000000000000000, 1.000000000000000000, 1.000000000000000000, 1.000000000000000000, 1.000000000000000000, 1.000000000000000000, 1.000000000000000000, 1.000000000000000000, 1.000000000000000000, 1.000000000000000000, 1.000000000000000000, 1.000000000000000000, 1.000000000000000000, 1.000000000000000000, 1.000000000000000000, 1.000000000000000000, 1.000000000000000000, 1.000000000000000000, 1.000000000000000000, 1.000000000000000000, 1.000000000000000000, 1.000000000000000000, 1.000000000000000000, 1.000000000000000000) ) ) 
 REPRESENTATION_ITEM ( '' )  SURFACE ( )  );
#20155 = EDGE_LOOP ( 'NONE', ( #26859, #27294, #18502, #8286 ) ) ;
#20156 = DIRECTION ( 'NONE',  ( -1.000000000000000000, 0.000000000000000000, 0.000000000000000000 ) ) ;
#20157 = VERTEX_POINT ( 'NONE', #13400 ) ;
#20158 = CARTESIAN_POINT ( 'NONE',  ( 0.000000000000000000, 22.82995208772687334, 41.06517797613670950 ) ) ;
#20159 = ORIENTED_EDGE ( 'NONE', *, *, #19277, .F. ) ;
#20160 = ADVANCED_FACE ( 'NONE', ( #7805 ), #2431, .T. ) ;
#20161 = CARTESIAN_POINT ( 'NONE',  ( -35.50000000000000000, -115.0140978167143402, -0.6247823525984417259 ) ) ;
#20162 = CYLINDRICAL_SURFACE ( 'NONE', #17889, 47.49900000000001654 ) ;
#20163 = CARTESIAN_POINT ( 'NONE',  ( -35.62769128460905677, -115.4561184093552413, 3.191024454178449155 ) ) ;
#20164 = AXIS2_PLACEMENT_3D ( 'NONE', #386, #30640, #34054 ) ;
#20165 = EDGE_LOOP ( 'NONE', ( #3348, #26602, #7394, #28116 ) ) ;
#20166 = VECTOR ( 'NONE', #17438, 1000.000000000000000 ) ;
#20167 = CARTESIAN_POINT ( 'NONE',  ( -36.11231047232249125, -112.0245472910329880, 2.722274454178448266 ) ) ;
#20168 = LINE ( 'NONE', #31174, #23990 ) ;
#20169 = CARTESIAN_POINT ( 'NONE',  ( -35.50000000000000711, -114.9724313160460696, -1.624792769101446765 ) ) ;
#20170 = VERTEX_POINT ( 'NONE', #8159 ) ;
#20171 = ORIENTED_EDGE ( 'NONE', *, *, #22026, .T. ) ;
#20172 = CARTESIAN_POINT ( 'NONE',  ( 0.000000000000000000, 0.000000000000000000, 0.000000000000000000 ) ) ;
#20173 = EDGE_CURVE ( 'NONE', #31617, #15981, #35111, .T. ) ;
#20174 = DIRECTION ( 'NONE',  ( -1.000000000000000000, -0.000000000000000000, 0.000000000000000000 ) ) ;
#20175 = VERTEX_POINT ( 'NONE', #12872 ) ;
#20176 = ORIENTED_EDGE ( 'NONE', *, *, #23830, .F. ) ;
#20177 = CARTESIAN_POINT ( 'NONE',  ( -34.50000000000000000, -112.8511839106603247, -1.611965039240275122 ) ) ;
#20178 = CARTESIAN_POINT ( 'NONE',  ( 1.799999999999996048, 0.000000000000000000, 0.000000000000000000 ) ) ;
#20179 = VERTEX_POINT ( 'NONE', #24384 ) ;
#20180 = VERTEX_POINT ( 'NONE', #2608 ) ;
#20181 = CARTESIAN_POINT ( 'NONE',  ( 0.000000000000000000, -14.87816164169111133, -4.342730381190020417 ) ) ;
#20182 = CARTESIAN_POINT ( 'NONE',  ( -36.31249999999994316, -113.9929510916434339, 13.11852480586264846 ) ) ;
#20183 = CARTESIAN_POINT ( 'NONE',  ( -34.50000000000000000, -112.0140978167138712, 0.6252176474015680441 ) ) ;
#20184 = CARTESIAN_POINT ( 'NONE',  ( 0.000000000000000000, 0.000000000000000000, 0.000000000000000000 ) ) ;
#20185 = AXIS2_PLACEMENT_3D ( 'NONE', #21607, #2389, #19093 ) ;
#20186 = COLOUR_RGB ( '', 0.08235294, 0.09019608, 0.10196078) ;
#20187 = AXIS2_PLACEMENT_3D ( 'NONE', #32919, #140, #14343 ) ;
#20188 = CARTESIAN_POINT ( 'NONE',  ( -35.50100302244945993, -113.9929510916434339, 12.65121853911337446 ) ) ;
#20189 = CARTESIAN_POINT ( 'NONE',  ( -35.56312645773537895, -115.9929510916434481, 12.87038173996308998 ) ) ;
#20190 = CARTESIAN_POINT ( 'NONE',  ( 8.000000000000007105, -5.908880290975582206, 9.604183132802395662 ) ) ;
#20191 = DIRECTION ( 'NONE',  ( 0.000000000000000000, 0.000000000000000000, -1.000000000000000000 ) ) ;
#20192 = CARTESIAN_POINT ( 'NONE',  ( 8.000000000000000000, -10.62435788049434038, -13.16139124467930444 ) ) ;
#20193 = CARTESIAN_POINT ( 'NONE',  ( 8.000000000000000000, -13.55483219355736679, 11.06713717293235888 ) ) ;
#20194 = CARTESIAN_POINT ( 'NONE',  ( -34.50000000000001421, -33.18172400785640264, 69.52756813566438154 ) ) ;
#20195 = ORIENTED_EDGE ( 'NONE', *, *, #15044, .T. ) ;
#20196 = MECHANICAL_DESIGN_GEOMETRIC_PRESENTATION_REPRESENTATION (  '', ( #28866 ), #16198 ) ;
#20197 = CARTESIAN_POINT ( 'NONE',  ( 3.872983346207416133, 1.000000000000001110, -22.00000000000000000 ) ) ;
#20198 = LINE ( 'NONE', #31029, #26777 ) ;
#20199 = ADVANCED_FACE ( 'NONE', ( #16429 ), #10696, .T. ) ;
#20200 = DIRECTION ( 'NONE',  ( 0.000000000000000000, 0.000000000000000000, -1.000000000000000000 ) ) ;
#20201 = CARTESIAN_POINT ( 'NONE',  ( 4.000000000000000000, 4.898587196589412829E-16, 50.00000000000000000 ) ) ;
#20202 = ADVANCED_FACE ( 'NONE', ( #35371 ), #27091, .T. ) ;
#20203 = FACE_OUTER_BOUND ( 'NONE', #20796, .T. ) ;
#20204 = LINE ( 'NONE', #6905, #1529 ) ;
#20205 = ORIENTED_EDGE ( 'NONE', *, *, #17895, .F. ) ;
#20206 = FACE_OUTER_BOUND ( 'NONE', #34031, .T. ) ;
#20207 = CARTESIAN_POINT ( 'NONE',  ( -34.50000000000000000, -112.4957190293567066, -2.560864217808777266 ) ) ;
#20208 = DIRECTION ( 'NONE',  ( -1.000000000000000000, 0.000000000000000000, 0.000000000000000000 ) ) ;
#20209 = VERTEX_POINT ( 'NONE', #21662 ) ;
#20210 = ORIENTED_EDGE ( 'NONE', *, *, #22684, .T. ) ;
#20211 = CARTESIAN_POINT ( 'NONE',  ( -37.74901162816869515, -114.6652019342044042, 5.066024454178449155 ) ) ;
#20212 = EDGE_CURVE ( 'NONE', #18458, #4062, #21304, .T. ) ;
#20213 = ORIENTED_EDGE ( 'NONE', *, *, #25848, .F. ) ;
#20214 = AXIS2_PLACEMENT_3D ( 'NONE', #7496, #29477, #21516 ) ;
#20215 = MECHANICAL_DESIGN_GEOMETRIC_PRESENTATION_REPRESENTATION (  '', ( #3012 ), #29452 ) ;
#20216 = AXIS2_PLACEMENT_3D ( 'NONE', #21513, #35408, #34882 ) ;
#20217 = EDGE_CURVE ( 'NONE', #1101, #5612, #1736, .T. ) ;
#20218 = PRESENTATION_STYLE_ASSIGNMENT (( #23288 ) ) ;
#20219 = ORIENTED_EDGE ( 'NONE', *, *, #6334, .F. ) ;
#20220 = EDGE_LOOP ( 'NONE', ( #23392, #10015, #11823, #16355 ) ) ;
#20221 = CARTESIAN_POINT ( 'NONE',  ( 2.000000000000002665, -4.694161725993254197E-16, -6.765000000000044977 ) ) ;
#20222 = CARTESIAN_POINT ( 'NONE',  ( -35.50000000000000711, -116.0012805033554883, -0.7876962586524312027 ) ) ;
#20223 = FACE_OUTER_BOUND ( 'NONE', #16900, .T. ) ;
#20224 = CARTESIAN_POINT ( 'NONE',  ( -35.87040530316090070, -114.9929510916434339, 13.10254527216545917 ) ) ;
#20225 = DIRECTION ( 'NONE',  ( -1.174092375852890260E-15, 4.222049128630259891E-16, 1.000000000000000000 ) ) ;
#20226 = CARTESIAN_POINT ( 'NONE',  ( 0.9999999999999731326, -4.808326913196006913, -0.7999999999999951594 ) ) ;
#20227 = EDGE_CURVE ( 'NONE', #375, #26423, #22425, .T. ) ;
#20228 = CARTESIAN_POINT ( 'NONE',  ( -34.50000000000000000, -114.9929510916434339, 10.52000928670414126 ) ) ;
#20229 = DIRECTION ( 'NONE',  ( 1.000000000000000000, 0.000000000000000000, 0.000000000000000000 ) ) ;
#20230 = AXIS2_PLACEMENT_3D ( 'NONE', #23812, #28852, #34618 ) ;
#20231 = CARTESIAN_POINT ( 'NONE',  ( 7.999999999999992895, 0.2227391519116599106, 46.98410307550729215 ) ) ;
#20232 = ORIENTED_EDGE ( 'NONE', *, *, #30791, .F. ) ;
#20233 = CARTESIAN_POINT ( 'NONE',  ( -35.50000000000000000, -115.9929510916434481, 10.61627146648203990 ) ) ;
#20235 = CARTESIAN_POINT ( 'NONE',  ( -35.50000000000000711, -112.9185811467682754, 1.870920967077121411 ) ) ;
#20234 = AXIS2_PLACEMENT_3D ( 'NONE', #9977, #35196, #24203 ) ;
#20236 = FACE_OUTER_BOUND ( 'NONE', #29775, .T. ) ;
#20237 = CARTESIAN_POINT ( 'NONE',  ( -1.387778780781445676E-14, 0.4273491293403097746, -0.7999999999999951594 ) ) ;
#20238 = CARTESIAN_POINT ( 'NONE',  ( -34.49999999999998579, -26.94801722181404102, 85.25380613764170334 ) ) ;
#20239 = DIRECTION ( 'NONE',  ( 1.000000000000000000, -0.000000000000000000, 0.000000000000000000 ) ) ;
#20240 = DIRECTION ( 'NONE',  ( -1.000000000000000000, -0.000000000000000000, -0.000000000000000000 ) ) ;
#20241 = ADVANCED_FACE ( 'NONE', ( #13054 ), #24041, .T. ) ;
#20242 = DIRECTION ( 'NONE',  ( -1.000000000000000000, -1.836970198721029934E-16, -0.000000000000000000 ) ) ;
#20243 = CARTESIAN_POINT ( 'NONE',  ( -1.599999999999990319, 0.000000000000000000, 0.000000000000000000 ) ) ;
#20244 = ORIENTED_EDGE ( 'NONE', *, *, #19386, .T. ) ;
#20245 = EDGE_CURVE ( 'NONE', #34729, #27973, #32779, .T. ) ;
#20246 = EDGE_CURVE ( 'NONE', #15919, #20473, #17229, .T. ) ;
#20247 = CARTESIAN_POINT ( 'NONE',  ( -37.35495115944176803, -115.0245472910329880, 8.965225545821551734 ) ) ;
#20248 = DIRECTION ( 'NONE',  ( 0.000000000000000000, 1.000000000000000000, 0.000000000000000000 ) ) ;
#20249 = CARTESIAN_POINT ( 'NONE',  ( 7.999999999999992895, 46.21320724403649649, 10.97699764141971102 ) ) ;
#20250 = ORIENTED_EDGE ( 'NONE', *, *, #22938, .F. ) ;
#20251 = CIRCLE ( 'NONE', #24326, 14.00000000000000000 ) ;
#20252 = ORIENTED_EDGE ( 'NONE', *, *, #304, .F. ) ;
#20253 = AXIS2_PLACEMENT_3D ( 'NONE', #14138, #808, #6223 ) ;
#20254 = DIRECTION ( 'NONE',  ( -1.000000000000000000, 0.000000000000000000, 0.000000000000000000 ) ) ;
#20255 = ORIENTED_EDGE ( 'NONE', *, *, #21592, .T. ) ;
#20256 = CARTESIAN_POINT ( 'NONE',  ( -39.16322519054178741, -111.9205845034225177, 9.433975545821549957 ) ) ;
#20257 = EDGE_CURVE ( 'NONE', #9536, #15604, #32126, .T. ) ;
#20258 = ORIENTED_EDGE ( 'NONE', *, *, #34308, .F. ) ;
#20259 = EDGE_CURVE ( 'NONE', #8283, #14579, #24174, .T. ) ;
#20260 = CIRCLE ( 'NONE', #31799, 8.000000000000015987 ) ;
#20261 = DIRECTION ( 'NONE',  ( -1.000000000000000000, -0.000000000000000000, -0.000000000000000000 ) ) ;
#20262 = AXIS2_PLACEMENT_3D ( 'NONE', #27187, #32224, #7719 ) ;
#20263 = DIRECTION ( 'NONE',  ( -1.000000000000000000, 0.000000000000000000, -0.000000000000000000 ) ) ;
#20264 = APPLICATION_PROTOCOL_DEFINITION ( 'draft international standard', 'automotive_design', 1998, #3670 ) ;
#20265 = DIRECTION ( 'NONE',  ( -1.000000000000000000, 0.000000000000000000, 0.000000000000000000 ) ) ;
#20266 = ORIENTED_EDGE ( 'NONE', *, *, #33716, .T. ) ;
#20267 = VERTEX_POINT ( 'NONE', #26922 ) ;
#20268 = DIRECTION ( 'NONE',  ( 1.000000000000000000, -0.000000000000000000, -0.000000000000000000 ) ) ;
#20269 = DIRECTION ( 'NONE',  ( 1.174092375852890260E-15, -4.222049128630259891E-16, -1.000000000000000000 ) ) ;
#20270 = EDGE_LOOP ( 'NONE', ( #12949, #30260 ) ) ;
#20271 = DIRECTION ( 'NONE',  ( -0.000000000000000000, 0.000000000000000000, 1.000000000000000000 ) ) ;
#20272 = EDGE_CURVE ( 'NONE', #30962, #26405, #32472, .T. ) ;
#20273 = AXIS2_PLACEMENT_3D ( 'NONE', #18694, #27534, #13485 ) ;
#20274 = CARTESIAN_POINT ( 'NONE',  ( -34.50000000000000000, -115.0140978167137860, -0.6247823525984395054 ) ) ;
#20275 = FACE_OUTER_BOUND ( 'NONE', #5858, .T. ) ;
#20276 = CARTESIAN_POINT ( 'NONE',  ( -34.50000000000000000, -116.0140978167138712, -0.3122823525984417259 ) ) ;
#20277 = CARTESIAN_POINT ( 'NONE',  ( -34.50000000000000000, -115.9929510916434481, 10.85830208992344303 ) ) ;
#20278 = ADVANCED_FACE ( 'NONE', ( #18969 ), #21845, .F. ) ;
#20279 = DIRECTION ( 'NONE',  ( -1.174092375852890260E-15, 4.222049128630259891E-16, 1.000000000000000000 ) ) ;
#20280 = CARTESIAN_POINT ( 'NONE',  ( -39.02454729103295961, -114.7691647218148745, 2.159774454178448710 ) ) ;
#20281 = CARTESIAN_POINT ( 'NONE',  ( -37.59808119975203766, -114.9929510916434339, 14.11551573851448893 ) ) ;
#20282 = CYLINDRICAL_SURFACE ( 'NONE', #20491, 13.99999999999999822 ) ;
#20283 = CARTESIAN_POINT ( 'NONE',  ( 1.479000000000008086, 0.000000000000000000, 0.000000000000000000 ) ) ;
#20284 = DIRECTION ( 'NONE',  ( -1.000000000000000000, 0.000000000000000000, 0.000000000000000000 ) ) ;
#20285 = DIRECTION ( 'NONE',  ( 0.000000000000000000, 0.000000000000000000, -1.000000000000000000 ) ) ;
#20286 = AXIS2_PLACEMENT_3D ( 'NONE', #327, #33452, #33108 ) ;
#20287 = LINE ( 'NONE', #17952, #18770 ) ;
#20288 = VERTEX_POINT ( 'NONE', #8865 ) ;
#20289 = ADVANCED_FACE ( 'NONE', ( #13757 ), #11224, .F. ) ;
#20290 = AXIS2_PLACEMENT_3D ( 'NONE', #27653, #444, #2992 ) ;
#20291 = CARTESIAN_POINT ( 'NONE',  ( -34.00000000000000000, -113.9407375970686758, 2.496475545821551290 ) ) ;
#20292 = EDGE_CURVE ( 'NONE', #13511, #29087, #14089, .T. ) ;
#20293 = DIRECTION ( 'NONE',  ( -1.000000000000000000, 0.000000000000000000, 0.000000000000000000 ) ) ;
#20294 = CARTESIAN_POINT ( 'NONE',  ( -35.50000000000000000, -113.0140978167138712, 0.7502176474015694874 ) ) ;
#20295 = VERTEX_POINT ( 'NONE', #8519 ) ;
#20296 = ORIENTED_EDGE ( 'NONE', *, *, #28596, .F. ) ;
#20297 = DIRECTION ( 'NONE',  ( -1.000000000000000000, 0.000000000000000000, 0.000000000000000000 ) ) ;
#20298 = CARTESIAN_POINT ( 'NONE',  ( 0.000000000000000000, 0.000000000000000000, -39.50000000000000711 ) ) ;
#20299 = ORIENTED_EDGE ( 'NONE', *, *, #19565, .T. ) ;
#20300 = VERTEX_POINT ( 'NONE', #22722 ) ;
#20301 = CIRCLE ( 'NONE', #5414, 22.00000000000000000 ) ;
#20302 = CARTESIAN_POINT ( 'NONE',  ( 7.999999999999992895, -47.00885577955408223, -6.806061952192771436 ) ) ;
#20303 = ORIENTED_EDGE ( 'NONE', *, *, #34749, .F. ) ;
#20304 = CARTESIAN_POINT ( 'NONE',  ( -36.11231047232249836, -115.9754527089670262, 2.777725545821551290 ) ) ;
#20305 = CARTESIAN_POINT ( 'NONE',  ( 0.000000000000000000, 0.000000000000000000, 0.000000000000000000 ) ) ;
#20306 = CARTESIAN_POINT ( 'NONE',  ( 7.999999999999992895, -50.95304419620817526, -10.38206564895716255 ) ) ;
#20307 = VERTEX_POINT ( 'NONE', #589 ) ;
#20308 = VERTEX_POINT ( 'NONE', #5658 ) ;
#20309 = CARTESIAN_POINT ( 'NONE',  ( -35.50000000000000000, -117.0140978167138854, -0.5622823525984408377 ) ) ;
#20310 = CIRCLE ( 'NONE', #29558, 14.00000000000000000 ) ;
#20311 = CIRCLE ( 'NONE', #34148, 20.00000000000000355 ) ;
#20312 = UNCERTAINTY_MEASURE_WITH_UNIT (LENGTH_MEASURE( 1.000000000000000082E-05 ), #8983, 'distance_accuracy_value', 'NONE');
#20313 = CARTESIAN_POINT ( 'NONE',  ( 0.000000000000000000, -7.317194182740013098, -18.61340026142654480 ) ) ;
#20314 = ORIENTED_EDGE ( 'NONE', *, *, #3778, .T. ) ;
#20315 = CARTESIAN_POINT ( 'NONE',  ( -38.00000000000000711, -114.9929510916434339, 10.50625754673587231 ) ) ;
#20316 = EDGE_CURVE ( 'NONE', #29062, #15120, #10939, .T. ) ;
#20317 = ADVANCED_FACE ( 'NONE', ( #22545 ), #33192, .F. ) ;
#20318 = VECTOR ( 'NONE', #27338, 1000.000000000000000 ) ;
#20319 = CARTESIAN_POINT ( 'NONE',  ( -39.00000000000000000, -113.9929510916434339, 12.17846912687782179 ) ) ;
#20320 = DIRECTION ( 'NONE',  ( 0.000000000000000000, 0.000000000000000000, 1.000000000000000000 ) ) ;
#20321 = LINE ( 'NONE', #29180, #12245 ) ;
#20322 = CARTESIAN_POINT ( 'NONE',  ( -37.88878409051687157, -113.9929510916434339, 14.07058620477052280 ) ) ;
#20323 = DIRECTION ( 'NONE',  ( -1.783119874454246424E-31, -1.187911941725854497E-31, 1.000000000000000000 ) ) ;
#20324 = CARTESIAN_POINT ( 'NONE',  ( -35.50000000000000711, -114.9929510916434339, 12.53051367006571581 ) ) ;
#20325 = CARTESIAN_POINT ( 'NONE',  ( 8.000000000000007105, 5.363026430117337817, -9.919332006307165273 ) ) ;
#20326 = VERTEX_POINT ( 'NONE', #3314 ) ;
#20327 = CARTESIAN_POINT ( 'NONE',  ( 1.799999999999996936, -4.652013227827197341E-14, 8.000000000000024869 ) ) ;
#20328 = DIRECTION ( 'NONE',  ( -1.000000000000000000, 0.000000000000000000, 0.000000000000000000 ) ) ;
#20329 = ORIENTED_EDGE ( 'NONE', *, *, #11627, .T. ) ;
#20330 = CARTESIAN_POINT ( 'NONE',  ( -35.50040135968785648, -114.9929510916434339, 12.63896776382214071 ) ) ;
#20331 = ORIENTED_EDGE ( 'NONE', *, *, #31451, .T. ) ;
#20332 = CARTESIAN_POINT ( 'NONE',  ( -44.00199999999999534, -1.144142364505046046E-15, -3.000000000000002665 ) ) ;
#20333 = ORIENTED_EDGE ( 'NONE', *, *, #18309, .F. ) ;
#20334 = CARTESIAN_POINT ( 'NONE',  ( -39.49999999999999289, 7.019851009788996343, 105.5074730863398003 ) ) ;
#20335 = ORIENTED_EDGE ( 'NONE', *, *, #25330, .T. ) ;
#20336 = VECTOR ( 'NONE', #4710, 1000.000000000000000 ) ;
#20337 = CARTESIAN_POINT ( 'NONE',  ( -35.50000000000000000, -113.0140978167138712, -0.5622823525984297355 ) ) ;
#20338 = DIRECTION ( 'NONE',  ( 1.000000000000000000, 0.000000000000000000, 0.000000000000000000 ) ) ;
#20339 = CARTESIAN_POINT ( 'NONE',  ( -35.00000000000000000, -114.0592624029313242, 9.003524454178448266 ) ) ;
#20340 = ADVANCED_FACE ( 'NONE', ( #11745 ), #2797, .T. ) ;
#20341 = ORIENTED_EDGE ( 'NONE', *, *, #5842, .F. ) ;
#20342 = CARTESIAN_POINT ( 'NONE',  ( -38.37230871539094323, -112.5438815906447729, 3.941024454178448710 ) ) ;
#20343 = CARTESIAN_POINT ( 'NONE',  ( 7.999999999999992895, -51.93417535146740960, -2.615612846549736581 ) ) ;
#20344 = CARTESIAN_POINT ( 'NONE',  ( -35.50000000000000711, -114.8057644833805568, -1.624782352598427959 ) ) ;
#20345 = VERTEX_POINT ( 'NONE', #24739 ) ;
#20346 = ORIENTED_EDGE ( 'NONE', *, *, #35015, .F. ) ;
#20347 = DIRECTION ( 'NONE',  ( -1.000000000000000000, 0.000000000000000000, 0.000000000000000000 ) ) ;
#20348 = DIRECTION ( 'NONE',  ( -1.000000000000000000, -0.000000000000000000, -0.000000000000000000 ) ) ;
#20349 = ORIENTED_EDGE ( 'NONE', *, *, #28519, .F. ) ;
#20350 = VERTEX_POINT ( 'NONE', #2963 ) ;
#20351 = CARTESIAN_POINT ( 'NONE',  ( -34.50000000000000000, -113.4307644833805000, -1.624782352598427959 ) ) ;
#20352 = CARTESIAN_POINT ( 'NONE',  ( -35.50000000000000711, -113.3557509229967764, 1.923098431109107054 ) ) ;
#20353 = ORIENTED_EDGE ( 'NONE', *, *, #35297, .T. ) ;
#20354 = ORIENTED_EDGE ( 'NONE', *, *, #17363, .F. ) ;
#20355 = DIRECTION ( 'NONE',  ( -1.000000000000000000, -1.836970198721029934E-16, -0.000000000000000000 ) ) ;
#20356 = AXIS2_PLACEMENT_3D ( 'NONE', #15393, #2459, #26765 ) ;
#20357 = EDGE_CURVE ( 'NONE', #779, #15796, #8688, .T. ) ;
#20358 = CARTESIAN_POINT ( 'NONE',  ( -37.80727372874345349, -113.9929510916434339, 13.01835785830664705 ) ) ;
#20359 = CARTESIAN_POINT ( 'NONE',  ( -36.49999999999999289, -6.699660887819688604, 116.5112005972652014 ) ) ;
#20360 = CARTESIAN_POINT ( 'NONE',  ( 50.00000000000000000, 10.00000000000000888, 120.0000000000000000 ) ) ;
#20361 = CARTESIAN_POINT ( 'NONE',  ( -35.50005019975638021, -113.9929510916434339, 12.62670525340498351 ) ) ;
#20362 = AXIS2_PLACEMENT_3D ( 'NONE', #27373, #33123, #8449 ) ;
#20364 = CARTESIAN_POINT ( 'NONE',  ( -35.50000000000000000, -115.9929510916434481, 12.57451923796416260 ) ) ;
#20363 = B_SPLINE_CURVE_WITH_KNOTS ( 'NONE', 3,
 ( #13359, #32972, #10838, #2028, #21794, #32437, #18393, #32792, #35158, #13190, #29396, #10477, #23991, #13533, #26874, #24164, #7585, #24341, #7758, #4907, #18741, #4741, #15677, #10303, #16381, #24517, #13001, #21440, #35332, #21266, #19095, #18573, #29573, #15849, #2222, #29746, #18921, #2753, #16030, #8114, #10654, #21609, #32614, #7942, #30095, #29923, #5433, #5265, #24692, #27225, #27399, #16202, #2566, #13713, #20, #6300, #11532, #19776, #19961, #8646, #19612, #19265, #17270, #25040, #33145, #8475, #33319, #3089, #24864, #19454, #30787, #543, #33487, #25224, #193, #5951, #28273, #16741, #28100, #11361, #22500, #11698, #896, #361, #8815, #3262, #22149, #30968, #27748, #6126, #27915, #22325, #30454, #11178, #8287, #30270, #5783, #3616, #3444, #5613, #14043, #11876, #17093, #30616, #25402, #25578, #16908, #14565, #14224, #14394, #715, #22854, #22668, #16575, #33658, #8992, #27581, #2920, #13878, #26284, #3792, #15095, #20501, #23217, #20675, #14921, #3979, #7005, #34207, #28634, #17626, #1624, #28449, #28805, #9176, #7184, #25934, #23033, #34032, #9537, #1257, #9356, #31672, #26107, #23399, #1436, #25759, #31511, #18164, #6652, #17981, #12242, #12414, #4522, #28982, #33850, #31324, #20315 ),
 .UNSPECIFIED., .F., .F.,
 ( 4, 2, 2, 2, 2, 2, 2, 2, 2, 2, 2, 2, 2, 2, 2, 2, 2, 2, 2, 2, 2, 2, 2, 2, 2, 2, 2, 2, 2, 2, 2, 2, 2, 2, 2, 2, 2, 2, 2, 2, 2, 2, 2, 2, 2, 2, 2, 2, 2, 2, 2, 2, 2, 2, 2, 2, 2, 2, 2, 2, 2, 2, 2, 2, 2, 2, 2, 2, 2, 2, 2, 2, 2, 2, 2, 2, 2, 2, 4 ),
 ( 0.000000000000000000, 0.005381740036788157898, 0.008072610055182236413, 0.009418045064379276105, 0.01009076256897779508, 0.01076348007357631580, 0.01185104180586291078, 0.01293860353814950404, 0.01511372700272269054, 0.01946397393186906355, 0.02816446779016181304, 0.04556545550674730855, 0.08036743093991829956, 0.1151694063730892975, 0.1325703940896748034, 0.1412708879479675494, 0.1456211348771139225, 0.1477962583416871090, 0.1488838200739737161, 0.1499713818062602955, 0.1507624401091536004, 0.1515534984120469053, 0.1531356150178334874, 0.1562998482294066793, 0.1626283146525530909, 0.1752852474988458864, 0.2005991131914315051, 0.2512268445766027147, 0.3018545759617738966, 0.3271684416543594875, 0.3398253745006523108, 0.3461538409237986946, 0.3493180741353718588, 0.3509001907411584686, 0.3524823073469450785, 0.3548354025267266287, 0.3571884977065081790, 0.3618946880660712795, 0.3713070687851974805, 0.3901318302234498825, 0.4277813530999547420, 0.4654308759764596015, 0.4842556374147120035, 0.4936680181338382045, 0.4983742084934013050, 0.5007273036731828553, 0.5030803988529644055, 0.5053274392295320494, 0.5075744796060996933, 0.5120685603592350921, 0.5210567218655057786, 0.5390330448780472627, 0.5749856909031301200, 0.6109383369282129772, 0.6289146599407544613, 0.6379028214470251479, 0.6423969022001605467, 0.6446439425767281906, 0.6468909829532958344, 0.6492440781330773847, 0.6515971733128589349, 0.6563033636724220354, 0.6657157443915482364, 0.6845405058298006384, 0.7221900287063054424, 0.7598395515828102464, 0.7786643130210626484, 0.7880766937401888494, 0.7927828840997519499, 0.7951359792795336112, 0.7974890744593151615, 0.7990711910651018268, 0.8006533076708883812, 0.8038175408824614898, 0.8101460073056079292, 0.8228029401519008079, 0.8481168058444863433, 0.8987445372296576362, 1.000000000000000000 ),
 .UNSPECIFIED. ) ;
#20365 = UNCERTAINTY_MEASURE_WITH_UNIT (LENGTH_MEASURE( 1.000000000000000082E-05 ), #10687, 'distance_accuracy_value', 'NONE');
#20366 = CARTESIAN_POINT ( 'NONE',  ( -42.49999999999999289, -25.98076211353320986, 84.99999999999994316 ) ) ;
#20367 = DIRECTION ( 'NONE',  ( 0.000000000000000000, 0.3420201433256629397, 0.9396926207859104263 ) ) ;
#20368 = EDGE_CURVE ( 'NONE', #29056, #35356, #1759, .T. ) ;
#20369 = CARTESIAN_POINT ( 'NONE',  ( 0.000000000000000000, -9.919332006307138627, -5.363026430117212584 ) ) ;
#20370 = DIRECTION ( 'NONE',  ( 1.000000000000000000, -0.000000000000000000, -0.000000000000000000 ) ) ;
#20371 = LINE ( 'NONE', #34089, #27221 ) ;
#20372 = ORIENTED_EDGE ( 'NONE', *, *, #28839, .T. ) ;
#20373 = DIRECTION ( 'NONE',  ( 1.000000000000000000, -0.000000000000000000, -0.000000000000000000 ) ) ;
#20374 = DIRECTION ( 'NONE',  ( 0.000000000000000000, 0.000000000000000000, -1.000000000000000000 ) ) ;
#20375 = DIRECTION ( 'NONE',  ( -1.000000000000000000, 0.000000000000000000, 0.000000000000000000 ) ) ;
#20376 = DIRECTION ( 'NONE',  ( -1.000000000000000000, 0.000000000000000000, -0.000000000000000000 ) ) ;
#20377 = CARTESIAN_POINT ( 'NONE',  ( 8.000000000000000000, 0.000000000000000000, 0.000000000000000000 ) ) ;
#20378 = VERTEX_POINT ( 'NONE', #22368 ) ;
#20379 = CIRCLE ( 'NONE', #18113, 47.49900000000001654 ) ;
#20380 = DIRECTION ( 'NONE',  ( 1.000000000000000000, 0.000000000000000000, -1.691777834109591064E-31 ) ) ;
#20381 = VECTOR ( 'NONE', #11620, 1000.000000000000000 ) ;
#20382 = CARTESIAN_POINT ( 'NONE',  ( -34.50000000000000000, -114.1807644833817648, -2.624782352598442614 ) ) ;
#20383 = CARTESIAN_POINT ( 'NONE',  ( -34.49999999999998579, -12.06135120645816983, 86.49999999999994316 ) ) ;
#20384 = ORIENTED_EDGE ( 'NONE', *, *, #2464, .F. ) ;
#20385 = VERTEX_POINT ( 'NONE', #22022 ) ;
#20386 = CARTESIAN_POINT ( 'NONE',  ( -37.97545270896702618, -114.4734759653044023, 9.152725545821551734 ) ) ;
#20387 = ORIENTED_EDGE ( 'NONE', *, *, #7733, .T. ) ;
#20388 = CIRCLE ( 'NONE', #11220, 19.99999999999998579 ) ;
#20389 = FILL_AREA_STYLE ('',( #9431 ) ) ;
#20390 = ORIENTED_EDGE ( 'NONE', *, *, #33326, .T. ) ;
#20391 = ORIENTED_EDGE ( 'NONE', *, *, #27489, .T. ) ;
#20392 = CARTESIAN_POINT ( 'NONE',  ( -35.50000000000000000, -115.0140978167137860, -0.6247823525984395054 ) ) ;
#20393 = CIRCLE ( 'NONE', #5474, 7.199999999999991296 ) ;
#20394 = CARTESIAN_POINT ( 'NONE',  ( -39.49999999999999289, -14.67619866229204284, 93.25874355921412473 ) ) ;
#20395 = CARTESIAN_POINT ( 'NONE',  ( 8.000000000000000000, 16.94522934049224361, -8.128228055638670568 ) ) ;
#20396 = ADVANCED_FACE ( 'NONE', ( #16615 ), #33018, .T. ) ;
#20397 = CARTESIAN_POINT ( 'NONE',  ( -35.50000000000000711, -114.9929510916434339, 11.91443571948719971 ) ) ;
#20398 = CARTESIAN_POINT ( 'NONE',  ( 7.999999999999992895, -47.32430374665916872, -21.55018039121578255 ) ) ;
#20399 = EDGE_CURVE ( 'NONE', #5280, #5287, #27798, .T. ) ;
#20400 = DIRECTION ( 'NONE',  ( 0.000000000000000000, -6.938893903907204958E-17, -1.000000000000000000 ) ) ;
#20401 = CARTESIAN_POINT ( 'NONE',  ( -36.87500000000098055, -114.9929510916434339, 14.11852480586264846 ) ) ;
#20402 = CARTESIAN_POINT ( 'NONE',  ( 46.00000000000000000, -25.98076211353320275, 95.99999999999991473 ) ) ;
#20403 = PRODUCT_DEFINITION_SHAPE ( 'NONE', 'NONE',  #35618 ) ;
#20404 = CIRCLE ( 'NONE', #5516, 52.00000000000000711 ) ;
#20405 = UNCERTAINTY_MEASURE_WITH_UNIT (LENGTH_MEASURE( 1.000000000000000082E-05 ), #18133, 'distance_accuracy_value', 'NONE');
#20406 = DIRECTION ( 'NONE',  ( 0.000000000000000000, -0.9848077530122096857, 0.1736481776669211718 ) ) ;
#20407 = ORIENTED_EDGE ( 'NONE', *, *, #21430, .T. ) ;
#20408 = EDGE_CURVE ( 'NONE', #9203, #5782, #13833, .T. ) ;
#20409 = CARTESIAN_POINT ( 'NONE',  ( -35.50000000000000000, -114.8124184834118324, 8.677834500183694288 ) ) ;
#20410 = CARTESIAN_POINT ( 'NONE',  ( -35.50000000000000711, -112.0140978167138712, -0.3747823525984256832 ) ) ;
#20411 = SURFACE_SIDE_STYLE ('',( #31423 ) ) ;
#20412 = DIRECTION ( 'NONE',  ( 0.000000000000000000, 0.4999999999999898415, 0.8660254037844444808 ) ) ;
#20413 = CIRCLE ( 'NONE', #23312, 20.00000000000000355 ) ;
#20414 = DIRECTION ( 'NONE',  ( -1.000000000000000000, 0.000000000000000000, 0.000000000000000000 ) ) ;
#20415 = CARTESIAN_POINT ( 'NONE',  ( -3.799999999999999822, 4.382607293638566128E-16, 38.00000000000000711 ) ) ;
#20416 = DIRECTION ( 'NONE',  ( -1.000000000000000000, -0.000000000000000000, -0.000000000000000000 ) ) ;
#20417 = CARTESIAN_POINT ( 'NONE',  ( -44.00000000000000000, 3.711905462088098291E-31, 0.000000000000000000 ) ) ;
#20418 = CARTESIAN_POINT ( 'NONE',  ( 0.000000000000000000, 3.753907720749211308, -8.725776631572673026 ) ) ;
#20419 = ORIENTED_EDGE ( 'NONE', *, *, #21207, .T. ) ;
#20420 = CARTESIAN_POINT ( 'NONE',  ( -37.35495115944176803, -115.0245472910329880, 5.965225545821550845 ) ) ;
#20421 = LINE ( 'NONE', #26038, #23900 ) ;
#20422 = CARTESIAN_POINT ( 'NONE',  ( 0.000000000000000000, 0.000000000000000000, -40.89999999999999858 ) ) ;
#20423 = ORIENTED_EDGE ( 'NONE', *, *, #1106, .T. ) ;
#20424 = CIRCLE ( 'NONE', #3785, 20.00000000000000711 ) ;
#20425 = VERTEX_POINT ( 'NONE', #17140 ) ;
#20426 = CARTESIAN_POINT ( 'NONE',  ( 0.000000000000000000, 0.000000000000000000, -44.50000000000000000 ) ) ;
#20427 = VERTEX_POINT ( 'NONE', #6347 ) ;
#20428 = CARTESIAN_POINT ( 'NONE',  ( -38.30190309005061522, -111.0245472910330022, 8.027725545821551734 ) ) ;
#20429 = ORIENTED_EDGE ( 'NONE', *, *, #1133, .F. ) ;
#20430 = ADVANCED_FACE ( 'NONE', ( #30321 ), #28146, .T. ) ;
#20431 = DIRECTION ( 'NONE',  ( 1.783119874454246424E-31, 1.187911941725854497E-31, -1.000000000000000000 ) ) ;
#20432 = DIRECTION ( 'NONE',  ( 1.000000000000000000, 0.000000000000000000, -0.000000000000000000 ) ) ;
#20433 = DIRECTION ( 'NONE',  ( 0.000000000000000000, 0.000000000000000000, -1.000000000000000000 ) ) ;
#20434 = VECTOR ( 'NONE', #26352, 1000.000000000000000 ) ;
#20435 = CARTESIAN_POINT ( 'NONE',  ( -46.00000000000000000, 0.000000000000000000, 70.00000000000000000 ) ) ;
#20436 = SHAPE_DEFINITION_REPRESENTATION ( #1183, #27563 ) ;
#20437 = AXIS2_PLACEMENT_3D ( 'NONE', #17861, #31561, #6887 ) ;
#20438 = AXIS2_PLACEMENT_3D ( 'NONE', #9249, #785, #30862 ) ;
#20439 = DIRECTION ( 'NONE',  ( 1.000000000000000000, -4.524158825347490025E-15, -1.174092375852883357E-15 ) ) ;
#20440 = ORIENTED_EDGE ( 'NONE', *, *, #16524, .T. ) ;
#20441 = ORIENTED_EDGE ( 'NONE', *, *, #3378, .F. ) ;
#20442 = AXIS2_PLACEMENT_3D ( 'NONE', #25334, #299, #27854 ) ;
#20443 = ADVANCED_FACE ( 'NONE', ( #25449 ), #9051, .T. ) ;
#20444 = CARTESIAN_POINT ( 'NONE',  ( 8.000000000000000000, 0.9861715913090087771, -17.47118961583601049 ) ) ;
#20445 = CARTESIAN_POINT ( 'NONE',  ( 7.999999999999992895, 7.162210897275726573, 51.50439529848831199 ) ) ;
#20446 = ADVANCED_FACE ( 'NONE', ( #237 ), #34746, .T. ) ;
#20447 = EDGE_CURVE ( 'NONE', #6690, #7164, #21895, .T. ) ;
#20448 = EDGE_LOOP ( 'NONE', ( #11090, #13306 ) ) ;
#20449 = FACE_OUTER_BOUND ( 'NONE', #28001, .T. ) ;
#20450 = AXIS2_PLACEMENT_3D ( 'NONE', #13849, #13502, #27718 ) ;
#20451 = CARTESIAN_POINT ( 'NONE',  ( -34.50000000000000000, -113.0349311500474982, -0.6247823525985715110 ) ) ;
#20452 = CYLINDRICAL_SURFACE ( 'NONE', #24820, 2.447112362156710574 ) ;
#20453 = CARTESIAN_POINT ( 'NONE',  ( -34.49999999999998579, -15.63316754279159326, 121.0048025873809792 ) ) ;
#20454 =( REPRESENTATION_RELATIONSHIP ('NONE','NONE', #26607, #2005 ) REPRESENTATION_RELATIONSHIP_WITH_TRANSFORMATION ( #9419 )SHAPE_REPRESENTATION_RELATIONSHIP( ) );
#20455 = CARTESIAN_POINT ( 'NONE',  ( -34.50000000000000000, -115.9920935318519923, 10.44577481630138749 ) ) ;
#20456 = DIRECTION ( 'NONE',  ( 1.000000000000000000, -0.000000000000000000, -0.000000000000000000 ) ) ;
#20457 = DIRECTION ( 'NONE',  ( 1.000000000000000000, 0.000000000000000000, 0.000000000000000000 ) ) ;
#20458 = EDGE_CURVE ( 'NONE', #21073, #8899, #10069, .T. ) ;
#20459 = CARTESIAN_POINT ( 'NONE',  ( -34.50000000000000000, -114.1556834383649459, 8.511484393387789282 ) ) ;
#20460 = DIRECTION ( 'NONE',  ( 0.02040816326530624572, 0.9997917317482359900, -1.513872302914096262E-31 ) ) ;
#20461 = ADVANCED_FACE ( 'NONE', ( #7715 ), #7378, .T. ) ;
#20462 = FACE_OUTER_BOUND ( 'NONE', #8297, .T. ) ;
#20463 = CARTESIAN_POINT ( 'NONE',  ( 8.000000000000007105, 3.753907720749211308, -8.725776631572673026 ) ) ;
#20464 = CARTESIAN_POINT ( 'NONE',  ( 5.400000000000071410, 0.9999999999999662492, -32.00000000000000000 ) ) ;
#20465 = VECTOR ( 'NONE', #5539, 1000.000000000000000 ) ;
#20466 = DIRECTION ( 'NONE',  ( 1.541976423090495140E-16, -1.000000000000000000, 0.000000000000000000 ) ) ;
#20467 = VERTEX_POINT ( 'NONE', #28496 ) ;
#20468 = CARTESIAN_POINT ( 'NONE',  ( -39.07941549657749647, -116.1632251905417803, 6.058975545821550845 ) ) ;
#20469 = AXIS2_PLACEMENT_3D ( 'NONE', #5271, #19105, #30102 ) ;
#20470 = DIRECTION ( 'NONE',  ( 0.000000000000000000, 1.000000000000000000, 3.497202527569241525E-15 ) ) ;
#20471 = AXIS2_PLACEMENT_3D ( 'NONE', #475, #25150, #19374 ) ;
#20472 = CARTESIAN_POINT ( 'NONE',  ( -35.50000000000000000, -113.0140978167139991, -0.6091573525984278481 ) ) ;
#20473 = VERTEX_POINT ( 'NONE', #29174 ) ;
#20474 = EDGE_LOOP ( 'NONE', ( #5627, #1661, #921, #31457 ) ) ;
#20475 = CARTESIAN_POINT ( 'NONE',  ( -4.000000000000000000, 0.000000000000000000, -33.50000000000000711 ) ) ;
#20476 = DIRECTION ( 'NONE',  ( 0.000000000000000000, 0.000000000000000000, -1.000000000000000000 ) ) ;
#20477 = ORIENTED_EDGE ( 'NONE', *, *, #15711, .F. ) ;
#20478 = AXIS2_PLACEMENT_3D ( 'NONE', #27844, #17190, #25144 ) ;
#20479 = EDGE_LOOP ( 'NONE', ( #27910, #3767, #5771, #17124 ) ) ;
#20481 = EDGE_LOOP ( 'NONE', ( #13431, #34591 ) ) ;
#20480 = CIRCLE ( 'NONE', #6700, 4.000000000000003553 ) ;
#20482 = EDGE_CURVE ( 'NONE', #3103, #23381, #7186, .T. ) ;
#20483 = AXIS2_PLACEMENT_3D ( 'NONE', #31073, #8918, #6399 ) ;
#20484 = CYLINDRICAL_SURFACE ( 'NONE', #18848, 11.00000000000001066 ) ;
#20485 = ADVANCED_FACE ( 'NONE', ( #3665 ), #33898, .T. ) ;
#20486 = CARTESIAN_POINT ( 'NONE',  ( -35.62769128460905677, -112.5438815906447729, 6.808975545821550845 ) ) ;
#20487 = ADVANCED_FACE ( 'NONE', ( #2179 ), #4524, .T. ) ;
#20488 = DIRECTION ( 'NONE',  ( 0.000000000000000000, 0.000000000000000000, 1.000000000000000000 ) ) ;
#20489 = VECTOR ( 'NONE', #26749, 1000.000000000000000 ) ;
#20490 = DIRECTION ( 'NONE',  ( -1.000000000000000000, 0.000000000000000000, 0.000000000000000000 ) ) ;
#20491 = AXIS2_PLACEMENT_3D ( 'NONE', #17057, #3755, #14359 ) ;
#20492 = VERTEX_POINT ( 'NONE', #13150 ) ;
#20493 = VERTEX_POINT ( 'NONE', #20359 ) ;
#20494 = CARTESIAN_POINT ( 'NONE',  ( -35.50000000000000000, -111.0140978167138570, -0.3747823525984258497 ) ) ;
#20495 = AXIS2_PLACEMENT_3D ( 'NONE', #19142, #18616, #21305 ) ;
#20496 = CARTESIAN_POINT ( 'NONE',  ( 8.000000000000000000, 0.000000000000000000, 0.000000000000000000 ) ) ;
#20497 = EDGE_CURVE ( 'NONE', #14462, #18380, #8684, .T. ) ;
#20498 = ADVANCED_FACE ( 'NONE', ( #6609 ), #14353, .T. ) ;
#20499 = CARTESIAN_POINT ( 'NONE',  ( -1.520000000000000906, 9.842294572325847517E-16, 5.016000000000010672 ) ) ;
#20500 = ORIENTED_EDGE ( 'NONE', *, *, #31555, .F. ) ;
#20501 = CARTESIAN_POINT ( 'NONE',  ( -37.54084996655477369, -114.9929510916434339, 13.11692036158760466 ) ) ;
#20502 = STYLED_ITEM ( 'NONE', ( #32574 ), #22365 ) ;
#20503 = AXIS2_PLACEMENT_3D ( 'NONE', #15379, #32318, #4259 ) ;
#20504 = VECTOR ( 'NONE', #5114, 1000.000000000000000 ) ;
#20505 = CARTESIAN_POINT ( 'NONE',  ( -39.00000000000000000, -113.9929510916434339, 12.59102132592609102 ) ) ;
#20506 = VECTOR ( 'NONE', #8225, 1000.000000000000000 ) ;
#20507 = CARTESIAN_POINT ( 'NONE',  ( -39.49999999999999289, -12.00833024919777081, 94.79903810567661537 ) ) ;
#20508 = AXIS2_PLACEMENT_3D ( 'NONE', #13988, #6066, #488 ) ;
#20509 = CARTESIAN_POINT ( 'NONE',  ( 7.999999999999992895, -44.75336757549767697, -14.30704879393654494 ) ) ;
#20510 = CARTESIAN_POINT ( 'NONE',  ( -39.00000000000000000, -113.9929510916434339, 12.60752341388803721 ) ) ;
#20511 = DIRECTION ( 'NONE',  ( 1.000000000000000000, 0.000000000000000000, 0.000000000000000000 ) ) ;
#20512 = VECTOR ( 'NONE', #6329, 1000.000000000000000 ) ;
#20513 = EDGE_CURVE ( 'NONE', #12757, #8637, #26498, .T. ) ;
#20514 = CARTESIAN_POINT ( 'NONE',  ( -35.52552712174884419, -114.9929510916434339, 12.77960891308624447 ) ) ;
#20515 = FACE_OUTER_BOUND ( 'NONE', #15354, .T. ) ;
#20516 = ORIENTED_EDGE ( 'NONE', *, *, #11450, .F. ) ;
#20517 = CARTESIAN_POINT ( 'NONE',  ( 8.000000000000000000, 11.06713717293239441, 13.55483219355733837 ) ) ;
#20518 = DIRECTION ( 'NONE',  ( 0.000000000000000000, 0.000000000000000000, -1.000000000000000000 ) ) ;
#20519 = ORIENTED_EDGE ( 'NONE', *, *, #23320, .F. ) ;
#20520 = CARTESIAN_POINT ( 'NONE',  ( -35.50000000000000711, -114.9929510916434339, 12.59652202191340642 ) ) ;
#20521 = EDGE_LOOP ( 'NONE', ( #1473, #10813, #33482, #31267 ) ) ;
#20522 = CARTESIAN_POINT ( 'NONE',  ( 0.000000000000000000, -32.32520163883559405, -34.09746168776067776 ) ) ;
#20523 = VECTOR ( 'NONE', #27843, 1000.000000000000000 ) ;
#20524 = VERTEX_POINT ( 'NONE', #12022 ) ;
#20525 = DIRECTION ( 'NONE',  ( -1.000000000000000000, 0.000000000000000000, 0.000000000000000000 ) ) ;
#20526 = ORIENTED_EDGE ( 'NONE', *, *, #20697, .F. ) ;
#20527 = VECTOR ( 'NONE', #8866, 1000.000000000000000 ) ;
#20528 = CARTESIAN_POINT ( 'NONE',  ( -34.50000000000000000, -112.9990795116828650, 0.8734249692896993711 ) ) ;
#20529 = CARTESIAN_POINT ( 'NONE',  ( 8.000000000000007105, 5.908880290975540461, 9.604183132802438294 ) ) ;
#20530 = DIRECTION ( 'NONE',  ( 0.000000000000000000, -0.5877852522924624790, -0.8090169943749551118 ) ) ;
#20531 = ORIENTED_EDGE ( 'NONE', *, *, #8396, .F. ) ;
#20532 = CARTESIAN_POINT ( 'NONE',  ( -35.62769128460905677, -115.4561184093552413, 6.191024454178448266 ) ) ;
#20533 = AXIS2_PLACEMENT_3D ( 'NONE', #3863, #20025, #25464 ) ;
#20534 = EDGE_CURVE ( 'NONE', #209, #19897, #25186, .T. ) ;
#20535 = EDGE_CURVE ( 'NONE', #4534, #8762, #21300, .T. ) ;
#20536 = DIRECTION ( 'NONE',  ( -1.000000000000000000, 0.000000000000000000, 0.000000000000000000 ) ) ;
#20537 = CARTESIAN_POINT ( 'NONE',  ( -35.50000000000000711, -112.0140978167138712, -0.1247823525984259746 ) ) ;
#20538 = EDGE_LOOP ( 'NONE', ( #1607, #6768, #13183, #17223 ) ) ;
#20540 = EDGE_LOOP ( 'NONE', ( #4287, #24675, #3466, #32114 ) ) ;
#20539 = EDGE_CURVE ( 'NONE', #4854, #3615, #33388, .T. ) ;
#20541 = AXIS2_PLACEMENT_3D ( 'NONE', #15204, #20786, #26039 ) ;
#20542 = DIRECTION ( 'NONE',  ( -1.000000000000000000, 0.000000000000000000, 0.000000000000000000 ) ) ;
#20543 = AXIS2_PLACEMENT_3D ( 'NONE', #982, #11961, #3511 ) ;
#20544 = FILL_AREA_STYLE_COLOUR ( '', #20186 ) ;
#20545 = DIRECTION ( 'NONE',  ( -1.000000000000000000, -1.836970198721029934E-16, -0.000000000000000000 ) ) ;
#20546 = VERTEX_POINT ( 'NONE', #33449 ) ;
#20547 = ORIENTED_EDGE ( 'NONE', *, *, #18188, .T. ) ;
#20548 = CARTESIAN_POINT ( 'NONE',  ( -34.50000000000000000, -113.1807644833805426, -1.624782352598427959 ) ) ;
#20549 = CARTESIAN_POINT ( 'NONE',  ( -35.50000000000000711, -112.6043641208289188, 1.789429170677330649 ) ) ;
#20550 = EDGE_CURVE ( 'NONE', #19239, #19089, #22450, .T. ) ;
#20551 = ORIENTED_EDGE ( 'NONE', *, *, #9265, .T. ) ;
#20552 = EDGE_LOOP ( 'NONE', ( #6295, #31690, #8577, #5484 ) ) ;
#20553 = ADVANCED_FACE ( 'NONE', ( #6435, #11486 ), #6263, .T. ) ;
#20554 = DIRECTION ( 'NONE',  ( 0.000000000000000000, 0.000000000000000000, 1.000000000000000000 ) ) ;
#20555 = VECTOR ( 'NONE', #111, 1000.000000000000000 ) ;
#20556 = CARTESIAN_POINT ( 'NONE',  ( -36.06250000000000711, -113.9929510916434339, 13.11852480586264846 ) ) ;
#20557 = DIRECTION ( 'NONE',  ( -1.000000000000000000, 0.000000000000000000, 0.000000000000000000 ) ) ;
#20558 = CARTESIAN_POINT ( 'NONE',  ( -36.99999999999988631, -113.9929510916434339, 13.11852480586264846 ) ) ;
#20559 = CIRCLE ( 'NONE', #4512, 20.00000000000000355 ) ;
#20560 = CARTESIAN_POINT ( 'NONE',  ( -35.50000000000000000, -115.9929510916434481, 10.51725893871049067 ) ) ;
#20561 = DIRECTION ( 'NONE',  ( -1.000000000000000000, 0.000000000000000000, 0.000000000000000000 ) ) ;
#20562 = CIRCLE ( 'NONE', #2207, 52.00000000000000711 ) ;
#20563 = CARTESIAN_POINT ( 'NONE',  ( -2.141980652367370119, -6.189445006155602336, 0.000000000000000000 ) ) ;
#20564 = DIRECTION ( 'NONE',  ( -1.000000000000000000, -0.000000000000000000, -0.000000000000000000 ) ) ;
#20565 = DIRECTION ( 'NONE',  ( 0.000000000000000000, 0.000000000000000000, -1.000000000000000000 ) ) ;
#20566 = AXIS2_PLACEMENT_3D ( 'NONE', #6630, #31129, #11342 ) ;
#20567 = CARTESIAN_POINT ( 'NONE',  ( 5.400000000000071410, 0.9999999999999662492, -44.50000000000000000 ) ) ;
#20568 = ORIENTED_EDGE ( 'NONE', *, *, #18109, .T. ) ;
#20569 = DIRECTION ( 'NONE',  ( -1.174092375852890260E-15, 4.222049128630259891E-16, 1.000000000000000000 ) ) ;
#20570 = CARTESIAN_POINT ( 'NONE',  ( -35.50000000000000711, -112.0140978167138712, -0.1247823525984259746 ) ) ;
#20571 = DIRECTION ( 'NONE',  ( -0.000000000000000000, -0.2588190451025194627, -0.9659258262890686453 ) ) ;
#20572 = ITEM_DEFINED_TRANSFORMATION ( 'NONE', 'NONE', #627,  #21307 ) ;
#20573 = DIRECTION ( 'NONE',  ( 5.339440136655842133E-16, 1.000000000000000000, -1.918536189538073087E-16 ) ) ;
#20574 = DIRECTION ( 'NONE',  ( 0.000000000000000000, 0.000000000000000000, 1.000000000000000000 ) ) ;
#20575 = ORIENTED_EDGE ( 'NONE', *, *, #30449, .F. ) ;
#20576 = ADVANCED_FACE ( 'NONE', ( #17582 ), #28233, .T. ) ;
#20577 = CARTESIAN_POINT ( 'NONE',  ( -37.49999999999999289, -11.52052244843579309, 115.1848168619253698 ) ) ;
#20578 = CARTESIAN_POINT ( 'NONE',  ( -34.50000000000000000, -114.5974311500472567, -2.624782352598442614 ) ) ;
#20579 = DIRECTION ( 'NONE',  ( 0.000000000000000000, -0.8443279255020087470, -0.5358267949790064266 ) ) ;
#20580 = EDGE_LOOP ( 'NONE', ( #8620, #7415, #27518, #3599 ) ) ;
#20581 = EDGE_LOOP ( 'NONE', ( #18242, #21439, #28480, #5506 ) ) ;
#20582 = CARTESIAN_POINT ( 'NONE',  ( -36.02454729103297382, -113.5265240346956261, 9.902725545821553510 ) ) ;
#20583 = ORIENTED_EDGE ( 'NONE', *, *, #33770, .F. ) ;
#20584 = SHAPE_REPRESENTATION_RELATIONSHIP ( 'NONE' , 'NONE' ,  #7982, #6921 ) ;
#20585 = ORIENTED_EDGE ( 'NONE', *, *, #19823, .F. ) ;
#20586 = ORIENTED_EDGE ( 'NONE', *, *, #20550, .T. ) ;
#20587 = AXIS2_PLACEMENT_3D ( 'NONE', #30493, #31007, #583 ) ;
#20588 = CARTESIAN_POINT ( 'NONE',  ( -34.50000000000000000, -113.0140978167138712, 0.8752176474013583229 ) ) ;
#20589 = CIRCLE ( 'NONE', #25217, 3.799999999999999822 ) ;
#20590 = CARTESIAN_POINT ( 'NONE',  ( 0.000000000000000000, 0.000000000000000000, 65.00000000000000000 ) ) ;
#20591 = LINE ( 'NONE', #26017, #5326 ) ;
#20592 = CARTESIAN_POINT ( 'NONE',  ( -36.62499999999902656, -114.9929510916434339, 13.11852480586264669 ) ) ;
#20593 = DIRECTION ( 'NONE',  ( -0.000000000000000000, 0.000000000000000000, -1.000000000000000000 ) ) ;
#20594 = CARTESIAN_POINT ( 'NONE',  ( -36.24999999999983658, -114.9929510916434339, 14.11852480586264846 ) ) ;
#20595 = CARTESIAN_POINT ( 'NONE',  ( 8.000000000000007105, 3.975523202428290936, -13.42368113696666754 ) ) ;
#20596 = FACE_OUTER_BOUND ( 'NONE', #12228, .T. ) ;
#20597 = VERTEX_POINT ( 'NONE', #17052 ) ;
#20598 = CIRCLE ( 'NONE', #7395, 20.00000000000000355 ) ;
#20599 = CARTESIAN_POINT ( 'NONE',  ( -37.50613590685470911, -115.9929510916434481, 13.11852378322482515 ) ) ;
#20600 = CARTESIAN_POINT ( 'NONE',  ( -35.50000000000000711, -114.9724313160460696, -1.624792769101446765 ) ) ;
#20601 = CARTESIAN_POINT ( 'NONE',  ( 8.000000000000000000, -14.80634052301628145, 8.177498406287162069 ) ) ;
#20602 = FACE_OUTER_BOUND ( 'NONE', #34267, .T. ) ;
#20603 = CARTESIAN_POINT ( 'NONE',  ( 4.000000000000003553, 40.47821179127715396, 32.64221760512774040 ) ) ;
#20604 = DIRECTION ( 'NONE',  ( 1.000000000000000000, 0.000000000000000000, 0.000000000000000000 ) ) ;
#20605 = CYLINDRICAL_SURFACE ( 'NONE', #965, 52.00000000000000711 ) ;
#20606 = DIRECTION ( 'NONE',  ( -1.000000000000000000, 0.000000000000000000, 0.000000000000000000 ) ) ;
#20607 = EDGE_LOOP ( 'NONE', ( #14278, #5032, #28437, #15913 ) ) ;
#20608 = CARTESIAN_POINT ( 'NONE',  ( -36.25098837183130485, -114.6652019342044184, 8.683975545821549957 ) ) ;
#20609 = DIRECTION ( 'NONE',  ( -1.000000000000000000, -0.000000000000000000, -0.000000000000000000 ) ) ;
#20610 = LINE ( 'NONE', #20249, #31479 ) ;
#20611 = ORIENTED_EDGE ( 'NONE', *, *, #13536, .T. ) ;
#20612 = ORIENTED_EDGE ( 'NONE', *, *, #20073, .T. ) ;
#20613 = EDGE_CURVE ( 'NONE', #29380, #28214, #11545, .T. ) ;
#20614 = SURFACE_STYLE_USAGE ( .BOTH. , #29101 ) ;
#20615 = FACE_OUTER_BOUND ( 'NONE', #8096, .T. ) ;
#20616 = ORIENTED_EDGE ( 'NONE', *, *, #23294, .T. ) ;
#20617 = CARTESIAN_POINT ( 'NONE',  ( -40.02454729103296671, -112.8166217158120332, 9.340225545821551734 ) ) ;
#20618 = ORIENTED_EDGE ( 'NONE', *, *, #3378, .T. ) ;
#20619 = DIRECTION ( 'NONE',  ( 0.000000000000000000, 0.000000000000000000, 1.000000000000000000 ) ) ;
#20620 = CARTESIAN_POINT ( 'NONE',  ( 0.000000000000000000, -11.46872990052412611, 45.56340405422440654 ) ) ;
#20621 = CARTESIAN_POINT ( 'NONE',  ( 7.999999999999992895, -32.00046193115173310, 34.40241257139674502 ) ) ;
#20622 = VECTOR ( 'NONE', #34701, 1000.000000000000000 ) ;
#20623 = EDGE_CURVE ( 'NONE', #26766, #3989, #10960, .T. ) ;
#20624 = DIRECTION ( 'NONE',  ( 0.000000000000000000, 0.000000000000000000, -1.000000000000000000 ) ) ;
#20625 = ORIENTED_EDGE ( 'NONE', *, *, #14323, .F. ) ;
#20626 = ORIENTED_EDGE ( 'NONE', *, *, #32387, .T. ) ;
#20627 = DIRECTION ( 'NONE',  ( -1.000000000000000000, 0.000000000000000000, 0.000000000000000000 ) ) ;
#20628 = DIRECTION ( 'NONE',  ( -1.000000000000000000, -0.000000000000000000, -0.000000000000000000 ) ) ;
#20629 = ORIENTED_EDGE ( 'NONE', *, *, #18394, .T. ) ;
#20630 = LINE ( 'NONE', #15228, #13090 ) ;
#20631 = CIRCLE ( 'NONE', #25264, 20.00000000000000711 ) ;
#20632 = DIRECTION ( 'NONE',  ( 0.000000000000000000, 0.000000000000000000, 1.000000000000000000 ) ) ;
#20633 = CARTESIAN_POINT ( 'NONE',  ( -34.49999999999998579, -24.48076211353329157, 98.99999999999994316 ) ) ;
#20634 = CARTESIAN_POINT ( 'NONE',  ( -35.87745010033553683, -115.9929510916434481, 14.11371147303761475 ) ) ;
#20635 = DIRECTION ( 'NONE',  ( -1.174092375852890260E-15, 4.222049128630259891E-16, 1.000000000000000000 ) ) ;
#20636 = DIRECTION ( 'NONE',  ( -1.000000000000000000, 0.000000000000000000, 0.000000000000000000 ) ) ;
#20637 = CARTESIAN_POINT ( 'NONE',  ( -39.00000000000000711, -114.9929510916434339, 10.85830208992306822 ) ) ;
#20638 = LINE ( 'NONE', #29659, #32031 ) ;
#20639 = ADVANCED_FACE ( 'NONE', ( #25360, #14705 ), #25718, .T. ) ;
#20640 = CARTESIAN_POINT ( 'NONE',  ( 7.999999999999992895, -37.91532898920900863, -28.61088654061680359 ) ) ;
#20641 = CARTESIAN_POINT ( 'NONE',  ( 3.799999999999999822, -2.710505431213761085E-17, 29.09999999999999787 ) ) ;
#20642 = CARTESIAN_POINT ( 'NONE',  ( -42.49999999999999289, -24.48076211353329157, 98.99999999999994316 ) ) ;
#20643 = DIRECTION ( 'NONE',  ( 0.000000000000000000, 0.000000000000000000, 1.000000000000000000 ) ) ;
#20644 = DIRECTION ( 'NONE',  ( 1.000000000000000000, -5.339440136655842133E-16, -1.047965281155519420E-16 ) ) ;
#20645 = EDGE_LOOP ( 'NONE', ( #22494, #9196, #26267, #12686 ) ) ;
#20646 = CIRCLE ( 'NONE', #11469, 19.99999999999998579 ) ;
#20647 = CARTESIAN_POINT ( 'NONE',  ( -35.69809690994941320, -116.9754527089670546, 2.777725545821551734 ) ) ;
#20648 = CARTESIAN_POINT ( 'NONE',  ( 7.999999999999992895, 0.000000000000000000, 0.000000000000000000 ) ) ;
#20649 = CARTESIAN_POINT ( 'NONE',  ( -35.50000000000000000, -113.0140978167142833, 0.8752176474015604946 ) ) ;
#20650 = ORIENTED_EDGE ( 'NONE', *, *, #31158, .T. ) ;
#20651 = AXIS2_PLACEMENT_3D ( 'NONE', #1804, #31852, #29171 ) ;
#20652 = ORIENTED_EDGE ( 'NONE', *, *, #724, .F. ) ;
#20653 = EDGE_CURVE ( 'NONE', #17430, #12448, #6942, .T. ) ;
#20654 =( NAMED_UNIT ( * ) PLANE_ANGLE_UNIT ( ) SI_UNIT ( $, .RADIAN. ) );
#20655 = CARTESIAN_POINT ( 'NONE',  ( -39.49999999999999289, -14.67619866229204284, 94.12476896299857287 ) ) ;
#20656 = VERTEX_POINT ( 'NONE', #509 ) ;
#20657 = ADVANCED_FACE ( 'NONE', ( #3939 ), #30575, .T. ) ;
#20658 = ORIENTED_EDGE ( 'NONE', *, *, #16927, .F. ) ;
#20659 = AXIS2_PLACEMENT_3D ( 'NONE', #11024, #21987, #29761 ) ;
#20660 = AXIS2_PLACEMENT_3D ( 'NONE', #23206, #22846, #12048 ) ;
#20661 = ORIENTED_EDGE ( 'NONE', *, *, #13922, .F. ) ;
#20662 = CARTESIAN_POINT ( 'NONE',  ( -46.00000000000000000, 0.000000000000000000, 70.00000000000000000 ) ) ;
#20663 = CARTESIAN_POINT ( 'NONE',  ( -37.88768952767750875, -112.0245472910329880, 8.027725545821549957 ) ) ;
#20664 = ADVANCED_FACE ( 'NONE', ( #25897 ), #27876, .T. ) ;
#20665 = DIRECTION ( 'NONE',  ( 1.000000000000000000, 0.000000000000000000, 0.000000000000000000 ) ) ;
#20666 = EDGE_CURVE ( 'NONE', #28349, #11089, #616, .T. ) ;
#20667 = CARTESIAN_POINT ( 'NONE',  ( 1.498621416870294487, -4.753539400292362065E-14, 7.020000000000020890 ) ) ;
#20668 = ORIENTED_EDGE ( 'NONE', *, *, #13770, .T. ) ;
#20669 = ORIENTED_EDGE ( 'NONE', *, *, #5513, .F. ) ;
#20670 = CARTESIAN_POINT ( 'NONE',  ( -35.50000000000000000, -111.0141141789186605, -0.6738694770610589302 ) ) ;
#20671 = CARTESIAN_POINT ( 'NONE',  ( -55.00000000000000000, 0.000000000000000000, 70.00000000000000000 ) ) ;
#20672 = AXIS2_PLACEMENT_3D ( 'NONE', #7097, #12151, #20943 ) ;
#20673 = CARTESIAN_POINT ( 'NONE',  ( 70.00000000000001421, -36.26296008782259861, 84.27446239413865214 ) ) ;
#20674 = EDGE_LOOP ( 'NONE', ( #17927, #8489, #32373, #15982 ) ) ;
#20675 = CARTESIAN_POINT ( 'NONE',  ( -37.58145695302688694, -114.9929510916434339, 13.11211614918362756 ) ) ;
#20676 = AXIS2_PLACEMENT_3D ( 'NONE', #14192, #10801, #11148 ) ;
#20677 = CARTESIAN_POINT ( 'NONE',  ( -34.50000000000000000, -114.9929510916434339, 12.57451923796416082 ) ) ;
#20678 = PLANE ( 'NONE',  #9672 ) ;
#20679 = CARTESIAN_POINT ( 'NONE',  ( -37.51635661748575501, -114.9929510916434339, 13.11827392651459157 ) ) ;
#20680 = CARTESIAN_POINT ( 'NONE',  ( 7.999999999999992895, -44.61570720899105424, 14.73072383765550164 ) ) ;
#20681 = AXIS2_PLACEMENT_3D ( 'NONE', #22781, #15923, #7643 ) ;
#20682 = CARTESIAN_POINT ( 'NONE',  ( -37.74437085908086686, -113.9929510916434339, 14.09929883582536903 ) ) ;
#20684 = CYLINDRICAL_SURFACE ( 'NONE', #18194, 7.999999999999992895 ) ;
#20683 = CIRCLE ( 'NONE', #4048, 20.00000000000000355 ) ;
#20685 = EDGE_CURVE ( 'NONE', #2539, #16003, #8095, .T. ) ;
#20686 = CARTESIAN_POINT ( 'NONE',  ( -37.50613590685470911, -114.9929510916434339, 13.11852378322482515 ) ) ;
#20687 = ORIENTED_EDGE ( 'NONE', *, *, #5817, .F. ) ;
#20688 = CARTESIAN_POINT ( 'NONE',  ( 8.000000000000000000, 6.071532165918824830E-15, 1.000000000000000000 ) ) ;
#20689 = DIRECTION ( 'NONE',  ( 0.000000000000000000, 0.000000000000000000, 1.000000000000000000 ) ) ;
#20690 = ORIENTED_EDGE ( 'NONE', *, *, #6800, .T. ) ;
#20691 = CARTESIAN_POINT ( 'NONE',  ( -35.50000000000000711, -114.6604609523327838, 9.751889438017201428 ) ) ;
#20692 = ORIENTED_EDGE ( 'NONE', *, *, #16834, .T. ) ;
#20693 = CARTESIAN_POINT ( 'NONE',  ( 8.000000000000000000, 0.000000000000000000, 0.000000000000000000 ) ) ;
#20694 = EDGE_LOOP ( 'NONE', ( #13330, #2593, #7971, #31488, #21146, #15531 ) ) ;
#20695 = CARTESIAN_POINT ( 'NONE',  ( 8.000000000000000000, -15.92965478239607613, -15.17386234660400746 ) ) ;
#20696 = ORIENTED_EDGE ( 'NONE', *, *, #31555, .T. ) ;
#20697 = EDGE_CURVE ( 'NONE', #30657, #16063, #32833, .T. ) ;
#20698 = CARTESIAN_POINT ( 'NONE',  ( -34.50000000000000000, -113.0140978167142833, 0.8752176474019800478 ) ) ;
#20699 = FACE_OUTER_BOUND ( 'NONE', #24555, .T. ) ;
#20700 = DIRECTION ( 'NONE',  ( -1.000000000000000000, -0.000000000000000000, -0.000000000000000000 ) ) ;
#20701 = ADVANCED_FACE ( 'NONE', ( #10029 ), #10218, .T. ) ;
#20702 = EDGE_CURVE ( 'NONE', #34245, #25748, #9228, .T. ) ;
#20703 = ORIENTED_EDGE ( 'NONE', *, *, #30624, .F. ) ;
#20704 = CARTESIAN_POINT ( 'NONE',  ( -38.99999999999999289, -113.9407375970686900, 5.253524454178449155 ) ) ;
#20705 = VECTOR ( 'NONE', #23360, 1000.000000000000000 ) ;
#20706 = CARTESIAN_POINT ( 'NONE',  ( 7.999999999999992895, 7.162210897276456656, -51.50439529848821252 ) ) ;
#20707 = CARTESIAN_POINT ( 'NONE',  ( -35.50000000000000711, -112.0140978167138712, 0.5627176474015717078 ) ) ;
#20708 = ORIENTED_EDGE ( 'NONE', *, *, #32550, .F. ) ;
#20709 = ORIENTED_EDGE ( 'NONE', *, *, #5137, .T. ) ;
#20710 = CARTESIAN_POINT ( 'NONE',  ( -39.49999999999999289, 9.432411113711806294, 117.4309090467819772 ) ) ;
#20711 = AXIS2_PLACEMENT_3D ( 'NONE', #19509, #21495, #32490 ) ;
#20712 =( NAMED_UNIT ( * ) PLANE_ANGLE_UNIT ( ) SI_UNIT ( $, .RADIAN. ) );
#20713 = EDGE_CURVE ( 'NONE', #4978, #22530, #33962, .T. ) ;
#20714 = CARTESIAN_POINT ( 'NONE',  ( 0.000000000000000000, -2.710505431213761085E-17, -20.99999999999999645 ) ) ;
#20715 = ORIENTED_EDGE ( 'NONE', *, *, #2219, .T. ) ;
#20716 = ORIENTED_EDGE ( 'NONE', *, *, #15695, .T. ) ;
#20717 = CARTESIAN_POINT ( 'NONE',  ( -34.50000000000000000, -113.0557643173828524, -1.624792769101735868 ) ) ;
#20718 = CARTESIAN_POINT ( 'NONE',  ( -35.50000000000000711, -112.0140978167138712, 0.7502176474015694874 ) ) ;
#20719 = PRODUCT ( 'Heavy-Duty Locking Pawl', 'Heavy-Duty Locking Pawl', '', ( #33984 ) ) ;
#20720 = DIRECTION ( 'NONE',  ( -1.000000000000000000, -1.836970198721029934E-16, -0.000000000000000000 ) ) ;
#20721 = ORIENTED_EDGE ( 'NONE', *, *, #19569, .F. ) ;
#20722 = ORIENTED_EDGE ( 'NONE', *, *, #30839, .T. ) ;
#20723 = LINE ( 'NONE', #14800, #7439 ) ;
#20724 =( REPRESENTATION_RELATIONSHIP ('NONE','NONE', #26607, #2005 ) REPRESENTATION_RELATIONSHIP_WITH_TRANSFORMATION ( #29981 )SHAPE_REPRESENTATION_RELATIONSHIP( ) );
#20725 = CARTESIAN_POINT ( 'NONE',  ( -34.50000000000000000, -113.9929510916434623, 10.50436693183592141 ) ) ;
#20726 = AXIS2_PLACEMENT_3D ( 'NONE', #850, #17227, #20101 ) ;
#20727 = DIRECTION ( 'NONE',  ( 0.000000000000000000, 0.000000000000000000, 1.000000000000000000 ) ) ;
#20728 = CARTESIAN_POINT ( 'NONE',  ( -35.96730626674924025, -113.9929510916434339, 13.11752178341330222 ) ) ;
#20729 = ADVANCED_FACE ( 'NONE', ( #6792 ), #20994, .F. ) ;
#20730 = CARTESIAN_POINT ( 'NONE',  ( -35.51597953369717686, -115.9929510916434481, 12.74811950270164473 ) ) ;
#20731 = DIRECTION ( 'NONE',  ( -0.000000000000000000, -0.2538061376417690140, -0.9672551082808337197 ) ) ;
#20732 = LINE ( 'NONE', #18220, #15805 ) ;
#20733 = EDGE_CURVE ( 'NONE', #27996, #13354, #7504, .T. ) ;
#20734 = ORIENTED_EDGE ( 'NONE', *, *, #13664, .F. ) ;
#20735 = VECTOR ( 'NONE', #18592, 1000.000000000000000 ) ;
#20736 = CARTESIAN_POINT ( 'NONE',  ( -34.49999999999998579, -17.72201855431888973, 73.69543654875883476 ) ) ;
#20737 = DIRECTION ( 'NONE',  ( 0.000000000000000000, 0.000000000000000000, 1.000000000000000000 ) ) ;
#20738 = AXIS2_PLACEMENT_3D ( 'NONE', #7578, #19087, #8106 ) ;
#20739 = DIRECTION ( 'NONE',  ( 1.000000000000000000, -0.000000000000000000, -0.000000000000000000 ) ) ;
#20740 = STYLED_ITEM ( 'NONE', ( #30960 ), #487 ) ;
#20741 = ORIENTED_EDGE ( 'NONE', *, *, #11537, .F. ) ;
#20742 = DIRECTION ( 'NONE',  ( 0.000000000000000000, 0.9510565162951544194, -0.3090169943749449533 ) ) ;
#20743 = CARTESIAN_POINT ( 'NONE',  ( -35.50000000000000711, -112.9486715495423681, -1.623175561345890472 ) ) ;
#20744 = DIRECTION ( 'NONE',  ( 0.000000000000000000, 0.6427876096865349220, 0.7660444431189816772 ) ) ;
#20745 = EDGE_CURVE ( 'NONE', #31797, #3997, #2394, .T. ) ;
#20746 = EDGE_CURVE ( 'NONE', #21074, #4350, #26549, .T. ) ;
#20747 = DIRECTION ( 'NONE',  ( 1.000000000000000000, 0.000000000000000000, 0.000000000000000000 ) ) ;
#20748 = ORIENTED_EDGE ( 'NONE', *, *, #9739, .F. ) ;
#20749 = CARTESIAN_POINT ( 'NONE',  ( 46.00000000000000000, -25.98076211353320275, 84.99999999999992895 ) ) ;
#20750 = CARTESIAN_POINT ( 'NONE',  ( -34.50000000000000000, -117.0141134414687514, -0.5779076015960331603 ) ) ;
#20751 = DIRECTION ( 'NONE',  ( 1.000000000000000000, 0.000000000000000000, 0.000000000000000000 ) ) ;
#20752 = ORIENTED_EDGE ( 'NONE', *, *, #27920, .T. ) ;
#20753 = ORIENTED_EDGE ( 'NONE', *, *, #4206, .T. ) ;
#20754 = CARTESIAN_POINT ( 'NONE',  ( -36.52652403469556930, -113.0245472910329880, 4.222274454178449155 ) ) ;
#20755 = EDGE_LOOP ( 'NONE', ( #32339, #5037 ) ) ;
#20756 = ORIENTED_EDGE ( 'NONE', *, *, #7459, .T. ) ;
#20757 = CARTESIAN_POINT ( 'NONE',  ( -35.50000000000000000, -115.0140978167134165, -0.6247823525984399495 ) ) ;
#20758 = VECTOR ( 'NONE', #14183, 1000.000000000000000 ) ;
#20759 = STYLED_ITEM ( 'NONE', ( #24370 ), #16793 ) ;
#20760 = VECTOR ( 'NONE', #22320, 1000.000000000000000 ) ;
#20761 = CARTESIAN_POINT ( 'NONE',  ( -4.000000000000000000, 0.000000000000000000, 65.00000000000000000 ) ) ;
#20762 = CARTESIAN_POINT ( 'NONE',  ( 7.999999999999992895, -49.25004636492377585, -16.68630974939810940 ) ) ;
#20763 = CARTESIAN_POINT ( 'NONE',  ( -35.50005019975638021, -114.9929510916434339, 12.62670525340498529 ) ) ;
#20764 = CARTESIAN_POINT ( 'NONE',  ( 7.999999999999992895, 0.000000000000000000, 0.000000000000000000 ) ) ;
#20765 = EDGE_CURVE ( 'NONE', #2094, #3037, #24228, .T. ) ;
#20766 = CARTESIAN_POINT ( 'NONE',  ( -34.50000000000000000, -114.9929510916434339, 12.60752341388803544 ) ) ;
#20767 = CYLINDRICAL_SURFACE ( 'NONE', #23783, 47.49900000000001654 ) ;
#20768 = EDGE_CURVE ( 'NONE', #10384, #12895, #4824, .T. ) ;
#20769 = UNCERTAINTY_MEASURE_WITH_UNIT (LENGTH_MEASURE( 1.000000000000000082E-05 ), #15190, 'distance_accuracy_value', 'NONE');
#20770 = LINE ( 'NONE', #29618, #8836 ) ;
#20771 = ORIENTED_EDGE ( 'NONE', *, *, #5178, .T. ) ;
#20772 = CARTESIAN_POINT ( 'NONE',  ( -35.83891589277641287, -115.9929510916434481, 13.09299768411358400 ) ) ;
#20773 = CARTESIAN_POINT ( 'NONE',  ( -35.50000000000000711, -114.5974311500472425, -1.624782352598427959 ) ) ;
#20774 = DIRECTION ( 'NONE',  ( -1.000000000000000000, 0.000000000000000000, 0.000000000000000000 ) ) ;
#20775 = CARTESIAN_POINT ( 'NONE',  ( -50.00000000000000000, 19.99999999999998934, 120.0000000000000000 ) ) ;
#20776 = ORIENTED_EDGE ( 'NONE', *, *, #34662, .T. ) ;
#20777 = CARTESIAN_POINT ( 'NONE',  ( 8.000000000000000000, -14.48509162075970202, 8.733917826871310908 ) ) ;
#20778 = DIRECTION ( 'NONE',  ( 0.000000000000000000, 0.000000000000000000, 1.000000000000000000 ) ) ;
#20779 = DIRECTION ( 'NONE',  ( -1.000000000000000000, -1.734723475976807094E-16, 0.000000000000000000 ) ) ;
#20780 = DIRECTION ( 'NONE',  ( -1.000000000000000000, -0.000000000000000000, -0.000000000000000000 ) ) ;
#20781 = ORIENTED_EDGE ( 'NONE', *, *, #1630, .T. ) ;
#20782 = AXIS2_PLACEMENT_3D ( 'NONE', #34613, #1477, #29022 ) ;
#20783 = CARTESIAN_POINT ( 'NONE',  ( -37.99999999999998579, -113.9407375970686758, 3.753524454178448710 ) ) ;
#20784 = AXIS2_PLACEMENT_3D ( 'NONE', #32338, #10737, #13100 ) ;
#20785 = CARTESIAN_POINT ( 'NONE',  ( 4.000000000000003553, -12.30077720129063756, -50.52416135122095397 ) ) ;
#20786 = DIRECTION ( 'NONE',  ( 0.000000000000000000, 0.000000000000000000, -1.000000000000000000 ) ) ;
#20787 = ORIENTED_EDGE ( 'NONE', *, *, #30517, .F. ) ;
#20788 = VERTEX_POINT ( 'NONE', #29305 ) ;
#20789 = CARTESIAN_POINT ( 'NONE',  ( -42.49999999999999289, -20.32009476567218798, 72.19543654875880634 ) ) ;
#20790 = DIRECTION ( 'NONE',  ( -1.000000000000000000, 0.000000000000000000, 0.000000000000000000 ) ) ;
#20791 = ORIENTED_EDGE ( 'NONE', *, *, #3623, .F. ) ;
#20792 = CARTESIAN_POINT ( 'NONE',  ( -35.81662171581203324, -110.9754527089670546, 8.215225545821551734 ) ) ;
#20793 = ORIENTED_EDGE ( 'NONE', *, *, #15830, .F. ) ;
#20794 = CARTESIAN_POINT ( 'NONE',  ( -34.49999999999998579, -38.78532556477437510, 79.33933265213894970 ) ) ;
#20796 = EDGE_LOOP ( 'NONE', ( #15797, #6241, #18912, #6843 ) ) ;
#20795 = CIRCLE ( 'NONE', #27181, 5.016000000000010672 ) ;
#20797 = CARTESIAN_POINT ( 'NONE',  ( 8.000000000000000000, -16.59870953437682672, 3.253005020243791456 ) ) ;
#20798 = CARTESIAN_POINT ( 'NONE',  ( -50.00000000000000000, 19.99999999999998934, 110.0000000000000000 ) ) ;
#20799 = CARTESIAN_POINT ( 'NONE',  ( -42.49999999999999289, -16.18172400785637777, 71.02756813566458050 ) ) ;
#20800 = ORIENTED_EDGE ( 'NONE', *, *, #9342, .T. ) ;
#20801 = EDGE_LOOP ( 'NONE', ( #22853, #33967, #35302, #4861, #6008, #10045 ) ) ;
#20802 = CARTESIAN_POINT ( 'NONE',  ( 70.00001200000002655, -27.99523803501681130, 81.50485444658289680 ) ) ;
#20803 = CARTESIAN_POINT ( 'NONE',  ( -90.00000000000002842, 0.000000000000000000, 6.938893903907228378E-15 ) ) ;
#20804 = ORIENTED_EDGE ( 'NONE', *, *, #32433, .F. ) ;
#20805 = AXIS2_PLACEMENT_3D ( 'NONE', #20049, #9625, #34293 ) ;
#20806 = CARTESIAN_POINT ( 'NONE',  ( 8.000000000000000000, -3.384281271887680909, -18.48663108841362757 ) ) ;
#20807 = FACE_OUTER_BOUND ( 'NONE', #5794, .T. ) ;
#20808 = DIRECTION ( 'NONE',  ( 0.000000000000000000, 0.000000000000000000, -1.000000000000000000 ) ) ;
#20809 = EDGE_CURVE ( 'NONE', #27386, #10958, #13110, .T. ) ;
#20810 = CARTESIAN_POINT ( 'NONE',  ( -35.61121590948313553, -115.9929510916434481, 14.07058620477040733 ) ) ;
#20811 = CYLINDRICAL_SURFACE ( 'NONE', #22070, 7.199999999999994849 ) ;
#20812 = CARTESIAN_POINT ( 'NONE',  ( -38.97545270896704039, -113.1123104723225055, 3.847274454178449599 ) ) ;
#20813 = CARTESIAN_POINT ( 'NONE',  ( -34.50000000000000000, -115.9929510916434481, 10.85830208992344303 ) ) ;
#20814 = CYLINDRICAL_SURFACE ( 'NONE', #13627, 47.49900000000001654 ) ;
#20815 = DIRECTION ( 'NONE',  ( 0.000000000000000000, 0.000000000000000000, -1.000000000000000000 ) ) ;
#20816 = AXIS2_PLACEMENT_3D ( 'NONE', #31023, #8699, #30681 ) ;
#20817 = CARTESIAN_POINT ( 'NONE',  ( 70.00000000000001421, -24.67840078103129997, 92.38605814759151258 ) ) ;
#20818 = DIRECTION ( 'NONE',  ( 1.000000000000000000, -0.000000000000000000, -0.000000000000000000 ) ) ;
#20819 = CARTESIAN_POINT ( 'NONE',  ( -29.99999999999999645, -26.99999999999999645, 113.9999999999999858 ) ) ;
#20820 = FILL_AREA_STYLE ('',( #31824 ) ) ;
#20821 = EDGE_LOOP ( 'NONE', ( #796, #10410, #13712, #25298 ) ) ;
#20822 = EDGE_CURVE ( 'NONE', #20597, #5287, #8683, .T. ) ;
#20823 = CARTESIAN_POINT ( 'NONE',  ( -35.69809690994941320, -116.9754527089670546, 7.277725545821552622 ) ) ;
#20824 = DIRECTION ( 'NONE',  ( -1.000000000000000000, 0.000000000000000000, 0.000000000000000000 ) ) ;
#20825 = CARTESIAN_POINT ( 'NONE',  ( -35.50000000000000000, -113.0140978167136581, -0.6247823525984261828 ) ) ;
#20826 = ORIENTED_EDGE ( 'NONE', *, *, #5932, .F. ) ;
#20827 = ORIENTED_EDGE ( 'NONE', *, *, #25398, .F. ) ;
#20828 = CARTESIAN_POINT ( 'NONE',  ( 7.999999999999992895, 46.87740477351717061, 16.82754413119462455 ) ) ;
#20829 = VECTOR ( 'NONE', #20557, 1000.000000000000000 ) ;
#20830 = CARTESIAN_POINT ( 'NONE',  ( -42.49999999999997158, -25.99649394950417047, 81.00003093645244689 ) ) ;
#20831 = EDGE_LOOP ( 'NONE', ( #23741, #12685, #8809, #1446 ) ) ;
#20832 = ORIENTED_EDGE ( 'NONE', *, *, #11730, .F. ) ;
#20833 = VECTOR ( 'NONE', #7802, 1000.000000000000000 ) ;
#20834 = VERTEX_POINT ( 'NONE', #20633 ) ;
#20835 = DIRECTION ( 'NONE',  ( 0.000000000000000000, 0.4817536741017101609, 0.8763066800438663595 ) ) ;
#20836 = CARTESIAN_POINT ( 'NONE',  ( 8.000000000000007105, 0.000000000000000000, 0.000000000000000000 ) ) ;
#20837 = DIRECTION ( 'NONE',  ( 1.000000000000000000, 0.000000000000000000, 0.000000000000000000 ) ) ;
#20838 = FACE_BOUND ( 'NONE', #31243, .T. ) ;
#20839 = ORIENTED_EDGE ( 'NONE', *, *, #22912, .T. ) ;
#20840 = ORIENTED_EDGE ( 'NONE', *, *, #24868, .T. ) ;
#20841 = CIRCLE ( 'NONE', #27209, 8.000000000000007105 ) ;
#20842 = CARTESIAN_POINT ( 'NONE',  ( -35.50000000000000000, -113.6807644833805995, -2.624782352598442614 ) ) ;
#20843 = VECTOR ( 'NONE', #9805, 1000.000000000000000 ) ;
#20844 = AXIS2_PLACEMENT_3D ( 'NONE', #35135, #24319, #35309 ) ;
#20845 = CARTESIAN_POINT ( 'NONE',  ( 7.999999999999992895, 0.000000000000000000, 0.000000000000000000 ) ) ;
#20846 = CARTESIAN_POINT ( 'NONE',  ( -2.141980652367370119, -6.189445006155602336, -0.7999999999999951594 ) ) ;
#20847 = ORIENTED_EDGE ( 'NONE', *, *, #961, .T. ) ;
#20848 = PLANE ( 'NONE',  #20651 ) ;
#20849 = VECTOR ( 'NONE', #7773, 1000.000000000000000 ) ;
#20850 = EDGE_CURVE ( 'NONE', #8507, #342, #17883, .T. ) ;
#20851 = CARTESIAN_POINT ( 'NONE',  ( -34.50120407906360498, -114.9929510916434339, 12.67985367974112343 ) ) ;
#20852 = AXIS2_PLACEMENT_3D ( 'NONE', #2354, #10444, #23764 ) ;
#20853 = EDGE_CURVE ( 'NONE', #19816, #7160, #32860, .T. ) ;
#20854 = DIRECTION ( 'NONE',  ( -1.000000000000000000, 0.000000000000000000, 0.000000000000000000 ) ) ;
#20855 = CARTESIAN_POINT ( 'NONE',  ( -35.74814306589956914, -114.9929510916434339, 13.05539834812772781 ) ) ;
#20856 = DIRECTION ( 'NONE',  ( 0.000000000000000000, 1.000000000000000000, 0.000000000000000000 ) ) ;
#20857 = CARTESIAN_POINT ( 'NONE',  ( -34.50000000000000000, -114.0882517521923489, 9.510534276948430232 ) ) ;
#20858 = CARTESIAN_POINT ( 'NONE',  ( 8.000000000000000000, 0.9861715913087641949, 17.47118961583602115 ) ) ;
#20859 = CARTESIAN_POINT ( 'NONE',  ( -38.00000000000000711, -114.9929510916434339, 12.44250253426874941 ) ) ;
#20860 = CARTESIAN_POINT ( 'NONE',  ( 7.999999999999992895, -35.20873326984057883, -31.88259874184068465 ) ) ;
#20861 = ORIENTED_EDGE ( 'NONE', *, *, #8721, .F. ) ;
#20862 = FACE_OUTER_BOUND ( 'NONE', #8314, .T. ) ;
#20863 = CARTESIAN_POINT ( 'NONE',  ( 7.999999999999992895, 0.000000000000000000, 0.000000000000000000 ) ) ;
#20864 = ORIENTED_EDGE ( 'NONE', *, *, #12848, .T. ) ;
#20865 = CARTESIAN_POINT ( 'NONE',  ( -35.50000000000000711, -114.9929510916434339, 10.56126450660895699 ) ) ;
#20866 = ORIENTED_EDGE ( 'NONE', *, *, #2684, .T. ) ;
#20867 = ADVANCED_FACE ( 'NONE', ( #23534 ), #28765, .T. ) ;
#20868 = CARTESIAN_POINT ( 'NONE',  ( -37.05926240293131713, -115.9999999999999858, 1.878524454178448710 ) ) ;
#20869 = DIRECTION ( 'NONE',  ( 0.000000000000000000, -0.8443279255020201823, 0.5358267949789886631 ) ) ;
#20870 = ORIENTED_EDGE ( 'NONE', *, *, #14319, .T. ) ;
#20871 = CIRCLE ( 'NONE', #11681, 10.99999999999999645 ) ;
#20872 = CARTESIAN_POINT ( 'NONE',  ( 0.000000000000000000, -2.710505431213761085E-17, 45.89999999999999858 ) ) ;
#20873 = EDGE_LOOP ( 'NONE', ( #14433, #25967, #16628, #33845 ) ) ;
#20874 = AXIS2_PLACEMENT_3D ( 'NONE', #2082, #32306, #4953 ) ;
#20875 = CARTESIAN_POINT ( 'NONE',  ( -34.50000000000000000, -113.0140978167138712, -0.6247823525988807081 ) ) ;
#20876 = DIRECTION ( 'NONE',  ( 0.000000000000000000, -0.9510565162951500895, -0.3090169943749581649 ) ) ;
#20877 = PLANE ( 'NONE',  #14006 ) ;
#20878 = ORIENTED_EDGE ( 'NONE', *, *, #4681, .T. ) ;
#20879 = CARTESIAN_POINT ( 'NONE',  ( -33.97545270896702618, -112.8166217158120475, 4.409774454178449155 ) ) ;
#20880 = CARTESIAN_POINT ( 'NONE',  ( 0.000000000000000000, -2.710505431213761085E-17, -30.00000000000000711 ) ) ;
#20881 = CARTESIAN_POINT ( 'NONE',  ( -35.50000000000000711, -114.8474311500471572, -1.624782352598427959 ) ) ;
#20882 = AXIS2_PLACEMENT_3D ( 'NONE', #8729, #21896, #14140 ) ;
#20883 = EDGE_LOOP ( 'NONE', ( #1795, #22750, #15290, #12495 ) ) ;
#20884 = VERTEX_POINT ( 'NONE', #15059 ) ;
#20885 = CARTESIAN_POINT ( 'NONE',  ( 4.000000000000000000, 4.627536653468036720E-16, 55.00000000000000000 ) ) ;
#20886 = AXIS2_PLACEMENT_3D ( 'NONE', #23080, #4205, #31192 ) ;
#20887 = ADVANCED_FACE ( 'NONE', ( #1396 ), #12373, .T. ) ;
#20888 = CYLINDRICAL_SURFACE ( 'NONE', #2945, 20.00000000000000711 ) ;
#20889 = ORIENTED_EDGE ( 'NONE', *, *, #12556, .T. ) ;
#20890 = EDGE_LOOP ( 'NONE', ( #21875, #29242, #21640, #29372 ) ) ;
#20891 = CARTESIAN_POINT ( 'NONE',  ( -34.50000000000000000, -114.9307644833806137, -1.624782352598427959 ) ) ;
#20892 = CIRCLE ( 'NONE', #9416, 4.000000000000003553 ) ;
#20893 = LINE ( 'NONE', #35156, #7567 ) ;
#20894 = EDGE_LOOP ( 'NONE', ( #5802, #14819, #31444, #12542 ) ) ;
#20895 = VERTEX_POINT ( 'NONE', #16659 ) ;
#20896 = CARTESIAN_POINT ( 'NONE',  ( 7.999999999999992895, 0.000000000000000000, 0.000000000000000000 ) ) ;
#20897 = AXIS2_PLACEMENT_3D ( 'NONE', #10400, #27634, #2804 ) ;
#20898 = EDGE_CURVE ( 'NONE', #19399, #26771, #21353, .T. ) ;
#20899 = CARTESIAN_POINT ( 'NONE',  ( -34.50000000000000000, -113.9929510916434339, 10.50625754673586876 ) ) ;
#20900 = EDGE_CURVE ( 'NONE', #15039, #30052, #23048, .T. ) ;
#20901 = DIRECTION ( 'NONE',  ( 1.000000000000000000, -5.339440136655842133E-16, -1.047965281155519420E-16 ) ) ;
#20902 = EDGE_CURVE ( 'NONE', #1742, #33000, #21326, .T. ) ;
#20903 = CARTESIAN_POINT ( 'NONE',  ( -37.97447287825094264, -113.9929510916434339, 12.77960891308616809 ) ) ;
#20904 = CARTESIAN_POINT ( 'NONE',  ( -38.00000068757622529, -115.9929510916434481, 12.61439929482944855 ) ) ;
#20905 = DIRECTION ( 'NONE',  ( 0.000000000000000000, 1.000000000000000000, 0.000000000000000000 ) ) ;
#20907 = AXIS2_PLACEMENT_3D ( 'NONE', #28659, #31349, #12266 ) ;
#20906 = CARTESIAN_POINT ( 'NONE',  ( 8.000000000000007105, 5.679790370316226245, -7.613867765417517752 ) ) ;
#20908 = AXIS2_PLACEMENT_3D ( 'NONE', #21715, #5700, #10930 ) ;
#20909 = ORIENTED_EDGE ( 'NONE', *, *, #7274, .F. ) ;
#20910 = EDGE_CURVE ( 'NONE', #4881, #15404, #21350, .T. ) ;
#20911 = CARTESIAN_POINT ( 'NONE',  ( 0.000000000000000000, -2.710505431213761085E-17, 38.90000000000000568 ) ) ;
#20912 = FACE_OUTER_BOUND ( 'NONE', #376, .T. ) ;
#20913 = DIRECTION ( 'NONE',  ( 1.000000000000000000, 0.000000000000000000, 0.000000000000000000 ) ) ;
#20914 = EDGE_CURVE ( 'NONE', #17551, #11623, #22072, .T. ) ;
#20915 = ORIENTED_EDGE ( 'NONE', *, *, #25997, .T. ) ;
#20916 = DIRECTION ( 'NONE',  ( 0.000000000000000000, 0.000000000000000000, 1.000000000000000000 ) ) ;
#20917 = CARTESIAN_POINT ( 'NONE',  ( -35.50000000000000711, -112.0141053790792114, 0.9054673897245171243 ) ) ;
#20918 = CARTESIAN_POINT ( 'NONE',  ( -50.00000000000000000, 1.347111479062090574E-15, 59.00000000000000000 ) ) ;
#20919 = DIRECTION ( 'NONE',  ( 0.000000000000000000, 0.000000000000000000, -1.000000000000000000 ) ) ;
#20920 = CARTESIAN_POINT ( 'NONE',  ( 0.000000000000000000, 36.34385289850589373, 29.77717097092089205 ) ) ;
#20921 = CARTESIAN_POINT ( 'NONE',  ( 0.000000000000000000, -2.710505431213761085E-17, 55.00000000000000000 ) ) ;
#20922 = ORIENTED_EDGE ( 'NONE', *, *, #10573, .T. ) ;
#20923 = CARTESIAN_POINT ( 'NONE',  ( 0.000000000000000000, 0.000000000000000000, 0.000000000000000000 ) ) ;
#20924 = CARTESIAN_POINT ( 'NONE',  ( -34.50000000000000000, -112.3697613878167658, -2.522673865603075605 ) ) ;
#20925 = CARTESIAN_POINT ( 'NONE',  ( 8.000000000000000000, 0.000000000000000000, 0.000000000000000000 ) ) ;
#20926 = ORIENTED_EDGE ( 'NONE', *, *, #3104, .F. ) ;
#20927 = ORIENTED_EDGE ( 'NONE', *, *, #32301, .F. ) ;
#20928 = CARTESIAN_POINT ( 'NONE',  ( -37.05926240293131713, -113.0000000000000000, 8.121475545821549957 ) ) ;
#20929 = EDGE_CURVE ( 'NONE', #4713, #7329, #35187, .T. ) ;
#20930 = SURFACE_STYLE_USAGE ( .BOTH. , #26181 ) ;
#20931 = ORIENTED_EDGE ( 'NONE', *, *, #11910, .F. ) ;
#20932 = ORIENTED_EDGE ( 'NONE', *, *, #7540, .F. ) ;
#20933 = CARTESIAN_POINT ( 'NONE',  ( -34.50000000000000000, -113.1291422947505936, 0.8889500704178361357 ) ) ;
#20934 =( REPRESENTATION_RELATIONSHIP ('NONE','NONE', #26607, #2005 ) REPRESENTATION_RELATIONSHIP_WITH_TRANSFORMATION ( #16444 )SHAPE_REPRESENTATION_RELATIONSHIP( ) );
#20935 = AXIS2_PLACEMENT_3D ( 'NONE', #24281, #33427, #11633 ) ;
#20936 = VECTOR ( 'NONE', #28645, 1000.000000000000000 ) ;
#20937 = EDGE_CURVE ( 'NONE', #21589, #21098, #33434, .T. ) ;
#20938 = EDGE_CURVE ( 'NONE', #1909, #15703, #31178, .T. ) ;
#20939 = CARTESIAN_POINT ( 'NONE',  ( 8.000000000000000000, 5.399999999999999467, -1.000000000000003109 ) ) ;
#20940 = CIRCLE ( 'NONE', #11193, 0.7500000000000006661 ) ;
#20941 = CARTESIAN_POINT ( 'NONE',  ( 0.000000000000000000, 0.000000000000000000, 0.000000000000000000 ) ) ;
#20942 = CARTESIAN_POINT ( 'NONE',  ( -37.75185693410092824, -114.9929510916434339, 13.05539834812634581 ) ) ;
#20943 = DIRECTION ( 'NONE',  ( 0.000000000000000000, 0.000000000000000000, -1.000000000000000000 ) ) ;
#20944 = ADVANCED_FACE ( 'NONE', ( #24091 ), #10397, .T. ) ;
#20945 = ADVANCED_FACE ( 'NONE', ( #8379 ), #33063, .F. ) ;
#20946 = CARTESIAN_POINT ( 'NONE',  ( -36.50000000000011369, -114.9929510916434339, 14.11852480586264846 ) ) ;
#20947 = DIRECTION ( 'NONE',  ( -1.000000000000000000, 0.000000000000000000, 0.000000000000000000 ) ) ;
#20948 = CARTESIAN_POINT ( 'NONE',  ( -42.49999999999999289, -21.98076211353320630, 83.49999999999994316 ) ) ;
#20949 = ORIENTED_EDGE ( 'NONE', *, *, #21330, .F. ) ;
#20950 = CARTESIAN_POINT ( 'NONE',  ( -36.15625000000007816, -115.9929510916434481, 13.11852480586264846 ) ) ;
#20951 = CARTESIAN_POINT ( 'NONE',  ( 65.00000000000001421, -24.67840078103129997, 92.38605814759151258 ) ) ;
#20952 = CARTESIAN_POINT ( 'NONE',  ( 0.000000000000000000, 9.637487275701129619, 10.15474465512053470 ) ) ;
#20953 = CYLINDRICAL_SURFACE ( 'NONE', #5002, 3.799999999999999822 ) ;
#20954 = CARTESIAN_POINT ( 'NONE',  ( -34.49999999999998579, -25.98076211353322051, 84.99999999999992895 ) ) ;
#20955 = EDGE_CURVE ( 'NONE', #17521, #9833, #5890, .T. ) ;
#20956 = ORIENTED_EDGE ( 'NONE', *, *, #5319, .T. ) ;
#20957 = DIRECTION ( 'NONE',  ( 1.000000000000000000, 0.000000000000000000, 0.000000000000000000 ) ) ;
#20958 = DIRECTION ( 'NONE',  ( -1.000000000000000000, 0.000000000000000000, 0.000000000000000000 ) ) ;
#20959 = AXIS2_PLACEMENT_3D ( 'NONE', #22434, #30558, #8232 ) ;
#20960 = LINE ( 'NONE', #10535, #4456 ) ;
#20961 = FACE_OUTER_BOUND ( 'NONE', #13859, .T. ) ;
#20962 = ORIENTED_EDGE ( 'NONE', *, *, #22505, .F. ) ;
#20963 = CARTESIAN_POINT ( 'NONE',  ( -37.66520193420439000, -113.2509883718312977, 2.441024454178448710 ) ) ;
#20964 = DIRECTION ( 'NONE',  ( 1.000000000000000000, 0.000000000000000000, 0.000000000000000000 ) ) ;
#20965 = CARTESIAN_POINT ( 'NONE',  ( 0.000000000000000000, 15.46619997295644389, -1.007799283846741334 ) ) ;
#20966 = ORIENTED_EDGE ( 'NONE', *, *, #34052, .F. ) ;
#20967 = ORIENTED_EDGE ( 'NONE', *, *, #1620, .F. ) ;
#20968 = AXIS2_PLACEMENT_3D ( 'NONE', #3925, #17388, #31095 ) ;
#20969 = CARTESIAN_POINT ( 'NONE',  ( -39.49999999999999289, -13.10640646055107084, 90.70096189432331357 ) ) ;
#20970 = ORIENTED_EDGE ( 'NONE', *, *, #22491, .T. ) ;
#20971 = CARTESIAN_POINT ( 'NONE',  ( -38.99999999999999289, -114.0592624029313242, 3.246475545821551734 ) ) ;
#20972 = ORIENTED_EDGE ( 'NONE', *, *, #14271, .T. ) ;
#20973 = EDGE_CURVE ( 'NONE', #5751, #1868, #27185, .T. ) ;
#20974 = DIRECTION ( 'NONE',  ( 0.000000000000000000, 0.000000000000000000, -1.000000000000000000 ) ) ;
#20975 = CIRCLE ( 'NONE', #26161, 14.00000000000000000 ) ;
#20976 = ORIENTED_EDGE ( 'NONE', *, *, #1289, .T. ) ;
#20977 = ORIENTED_EDGE ( 'NONE', *, *, #7479, .F. ) ;
#20978 = LINE ( 'NONE', #12186, #30951 ) ;
#20979 = ADVANCED_FACE ( 'NONE', ( #27309 ), #21894, .T. ) ;
#20980 = CARTESIAN_POINT ( 'NONE',  ( 4.000000000000003553, 36.06787431788677623, 37.45808914225502662 ) ) ;
#20981 = DIRECTION ( 'NONE',  ( 0.000000000000000000, 0.000000000000000000, 1.000000000000000000 ) ) ;
#20982 = ORIENTED_EDGE ( 'NONE', *, *, #15431, .T. ) ;
#20983 = ORIENTED_EDGE ( 'NONE', *, *, #25579, .T. ) ;
#20984 = AXIS2_PLACEMENT_3D ( 'NONE', #1012, #19580, #27717 ) ;
#20985 = AXIS2_PLACEMENT_3D ( 'NONE', #28736, #3902, #4088 ) ;
#20986 = CARTESIAN_POINT ( 'NONE',  ( 0.000000000000000000, 0.000000000000000000, 0.000000000000000000 ) ) ;
#20987 = CARTESIAN_POINT ( 'NONE',  ( 9.714451465470119729E-14, 0.9999999999999870104, 53.00000000000000711 ) ) ;
#20988 = EDGE_CURVE ( 'NONE', #4405, #10551, #32887, .T. ) ;
#20989 = EDGE_LOOP ( 'NONE', ( #6299, #1020, #34803, #26818 ) ) ;
#20990 = CARTESIAN_POINT ( 'NONE',  ( 8.000000000000000000, 0.000000000000000000, 0.000000000000000000 ) ) ;
#20991 = EDGE_CURVE ( 'NONE', #33007, #19518, #8211, .T. ) ;
#20992 = VECTOR ( 'NONE', #35220, 1000.000000000000000 ) ;
#20993 = DIRECTION ( 'NONE',  ( 1.000000000000000000, 0.000000000000000000, -0.000000000000000000 ) ) ;
#20994 = CYLINDRICAL_SURFACE ( 'NONE', #1219, 4.000000000000014211 ) ;
#20995 = CARTESIAN_POINT ( 'NONE',  ( -34.50300906734826611, -115.9929510916434481, 12.71660600561482468 ) ) ;
#20996 = CARTESIAN_POINT ( 'NONE',  ( 8.000000000000000000, 0.3212489022565391261, 16.91141623315867193 ) ) ;
#20997 = CARTESIAN_POINT ( 'NONE',  ( -37.05926240293131713, -115.9999999999999858, 6.378524454178448266 ) ) ;
#20998 = CARTESIAN_POINT ( 'NONE',  ( -34.50000000000000000, -115.9929510916434481, 10.94631322572069365 ) ) ;
#20999 = DIRECTION ( 'NONE',  ( 0.000000000000000000, 0.000000000000000000, 1.000000000000000000 ) ) ;
#21000 = CARTESIAN_POINT ( 'NONE',  ( -2.000000000000000888, -5.412337245047654898E-16, -7.800000000000051337 ) ) ;
#21001 = AXIS2_PLACEMENT_3D ( 'NONE', #17994, #29364, #21237 ) ;
#21002 = CARTESIAN_POINT ( 'NONE',  ( 7.999999999999992895, 3.840921266749832252, 47.34345070675172451 ) ) ;
#21003 = PLANE ( 'NONE',  #4910 ) ;
#21004 = CARTESIAN_POINT ( 'NONE',  ( -1.799999999999996048, 0.000000000000000000, 0.000000000000000000 ) ) ;
#21005 = DIRECTION ( 'NONE',  ( -1.000000000000000000, 0.000000000000000000, 0.000000000000000000 ) ) ;
#21006 = ORIENTED_EDGE ( 'NONE', *, *, #18572, .F. ) ;
#21007 = CARTESIAN_POINT ( 'NONE',  ( -35.54388159064475872, -115.3723087153909432, 4.183975545821551734 ) ) ;
#21008 = DIRECTION ( 'NONE',  ( -1.000000000000000000, 0.000000000000000000, 0.000000000000000000 ) ) ;
#21009 = CARTESIAN_POINT ( 'NONE',  ( -35.50000000000000000, -113.0140978167138712, 0.8752176474013583229 ) ) ;
#21010 = ORIENTED_EDGE ( 'NONE', *, *, #678, .F. ) ;
#21011 = EDGE_LOOP ( 'NONE', ( #1469, #14020, #28293, #452 ) ) ;
#21013 = CARTESIAN_POINT ( 'NONE',  ( 0.000000000000000000, 32.32520163883631170, -34.09746168776000985 ) ) ;
#21012 = PRODUCT_DEFINITION_SHAPE ( 'NONE', 'NONE',  #35622 ) ;
#21014 = AXIS2_PLACEMENT_3D ( 'NONE', #10534, #32486, #7472 ) ;
#21015 = PLANE ( 'NONE',  #20935 ) ;
#21016 = EDGE_LOOP ( 'NONE', ( #4057, #19039, #32813, #3919 ) ) ;
#21017 = VERTEX_POINT ( 'NONE', #26971 ) ;
#21018 = ORIENTED_EDGE ( 'NONE', *, *, #30365, .T. ) ;
#21019 = CIRCLE ( 'NONE', #29680, 7.000000000000035527 ) ;
#21020 = EDGE_CURVE ( 'NONE', #26362, #4628, #13801, .T. ) ;
#21021 = LINE ( 'NONE', #21548, #9652 ) ;
#21022 = DIRECTION ( 'NONE',  ( 1.000000000000000000, 0.000000000000000000, 0.000000000000000000 ) ) ;
#21023 = VECTOR ( 'NONE', #29460, 1000.000000000000000 ) ;
#21024 = DIRECTION ( 'NONE',  ( -1.387778780781445922E-16, 1.000000000000000000, 0.000000000000000000 ) ) ;
#21025 = FACE_OUTER_BOUND ( 'NONE', #4634, .T. ) ;
#21027 = ORIENTED_EDGE ( 'NONE', *, *, #3429, .F. ) ;
#21026 = CIRCLE ( 'NONE', #35423, 4.000000000000000000 ) ;
#21028 = VERTEX_POINT ( 'NONE', #5522 ) ;
#21029 = CARTESIAN_POINT ( 'NONE',  ( -35.50000000000000711, -112.0140978167138712, 0.8127176474015721519 ) ) ;
#21030 = DIRECTION ( 'NONE',  ( 0.000000000000000000, 0.000000000000000000, 1.000000000000000000 ) ) ;
#21031 = DIRECTION ( 'NONE',  ( 0.000000000000000000, 0.000000000000000000, 1.000000000000000000 ) ) ;
#21032 = ORIENTED_EDGE ( 'NONE', *, *, #12599, .F. ) ;
#21033 = CARTESIAN_POINT ( 'NONE',  ( 8.000000000000000000, 6.359167119270465740, 18.96209359615096091 ) ) ;
#21034 = DIRECTION ( 'NONE',  ( -1.000000000000000000, 0.000000000000000000, 0.000000000000000000 ) ) ;
#21035 = CARTESIAN_POINT ( 'NONE',  ( -34.51922597003733273, -114.9929510916434339, 12.86289566494349224 ) ) ;
#21036 = AXIS2_PLACEMENT_3D ( 'NONE', #2770, #16402, #13376 ) ;
#21037 = CARTESIAN_POINT ( 'NONE',  ( -10.00000000000000178, 0.000000000000000000, 0.000000000000000000 ) ) ;
#21038 = CARTESIAN_POINT ( 'NONE',  ( -35.60016694755736921, -114.9929510916434339, 12.92579853460621209 ) ) ;
#21039 = LINE ( 'NONE', #2706, #28953 ) ;
#21040 = CARTESIAN_POINT ( 'NONE',  ( -39.00000000000000000, -113.9929510916434339, 12.17846912687782179 ) ) ;
#21041 = CARTESIAN_POINT ( 'NONE',  ( 7.999999999999992895, -39.78933988720095982, -24.98727647985043987 ) ) ;
#21042 = AXIS2_PLACEMENT_3D ( 'NONE', #29580, #15684, #34991 ) ;
#21043 = CIRCLE ( 'NONE', #4422, 8.000000000000001776 ) ;
#21044 = DIRECTION ( 'NONE',  ( -1.000000000000000000, 4.625929269271460867E-15, 1.174092375852883357E-15 ) ) ;
#21045 =( NAMED_UNIT ( * ) PLANE_ANGLE_UNIT ( ) SI_UNIT ( $, .RADIAN. ) );
#21046 = VERTEX_POINT ( 'NONE', #16481 ) ;
#21047 = CIRCLE ( 'NONE', #22768, 20.00000000000000355 ) ;
#21048 = CARTESIAN_POINT ( 'NONE',  ( -34.49999999999998579, -29.27980021920993536, 87.71410161513767889 ) ) ;
#21049 = CYLINDRICAL_SURFACE ( 'NONE', #12898, 3.799999999999999822 ) ;
#21050 = VERTEX_POINT ( 'NONE', #2839 ) ;
#21051 = CARTESIAN_POINT ( 'NONE',  ( -36.87500000000098055, -114.9929510916434339, 13.11852480586264669 ) ) ;
#21052 = ORIENTED_EDGE ( 'NONE', *, *, #29712, .F. ) ;
#21053 = CARTESIAN_POINT ( 'NONE',  ( -35.54388159064475872, -112.6276912846090568, 5.816024454178449155 ) ) ;
#21054 = CIRCLE ( 'NONE', #976, 14.00000000000000000 ) ;
#21055 = DIRECTION ( 'NONE',  ( -1.000000000000000000, 0.000000000000000000, 0.000000000000000000 ) ) ;
#21056 = VECTOR ( 'NONE', #8568, 1000.000000000000000 ) ;
#21057 = EDGE_LOOP ( 'NONE', ( #4186, #29230, #32393, #20611 ) ) ;
#21058 = ORIENTED_EDGE ( 'NONE', *, *, #13070, .T. ) ;
#21059 = CARTESIAN_POINT ( 'NONE',  ( -34.50000000000000000, -113.0140978167129617, -0.6247823525984270709 ) ) ;
#21060 = CARTESIAN_POINT ( 'NONE',  ( -38.99999999999999289, -113.9407375970686900, 8.253524454178448266 ) ) ;
#21061 = ORIENTED_EDGE ( 'NONE', *, *, #33878, .T. ) ;
#21062 = CARTESIAN_POINT ( 'NONE',  ( -35.62769128460905677, -115.4561184093552413, 7.691024454178449155 ) ) ;
#21063 = AXIS2_PLACEMENT_3D ( 'NONE', #32228, #7554, #26832 ) ;
#21064 = DIRECTION ( 'NONE',  ( -1.000000000000000000, 0.000000000000000000, -0.000000000000000000 ) ) ;
#21065 = EDGE_CURVE ( 'NONE', #13102, #580, #11104, .T. ) ;
#21066 = VECTOR ( 'NONE', #26309, 1000.000000000000000 ) ;
#21067 = CARTESIAN_POINT ( 'NONE',  ( -35.50000000000000711, -116.0140978167138712, 0.6252176474015648244 ) ) ;
#21068 = ORIENTED_EDGE ( 'NONE', *, *, #12632, .F. ) ;
#21069 = ORIENTED_EDGE ( 'NONE', *, *, #15490, .F. ) ;
#21070 = FACE_OUTER_BOUND ( 'NONE', #5899, .T. ) ;
#21071 = CIRCLE ( 'NONE', #29736, 11.00000000000000000 ) ;
#21072 = CARTESIAN_POINT ( 'NONE',  ( 0.1374368770859640820, -4.808326913196061980, -0.7999999999999951594 ) ) ;
#21073 = VERTEX_POINT ( 'NONE', #11270 ) ;
#21074 = VERTEX_POINT ( 'NONE', #33239 ) ;
#21075 = CARTESIAN_POINT ( 'NONE',  ( -34.50000000000000000, -113.8474311500459777, -2.624782352598442614 ) ) ;
#21076 = ADVANCED_FACE ( 'NONE', ( #31064 ), #14480, .T. ) ;
#21077 = LINE ( 'NONE', #15847, #4143 ) ;
#21078 = ORIENTED_EDGE ( 'NONE', *, *, #23996, .T. ) ;
#21079 = ORIENTED_EDGE ( 'NONE', *, *, #9978, .F. ) ;
#21080 = CARTESIAN_POINT ( 'NONE',  ( -4.000000000000000000, 0.000000000000000000, 65.00000000000000000 ) ) ;
#21081 = AXIS2_PLACEMENT_3D ( 'NONE', #21147, #24057, #34315 ) ;
#21082 = ADVANCED_FACE ( 'NONE', ( #28542 ), #11981, .T. ) ;
#21083 = CARTESIAN_POINT ( 'NONE',  ( -34.50000000000000000, -113.9813390189866027, 10.50487145766371100 ) ) ;
#21084 = LINE ( 'NONE', #34300, #2253 ) ;
#21085 = CARTESIAN_POINT ( 'NONE',  ( 7.999999999999992895, 36.05989434073613609, 30.12041790338630776 ) ) ;
#21086 = CARTESIAN_POINT ( 'NONE',  ( -38.00000000000000711, -113.9929510916434339, 12.17846912687782179 ) ) ;
#21087 = CARTESIAN_POINT ( 'NONE',  ( -36.87500000000098765, -115.9929510916434481, 13.11852480586264846 ) ) ;
#21088 = AXIS2_PLACEMENT_3D ( 'NONE', #34534, #18314, #26975 ) ;
#21089 = CARTESIAN_POINT ( 'NONE',  ( 7.999999999999992895, 47.32430374665932504, 21.55018039121545215 ) ) ;
#21090 = DIRECTION ( 'NONE',  ( 0.000000000000000000, 0.9672551082808338307, -0.2538061376417690695 ) ) ;
#21091 = CIRCLE ( 'NONE', #2734, 22.00000000000000000 ) ;
#21092 = EDGE_LOOP ( 'NONE', ( #21321, #20314, #18077, #17849 ) ) ;
#21093 = CARTESIAN_POINT ( 'NONE',  ( 50.00005079999998969, 5.400000000000098943, 1.000000000000000888 ) ) ;
#21094 = DIRECTION ( 'NONE',  ( -1.000000000000000000, 0.000000000000000000, 0.000000000000000000 ) ) ;
#21095 = DIRECTION ( 'NONE',  ( -1.000000000000000000, 0.000000000000000000, 0.000000000000000000 ) ) ;
#21096 = EDGE_CURVE ( 'NONE', #6914, #12814, #6393, .T. ) ;
#21097 = AXIS2_PLACEMENT_3D ( 'NONE', #16091, #5495, #432 ) ;
#21098 = VERTEX_POINT ( 'NONE', #24962 ) ;
#21099 = AXIS2_PLACEMENT_3D ( 'NONE', #14034, #21785, #3253 ) ;
#21100 = DIRECTION ( 'NONE',  ( -1.000000000000000000, -0.000000000000000000, -0.000000000000000000 ) ) ;
#21101 = CARTESIAN_POINT ( 'NONE',  ( -35.50000000000000711, -112.4434344552011282, 1.705278471174987986 ) ) ;
#21102 = DIRECTION ( 'NONE',  ( 0.000000000000000000, 0.000000000000000000, 1.000000000000000000 ) ) ;
#21103 = VECTOR ( 'NONE', #13247, 1000.000000000000000 ) ;
#21104 = CIRCLE ( 'NONE', #24573, 8.000000000000007105 ) ;
#21105 = VECTOR ( 'NONE', #16189, 1000.000000000000000 ) ;
#21106 = CARTESIAN_POINT ( 'NONE',  ( -35.50000000000000711, -114.3464919575557843, 9.568884482464163455 ) ) ;
#21107 = DIRECTION ( 'NONE',  ( -1.783119874454246424E-31, -1.187911941725854497E-31, 1.000000000000000000 ) ) ;
#21108 = ORIENTED_EDGE ( 'NONE', *, *, #34839, .F. ) ;
#21109 = DIRECTION ( 'NONE',  ( 1.000000000000000000, 0.000000000000000000, 0.000000000000000000 ) ) ;
#21110 = EDGE_CURVE ( 'NONE', #35305, #4771, #26044, .T. ) ;
#21111 = CARTESIAN_POINT ( 'NONE',  ( -35.50000000000000000, -112.7530559548648341, -2.608751991713152307 ) ) ;
#21112 = DIRECTION ( 'NONE',  ( -1.000000000000000000, 0.000000000000000000, 0.000000000000000000 ) ) ;
#21113 = ORIENTED_EDGE ( 'NONE', *, *, #16971, .F. ) ;
#21114 = ORIENTED_EDGE ( 'NONE', *, *, #33323, .F. ) ;
#21115 = EDGE_CURVE ( 'NONE', #21218, #9660, #2487, .T. ) ;
#21116 = CARTESIAN_POINT ( 'NONE',  ( -36.23083527818512550, -116.0245472910329880, 1.784774454178448932 ) ) ;
#21117 = ADVANCED_FACE ( 'NONE', ( #30538 ), #25491, .T. ) ;
#21118 = SURFACE_STYLE_USAGE ( .BOTH. , #27079 ) ;
#21119 = VECTOR ( 'NONE', #27462, 1000.000000000000000 ) ;
#21120 = DIRECTION ( 'NONE',  ( -1.000000000000000000, 0.000000000000000000, 0.000000000000000000 ) ) ;
#21121 = ORIENTED_EDGE ( 'NONE', *, *, #17378, .F. ) ;
#21122 = VERTEX_POINT ( 'NONE', #28192 ) ;
#21123 = CARTESIAN_POINT ( 'NONE',  ( -34.50000000000000000, -113.0140978167137717, 0.8752176474015607166 ) ) ;
#21124 = VECTOR ( 'NONE', #10567, 1000.000000000000000 ) ;
#21125 = VECTOR ( 'NONE', #33662, 1000.000000000000000 ) ;
#21126 = EDGE_CURVE ( 'NONE', #28461, #31067, #150, .T. ) ;
#21127 = CARTESIAN_POINT ( 'NONE',  ( 0.1085714285714300953, -3.798448662927791819, -0.7999999999999951594 ) ) ;
#21128 = AXIS2_PLACEMENT_3D ( 'NONE', #18867, #18151, #32205 ) ;
#21129 = EDGE_CURVE ( 'NONE', #21342, #27071, #3364, .T. ) ;
#21130 = CARTESIAN_POINT ( 'NONE',  ( 1.999999999999999112, -3.982223466972218742E-16, -4.200000000000014388 ) ) ;
#21131 = CIRCLE ( 'NONE', #23458, 0.9999999999999974465 ) ;
#21132 = CARTESIAN_POINT ( 'NONE',  ( -38.00000000000000711, -114.9929510916434339, 11.21034663311206181 ) ) ;
#21133 = DIRECTION ( 'NONE',  ( 0.000000000000000000, 0.000000000000000000, 1.000000000000000000 ) ) ;
#21134 = AXIS2_PLACEMENT_3D ( 'NONE', #2548, #29902, #30433 ) ;
#21135 = CARTESIAN_POINT ( 'NONE',  ( -34.50000000000000000, -114.5974311500472425, -1.624782352598427959 ) ) ;
#21136 = CARTESIAN_POINT ( 'NONE',  ( -37.69578139638701941, -114.9929510916434339, 14.10650203519847778 ) ) ;
#21137 = DIRECTION ( 'NONE',  ( 0.000000000000000000, 0.000000000000000000, -1.000000000000000000 ) ) ;
#21138 = FACE_OUTER_BOUND ( 'NONE', #7044, .T. ) ;
#21139 = ORIENTED_EDGE ( 'NONE', *, *, #3525, .F. ) ;
#21140 = CARTESIAN_POINT ( 'NONE',  ( -35.56312645773537895, -115.9929510916434481, 12.87038173996308998 ) ) ;
#21141 = CARTESIAN_POINT ( 'NONE',  ( -0.6000000000000037526, -12.74999999999999822, -1.200000000000006617 ) ) ;
#21142 = DIRECTION ( 'NONE',  ( 1.000000000000000000, -5.339440136655842133E-16, -1.047965281155519420E-16 ) ) ;
#21143 = PLANE ( 'NONE',  #35386 ) ;
#21144 = EDGE_CURVE ( 'NONE', #26858, #4881, #24327, .T. ) ;
#21145 = FACE_OUTER_BOUND ( 'NONE', #31318, .T. ) ;
#21146 = ORIENTED_EDGE ( 'NONE', *, *, #32177, .F. ) ;
#21147 = CARTESIAN_POINT ( 'NONE',  ( 8.000000000000000000, 8.931325931664597206, 16.53603053422209612 ) ) ;
#21148 = CARTESIAN_POINT ( 'NONE',  ( 0.000000000000000000, 0.000000000000000000, -31.10000000000000142 ) ) ;
#21149 = PRODUCT_DEFINITION ( 'UNKNOWN', '', #33917, #22715 ) ;
#21150 = PLANE ( 'NONE',  #20503 ) ;
#21151 = CARTESIAN_POINT ( 'NONE',  ( 7.999999999999992895, -11.46872990052349550, -45.56340405422456996 ) ) ;
#21152 = AXIS2_PLACEMENT_3D ( 'NONE', #23036, #3982, #1439 ) ;
#21153 = CARTESIAN_POINT ( 'NONE',  ( -36.94073759706866156, -113.0000000000000000, 5.628524454178450043 ) ) ;
#21154 = AXIS2_PLACEMENT_3D ( 'NONE', #32884, #5519, #9273 ) ;
#21155 = DIRECTION ( 'NONE',  ( 1.000000000000000000, 1.734723475976807094E-16, 0.000000000000000000 ) ) ;
#21156 = AXIS2_PLACEMENT_3D ( 'NONE', #23930, #32027, #23743 ) ;
#21157 = CARTESIAN_POINT ( 'NONE',  ( -1.600000000000004086, -12.74999999999999822, -1.200000000000006617 ) ) ;
#21158 = ORIENTED_EDGE ( 'NONE', *, *, #27088, .F. ) ;
#21159 = ORIENTED_EDGE ( 'NONE', *, *, #25362, .T. ) ;
#21160 = AXIS2_PLACEMENT_3D ( 'NONE', #537, #11517, #22489 ) ;
#21161 =( REPRESENTATION_RELATIONSHIP ('NONE','NONE', #26607, #33958 ) REPRESENTATION_RELATIONSHIP_WITH_TRANSFORMATION ( #19161 )SHAPE_REPRESENTATION_RELATIONSHIP( ) );
#21162 = DIRECTION ( 'NONE',  ( -1.000000000000000000, 0.000000000000000000, 0.000000000000000000 ) ) ;
#21163 = ADVANCED_FACE ( 'NONE', ( #25671 ), #8908, .T. ) ;
#21164 = CARTESIAN_POINT ( 'NONE',  ( 8.000000000000000000, 12.49559743815794199, -9.169462670380459812 ) ) ;
#21165 = ORIENTED_EDGE ( 'NONE', *, *, #5088, .T. ) ;
#21166 = EDGE_CURVE ( 'NONE', #34766, #30554, #3531, .T. ) ;
#21167 = CARTESIAN_POINT ( 'NONE',  ( -35.02454729103298803, -113.1123104723225197, 3.902725545821551290 ) ) ;
#21168 = ADVANCED_FACE ( 'NONE', ( #22767 ), #9098, .T. ) ;
#21169 = VERTEX_POINT ( 'NONE', #31239 ) ;
#21170 = AXIS2_PLACEMENT_3D ( 'NONE', #19940, #31304, #17427 ) ;
#21171 = VERTEX_POINT ( 'NONE', #6043 ) ;
#21172 = ORIENTED_EDGE ( 'NONE', *, *, #19909, .F. ) ;
#21173 = DIRECTION ( 'NONE',  ( 1.000000000000000000, 0.000000000000000000, 0.000000000000000000 ) ) ;
#21174 = EDGE_CURVE ( 'NONE', #1882, #15971, #17536, .T. ) ;
#21175 = CARTESIAN_POINT ( 'NONE',  ( -4.000000000000000000, 0.000000000000000000, -53.39999999999999858 ) ) ;
#21176 = ORIENTED_EDGE ( 'NONE', *, *, #1745, .T. ) ;
#21177 = ORIENTED_EDGE ( 'NONE', *, *, #2447, .T. ) ;
#21178 = DIRECTION ( 'NONE',  ( -1.000000000000000000, 0.000000000000000000, 0.000000000000000000 ) ) ;
#21179 = PLANE ( 'NONE',  #32133 ) ;
#21180 = ORIENTED_EDGE ( 'NONE', *, *, #26055, .T. ) ;
#21181 = CARTESIAN_POINT ( 'NONE',  ( -44.00000000000000000, 0.000000000000000000, 0.000000000000000000 ) ) ;
#21182 = CIRCLE ( 'NONE', #26386, 8.000000000000049738 ) ;
#21183 = CARTESIAN_POINT ( 'NONE',  ( 7.999999999999992895, -43.83938735307256707, -18.28286404005846677 ) ) ;
#21184 = DIRECTION ( 'NONE',  ( 1.000000000000000000, -5.339440136655842133E-16, -1.047965281155519420E-16 ) ) ;
#21185 = CIRCLE ( 'NONE', #26947, 20.00000000000000711 ) ;
#21186 = DIRECTION ( 'NONE',  ( -1.000000000000000000, 0.000000000000000000, 0.000000000000000000 ) ) ;
#21187 = CARTESIAN_POINT ( 'NONE',  ( -35.02454729103298092, -114.8876895276775087, 7.597274454178450043 ) ) ;
#21188 = CARTESIAN_POINT ( 'NONE',  ( -34.50000000000000000, -115.9929510916434481, 10.59426868253284226 ) ) ;
#21189 = DIRECTION ( 'NONE',  ( 1.000000000000000000, 0.000000000000000000, 0.000000000000000000 ) ) ;
#21190 = EDGE_CURVE ( 'NONE', #10377, #27557, #23723, .T. ) ;
#21191 = CARTESIAN_POINT ( 'NONE',  ( 0.000000000000000000, 0.000000000000000000, -32.00000000000000000 ) ) ;
#21192 = DIRECTION ( 'NONE',  ( 0.000000000000000000, 0.000000000000000000, 1.000000000000000000 ) ) ;
#21193 = DIRECTION ( 'NONE',  ( 1.000000000000000000, -0.000000000000000000, -0.000000000000000000 ) ) ;
#21194 = EDGE_CURVE ( 'NONE', #28247, #30561, #28919, .T. ) ;
#21195 = EDGE_CURVE ( 'NONE', #13985, #1301, #16822, .T. ) ;
#21196 = FACE_OUTER_BOUND ( 'NONE', #22281, .T. ) ;
#21197 = DIRECTION ( 'NONE',  ( -1.000000000000000000, 0.000000000000000000, 0.000000000000000000 ) ) ;
#21198 = VERTEX_POINT ( 'NONE', #12329 ) ;
#21199 = CARTESIAN_POINT ( 'NONE',  ( -37.76916472181486739, -116.0245472910329880, 4.465225545821550845 ) ) ;
#21200 = DIRECTION ( 'NONE',  ( 0.000000000000000000, 0.000000000000000000, 1.000000000000000000 ) ) ;
#21201 = DIRECTION ( 'NONE',  ( 0.000000000000000000, 0.7705132427757861446, 0.6374239897486932982 ) ) ;
#21202 = ORIENTED_EDGE ( 'NONE', *, *, #3, .F. ) ;
#21203 = ORIENTED_EDGE ( 'NONE', *, *, #3778, .F. ) ;
#21204 = DIRECTION ( 'NONE',  ( -1.000000000000000000, 0.000000000000000000, -0.000000000000000000 ) ) ;
#21205 = CARTESIAN_POINT ( 'NONE',  ( 55.00000000000000711, -27.93100416606587899, 81.50764321173589622 ) ) ;
#21206 = EDGE_LOOP ( 'NONE', ( #34982, #1771, #22344, #25079 ) ) ;
#21207 = EDGE_CURVE ( 'NONE', #35010, #2129, #1310, .T. ) ;
#21208 = ORIENTED_EDGE ( 'NONE', *, *, #63, .T. ) ;
#21209 = EDGE_CURVE ( 'NONE', #13101, #31834, #26193, .T. ) ;
#21210 = ORIENTED_EDGE ( 'NONE', *, *, #886, .T. ) ;
#21211 = AXIS2_PLACEMENT_3D ( 'NONE', #16743, #25043, #6480 ) ;
#21212 = VECTOR ( 'NONE', #1296, 1000.000000000000000 ) ;
#21213 = CARTESIAN_POINT ( 'NONE',  ( 8.000000000000000000, 0.000000000000000000, 0.000000000000000000 ) ) ;
#21214 = CARTESIAN_POINT ( 'NONE',  ( 8.000000000000007105, 7.613867765417669631, 5.679790370316101011 ) ) ;
#21215 = CARTESIAN_POINT ( 'NONE',  ( -47.99999999999999289, -25.98076211353320986, 84.99999999999992895 ) ) ;
#21216 = DIRECTION ( 'NONE',  ( -1.000000000000000000, 0.000000000000000000, 0.000000000000000000 ) ) ;
#21217 = VERTEX_POINT ( 'NONE', #23854 ) ;
#21218 = VERTEX_POINT ( 'NONE', #32130 ) ;
#21219 = CARTESIAN_POINT ( 'NONE',  ( -35.50000000000000711, -112.1403507321855528, -1.128496220798856253 ) ) ;
#21220 = DIRECTION ( 'NONE',  ( -1.000000000000000000, 5.339440136655842133E-16, -1.047965281155515476E-16 ) ) ;
#21221 = DIRECTION ( 'NONE',  ( 0.000000000000000000, 0.000000000000000000, 1.000000000000000000 ) ) ;
#21222 = ORIENTED_EDGE ( 'NONE', *, *, #8672, .T. ) ;
#21223 = DIRECTION ( 'NONE',  ( 0.000000000000000000, 0.000000000000000000, -1.000000000000000000 ) ) ;
#21224 = CARTESIAN_POINT ( 'NONE',  ( -9.999999999999994671, 0.000000000000000000, 0.000000000000000000 ) ) ;
#21225 = CARTESIAN_POINT ( 'NONE',  ( -34.50000000000000000, -114.9929510916434339, 12.44250253426871033 ) ) ;
#21226 = CARTESIAN_POINT ( 'NONE',  ( 0.000000000000000000, 15.49408907645171318, 44.90087086784599535 ) ) ;
#21227 = AXIS2_PLACEMENT_3D ( 'NONE', #24253, #5518, #27494 ) ;
#21228 = CARTESIAN_POINT ( 'NONE',  ( -37.46093750000000711, -114.9929510916434339, 13.11852480586264669 ) ) ;
#21229 = DIRECTION ( 'NONE',  ( 0.000000000000000000, -1.000000000000000000, 1.067522139062650474E-15 ) ) ;
#21230 = CARTESIAN_POINT ( 'NONE',  ( -39.00000000000000000, -113.9929510916434339, 11.21034663311206181 ) ) ;
#21231 = DIRECTION ( 'NONE',  ( 0.000000000000000000, 0.000000000000000000, -1.000000000000000000 ) ) ;
#21232 = ADVANCED_FACE ( 'NONE', ( #6748 ), #3892, .T. ) ;
#21233 = CARTESIAN_POINT ( 'NONE',  ( -37.99974912065192711, -114.9929510916434339, 12.63488142334838571 ) ) ;
#21234 = SURFACE_SIDE_STYLE ('',( #15999 ) ) ;
#21235 = ORIENTED_EDGE ( 'NONE', *, *, #19414, .F. ) ;
#21236 = AXIS2_PLACEMENT_3D ( 'NONE', #4025, #29025, #12826 ) ;
#21237 = DIRECTION ( 'NONE',  ( 0.000000000000000000, 0.000000000000000000, 1.000000000000000000 ) ) ;
#21238 = CARTESIAN_POINT ( 'NONE',  ( 7.999999999999992895, 0.000000000000000000, 0.000000000000000000 ) ) ;
#21239 = EDGE_CURVE ( 'NONE', #27661, #9040, #17975, .T. ) ;
#21240 = ORIENTED_EDGE ( 'NONE', *, *, #13487, .F. ) ;
#21241 = CARTESIAN_POINT ( 'NONE',  ( -37.50613590685470911, -114.9929510916434339, 13.11852378322482515 ) ) ;
#21242 = VERTEX_POINT ( 'NONE', #20402 ) ;
#21243 = CARTESIAN_POINT ( 'NONE',  ( -36.94073759706868287, -112.0000000000000142, 5.628524454178449155 ) ) ;
#21244 = VECTOR ( 'NONE', #1255, 1000.000000000000000 ) ;
#21245 = DIRECTION ( 'NONE',  ( 0.000000000000000000, 0.000000000000000000, 1.000000000000000000 ) ) ;
#21246 = ORIENTED_EDGE ( 'NONE', *, *, #29229, .F. ) ;
#21247 = ORIENTED_EDGE ( 'NONE', *, *, #8047, .T. ) ;
#21248 = CARTESIAN_POINT ( 'NONE',  ( -42.49999999999999289, -25.98076211353322051, 84.99999999999992895 ) ) ;
#21249 = ORIENTED_EDGE ( 'NONE', *, *, #26520, .T. ) ;
#21250 = CARTESIAN_POINT ( 'NONE',  ( -35.00000000000000000, -114.0592624029313242, 9.003524454178448266 ) ) ;
#21251 = CARTESIAN_POINT ( 'NONE',  ( 50.00005079999999680, 4.898587196589408884E-16, -3.999999999999996447 ) ) ;
#21252 = CYLINDRICAL_SURFACE ( 'NONE', #13668, 4.000000000000000000 ) ;
#21253 = ORIENTED_EDGE ( 'NONE', *, *, #34838, .F. ) ;
#21254 = ORIENTED_EDGE ( 'NONE', *, *, #7535, .F. ) ;
#21255 = CARTESIAN_POINT ( 'NONE',  ( 70.00001200000001234, -22.48561656011616350, 87.01447592148353749 ) ) ;
#21256 = FILL_AREA_STYLE ('',( #5256 ) ) ;
#21257 = CARTESIAN_POINT ( 'NONE',  ( 0.000000000000000000, 0.000000000000000000, -34.40000000000000568 ) ) ;
#21258 = ORIENTED_EDGE ( 'NONE', *, *, #30362, .F. ) ;
#21259 = ORIENTED_EDGE ( 'NONE', *, *, #5772, .F. ) ;
#21260 = AXIS2_PLACEMENT_3D ( 'NONE', #27538, #24824, #33103 ) ;
#21261 = CARTESIAN_POINT ( 'NONE',  ( -34.50000000000000000, -114.6807644833805000, -2.624782352598442614 ) ) ;
#21262 = DIRECTION ( 'NONE',  ( -1.000000000000000000, -0.000000000000000000, -0.000000000000000000 ) ) ;
#21263 = AXIS2_PLACEMENT_3D ( 'NONE', #14671, #33783, #30899 ) ;
#21264 = PRODUCT_DEFINITION_FORMATION_WITH_SPECIFIED_SOURCE ( 'ANY', '', #17848, .NOT_KNOWN. ) ;
#21265 = ORIENTED_EDGE ( 'NONE', *, *, #17134, .T. ) ;
#21266 = CARTESIAN_POINT ( 'NONE',  ( -35.50000000000000711, -114.9819937217110635, 10.35556074009299188 ) ) ;
#21267 = CARTESIAN_POINT ( 'NONE',  ( -34.50000000000000000, -113.9929510916435049, 10.50625754673586876 ) ) ;
#21268 = DIRECTION ( 'NONE',  ( 1.000000000000000000, -0.000000000000000000, -0.000000000000000000 ) ) ;
#21269 = FACE_OUTER_BOUND ( 'NONE', #35051, .T. ) ;
#21270 = CARTESIAN_POINT ( 'NONE',  ( -37.53269373325071712, -113.9929510916434339, 13.11752178341324360 ) ) ;
#21271 = CARTESIAN_POINT ( 'NONE',  ( -37.52044295795950291, -115.9929510916434481, 13.11812344617477422 ) ) ;
#21272 = DIRECTION ( 'NONE',  ( -1.000000000000000000, 0.000000000000000000, 0.000000000000000000 ) ) ;
#21273 = CARTESIAN_POINT ( 'NONE',  ( -49.99999999999998579, -60.00000000000000000, 120.0000000000000000 ) ) ;
#21274 = EDGE_CURVE ( 'NONE', #18652, #223, #4076, .T. ) ;
#21275 = ORIENTED_EDGE ( 'NONE', *, *, #16477, .T. ) ;
#21276 = AXIS2_PLACEMENT_3D ( 'NONE', #5308, #18433, #19141 ) ;
#21277 = LINE ( 'NONE', #7771, #1038 ) ;
#21278 = DIRECTION ( 'NONE',  ( 0.000000000000000000, 0.000000000000000000, -1.000000000000000000 ) ) ;
#21279 = CARTESIAN_POINT ( 'NONE',  ( -2.000000000000001776, 0.000000000000000000, 0.000000000000000000 ) ) ;
#21280 = ORIENTED_EDGE ( 'NONE', *, *, #26701, .F. ) ;
#21281 = AXIS2_PLACEMENT_3D ( 'NONE', #14892, #17060, #17412 ) ;
#21282 = LINE ( 'NONE', #34459, #20434 ) ;
#21283 = CARTESIAN_POINT ( 'NONE',  ( -35.50000000000000711, -112.3465879560236687, 1.629585756119413364 ) ) ;
#21284 = DIRECTION ( 'NONE',  ( 1.000000000000000000, -0.000000000000000000, -0.000000000000000000 ) ) ;
#21285 = EDGE_CURVE ( 'NONE', #33633, #31306, #1528, .T. ) ;
#21286 = CIRCLE ( 'NONE', #598, 7.200000000000000178 ) ;
#21287 = DIRECTION ( 'NONE',  ( -1.000000000000000000, -0.000000000000000000, 0.000000000000000000 ) ) ;
#21288 = CARTESIAN_POINT ( 'NONE',  ( 0.000000000000000000, 13.55483219355744673, -11.06713717293225407 ) ) ;
#21289 = ORIENTED_EDGE ( 'NONE', *, *, #17445, .T. ) ;
#21290 = CARTESIAN_POINT ( 'NONE',  ( -42.49999999999999289, -8.980762113533206303, 86.49999999999994316 ) ) ;
#21291 = CARTESIAN_POINT ( 'NONE',  ( -35.50000000000000000, -112.8115600290184801, 2.865251044451027074 ) ) ;
#21292 = EDGE_LOOP ( 'NONE', ( #31121, #1245, #30600, #29012 ) ) ;
#21293 = EDGE_LOOP ( 'NONE', ( #32427, #27895, #12255, #3351 ) ) ;
#21294 = CARTESIAN_POINT ( 'NONE',  ( -36.52652403469556930, -113.0245472910329880, 5.722274454178450043 ) ) ;
#21295 = SURFACE_STYLE_FILL_AREA ( #13040 ) ;
#21296 = CARTESIAN_POINT ( 'NONE',  ( 4.000000000000003553, 43.55304910509406824, 28.41006711800001128 ) ) ;
#21297 = ORIENTED_EDGE ( 'NONE', *, *, #4897, .T. ) ;
#21298 = ORIENTED_EDGE ( 'NONE', *, *, #10848, .F. ) ;
#21299 = CARTESIAN_POINT ( 'NONE',  ( -34.50000000000000000, -113.0140978167138712, 0.8752176474016720720 ) ) ;
#21300 = CIRCLE ( 'NONE', #5796, 4.200000000000014388 ) ;
#21301 = DIRECTION ( 'NONE',  ( 1.000000000000000000, -5.339440136655842133E-16, -1.047965281155519420E-16 ) ) ;
#21302 = DIRECTION ( 'NONE',  ( -1.000000000000000000, -0.000000000000000000, 0.000000000000000000 ) ) ;
#21303 = CARTESIAN_POINT ( 'NONE',  ( -38.00000000000000711, -114.9929510916434339, 12.26648026267477043 ) ) ;
#21304 = LINE ( 'NONE', #32837, #10378 ) ;
#21305 = DIRECTION ( 'NONE',  ( 0.000000000000000000, 0.5000000000000011102, -0.8660254037844380415 ) ) ;
#21306 = VECTOR ( 'NONE', #21284, 1000.000000000000000 ) ;
#21307 = AXIS2_PLACEMENT_3D ( 'NONE', #26589, #12725, #18292 ) ;
#21308 = AXIS2_PLACEMENT_3D ( 'NONE', #29737, #13352, #35499 ) ;
#21309 = CARTESIAN_POINT ( 'NONE',  ( -34.50000000000000000, -113.0974311500471714, -1.624782352598427959 ) ) ;
#21310 = AXIS2_PLACEMENT_3D ( 'NONE', #6824, #12232, #9525 ) ;
#21311 = DIRECTION ( 'NONE',  ( -1.000000000000000000, -0.000000000000000000, -0.000000000000000000 ) ) ;
#21312 = EDGE_CURVE ( 'NONE', #23442, #26801, #25854, .T. ) ;
#21313 = EDGE_CURVE ( 'NONE', #7438, #19094, #9985, .T. ) ;
#21314 = CARTESIAN_POINT ( 'NONE',  ( 8.000000000000000000, -18.48663108841356717, -3.384281271888017084 ) ) ;
#21315 = EDGE_LOOP ( 'NONE', ( #5819, #10179, #24687, #6272, #30311, #16819, #29196, #35312 ) ) ;
#21316 = CARTESIAN_POINT ( 'NONE',  ( -35.50025087934803736, -115.9929510916434481, 12.63488142334835196 ) ) ;
#21317 = CARTESIAN_POINT ( 'NONE',  ( -3.799999999999999822, 4.653657836759942730E-16, 60.00000000000000000 ) ) ;
#21318 = CARTESIAN_POINT ( 'NONE',  ( 4.000000000000000000, -6.359167119270330737, -18.96209359615098577 ) ) ;
#21319 = DIRECTION ( 'NONE',  ( 0.000000000000000000, -0.9510565162951564178, 0.3090169943749384585 ) ) ;
#21320 = CARTESIAN_POINT ( 'NONE',  ( -34.49999999999998579, -26.94801722181404102, 85.25380613764170334 ) ) ;
#21321 = ORIENTED_EDGE ( 'NONE', *, *, #478, .T. ) ;
#21322 = CARTESIAN_POINT ( 'NONE',  ( -44.00000000000000000, 0.000000000000000000, 0.000000000000000000 ) ) ;
#21323 = DIRECTION ( 'NONE',  ( -1.000000000000000000, 0.000000000000000000, 0.000000000000000000 ) ) ;
#21324 = DIRECTION ( 'NONE',  ( 1.000000000000000000, -0.000000000000000000, -0.000000000000000000 ) ) ;
#21325 = DIRECTION ( 'NONE',  ( 0.000000000000000000, 0.3420201433256629397, 0.9396926207859104263 ) ) ;
#21326 = CIRCLE ( 'NONE', #11011, 20.00000000000000355 ) ;
#21327 = ADVANCED_FACE ( 'NONE', ( #1710 ), #20767, .T. ) ;
#21328 = CARTESIAN_POINT ( 'NONE',  ( 7.999999999999992895, -44.47301969247433817, -16.68249143361957820 ) ) ;
#21329 = CARTESIAN_POINT ( 'NONE',  ( 0.000000000000000000, -2.710505431213761085E-17, -45.89999999999999858 ) ) ;
#21330 = EDGE_CURVE ( 'NONE', #18539, #28345, #22020, .T. ) ;
#21331 = VERTEX_POINT ( 'NONE', #10167 ) ;
#21332 = ORIENTED_EDGE ( 'NONE', *, *, #6432, .F. ) ;
#21333 = CARTESIAN_POINT ( 'NONE',  ( 7.999999999999992895, -3.840921266749481422, -47.34345070675177425 ) ) ;
#21334 = DIRECTION ( 'NONE',  ( 0.000000000000000000, 0.000000000000000000, 1.000000000000000000 ) ) ;
#21335 = CYLINDRICAL_SURFACE ( 'NONE', #11187, 22.00000000000000000 ) ;
#21336 = VERTEX_POINT ( 'NONE', #20595 ) ;
#21337 = CARTESIAN_POINT ( 'NONE',  ( -38.97545270896704039, -114.8876895276775087, 4.652725545821551734 ) ) ;
#21338 = VERTEX_POINT ( 'NONE', #29074 ) ;
#21339 = AXIS2_PLACEMENT_3D ( 'NONE', #6262, #27875, #22456 ) ;
#21340 = COLOUR_RGB ( '', 0.31764706, 0.68627451, 0.89019608) ;
#21341 = ORIENTED_EDGE ( 'NONE', *, *, #26222, .F. ) ;
#21342 = VERTEX_POINT ( 'NONE', #31767 ) ;
#21343 = DIRECTION ( 'NONE',  ( 0.000000000000000000, 0.8090169943749448977, 0.5877852522924766898 ) ) ;
#21344 = EDGE_CURVE ( 'NONE', #2400, #26214, #12696, .T. ) ;
#21345 = CYLINDRICAL_SURFACE ( 'NONE', #4172, 20.00000000000000711 ) ;
#21346 = ORIENTED_EDGE ( 'NONE', *, *, #25198, .F. ) ;
#21347 = ORIENTED_EDGE ( 'NONE', *, *, #29513, .T. ) ;
#21348 = CARTESIAN_POINT ( 'NONE',  ( 4.000000000000003553, 10.15474465512070168, -9.637487275700989287 ) ) ;
#21349 = DIRECTION ( 'NONE',  ( 1.000000000000000000, -5.339440136655842133E-16, -1.047965281155519420E-16 ) ) ;
#21350 = CIRCLE ( 'NONE', #27698, 22.00000000000000000 ) ;
#21351 = DIRECTION ( 'NONE',  ( 1.000000000000000000, -5.339440136655842133E-16, -1.047965281155519420E-16 ) ) ;
#21352 = LINE ( 'NONE', #34527, #31495 ) ;
#21353 = LINE ( 'NONE', #24613, #29988 ) ;
#21354 = EDGE_CURVE ( 'NONE', #19035, #30069, #32952, .T. ) ;
#21355 = EDGE_CURVE ( 'NONE', #5886, #14609, #16274, .T. ) ;
#21356 = CYLINDRICAL_SURFACE ( 'NONE', #17485, 0.7500000000000039968 ) ;
#21357 = CARTESIAN_POINT ( 'NONE',  ( -35.62769128460905677, -115.4561184093552413, 4.691024454178448266 ) ) ;
#21358 = ADVANCED_FACE ( 'NONE', ( #1182 ), #17723, .T. ) ;
#21359 = AXIS2_PLACEMENT_3D ( 'NONE', #11176, #22147, #19452 ) ;
#21360 =( GEOMETRIC_REPRESENTATION_CONTEXT ( 3 ) GLOBAL_UNCERTAINTY_ASSIGNED_CONTEXT ( ( #10767 ) ) GLOBAL_UNIT_ASSIGNED_CONTEXT ( ( #34242, #2019, #35150 ) ) REPRESENTATION_CONTEXT ( 'NONE', 'WORKASPACE' ) );
#21361 = CARTESIAN_POINT ( 'NONE',  ( -34.51922597003733273, -115.9929510916434481, 12.86289566494349224 ) ) ;
#21363 = LINE ( 'NONE', #12567, #12472 ) ;
#21362 = AXIS2_PLACEMENT_3D ( 'NONE', #24083, #29116, #10389 ) ;
#21364 = DIRECTION ( 'NONE',  ( -1.000000000000000000, 0.000000000000000000, 0.000000000000000000 ) ) ;
#21365 = LINE ( 'NONE', #7156, #11308 ) ;
#21366 = DIRECTION ( 'NONE',  ( 0.000000000000000000, -0.8660254037844327124, -0.5000000000000101030 ) ) ;
#21367 = DIRECTION ( 'NONE',  ( 1.000000000000000000, 0.000000000000000000, -0.000000000000000000 ) ) ;
#21368 = FACE_OUTER_BOUND ( 'NONE', #14545, .T. ) ;
#21369 = ORIENTED_EDGE ( 'NONE', *, *, #13960, .F. ) ;
#21370 = EDGE_CURVE ( 'NONE', #8637, #31804, #29522, .T. ) ;
#21371 = CARTESIAN_POINT ( 'NONE',  ( -38.18337828418796676, -117.0245472910329738, 8.965225545821551734 ) ) ;
#21372 = DIRECTION ( 'NONE',  ( -1.000000000000000000, -1.734723475976807094E-16, -0.000000000000000000 ) ) ;
#21373 = CARTESIAN_POINT ( 'NONE',  ( 0.000000000000000000, -9.919332006307262972, 5.363026430117087351 ) ) ;
#21374 = EDGE_CURVE ( 'NONE', #9277, #22897, #12262, .T. ) ;
#21375 = EDGE_LOOP ( 'NONE', ( #34611, #26263, #12535, #25709, #13863, #30305, #6027, #11509, #8279, #16132, #10338, #27600, #24085, #27602, #11028, #28568, #11313, #14406, #33990, #28044, #25752, #34682, #28402, #22535, #12490, #29722, #29957, #5770, #1784, #28395, #25387, #6725, #22342, #30702, #32957, #6586, #11246, #22753, #23290, #30628, #20626, #28996, #18995, #25559, #4809, #32084, #4217, #28123, #19798, #30088, #27532, #35061, #33500 ) ) ;
#21376 = MECHANICAL_DESIGN_GEOMETRIC_PRESENTATION_REPRESENTATION (  '', ( #4155 ), #34631 ) ;
#21377 = ORIENTED_EDGE ( 'NONE', *, *, #21808, .T. ) ;
#21378 = DIRECTION ( 'NONE',  ( -1.000000000000000000, 0.000000000000000000, 0.000000000000000000 ) ) ;
#21379 = DIRECTION ( 'NONE',  ( -1.000000000000000000, -0.000000000000000000, -0.000000000000000000 ) ) ;
#21380 = ORIENTED_EDGE ( 'NONE', *, *, #24916, .F. ) ;
#21381 = ORIENTED_EDGE ( 'NONE', *, *, #4066, .F. ) ;
#21382 = DIRECTION ( 'NONE',  ( -1.174092375852890260E-15, 4.222049128630259891E-16, 1.000000000000000000 ) ) ;
#21383 = CARTESIAN_POINT ( 'NONE',  ( -37.76916472181486739, -116.0245472910329880, 8.965225545821551734 ) ) ;
#21384 = CIRCLE ( 'NONE', #34648, 20.00000000000000711 ) ;
#21385 = CIRCLE ( 'NONE', #20216, 7.199999999999994849 ) ;
#21386 = DIRECTION ( 'NONE',  ( 1.000000000000000000, 0.000000000000000000, 0.000000000000000000 ) ) ;
#21387 = EDGE_CURVE ( 'NONE', #6691, #1965, #23126, .T. ) ;
#21388 = CARTESIAN_POINT ( 'NONE',  ( 0.000000000000000000, 6.359167119270465740, 18.96209359615096446 ) ) ;
#21389 = ORIENTED_EDGE ( 'NONE', *, *, #6811, .T. ) ;
#21390 = ORIENTED_EDGE ( 'NONE', *, *, #10525, .T. ) ;
#21391 = CARTESIAN_POINT ( 'NONE',  ( -35.50000000000000711, -113.3557509229967764, 1.923098431109107054 ) ) ;
#21392 = ADVANCED_FACE ( 'NONE', ( #18797 ), #24569, .T. ) ;
#21393 = DIRECTION ( 'NONE',  ( 0.000000000000000000, 0.000000000000000000, 1.000000000000000000 ) ) ;
#21394 = FACE_OUTER_BOUND ( 'NONE', #8893, .T. ) ;
#21395 = EDGE_CURVE ( 'NONE', #34729, #15733, #5936, .T. ) ;
#21396 = ORIENTED_EDGE ( 'NONE', *, *, #20032, .T. ) ;
#21397 = CARTESIAN_POINT ( 'NONE',  ( 4.872650870659739120, 0.4273491293402878477, -0.7999999999999893863 ) ) ;
#21398 = CARTESIAN_POINT ( 'NONE',  ( -34.50000000000000000, -112.0140900043112282, 0.8439677466545482121 ) ) ;
#21399 = CARTESIAN_POINT ( 'NONE',  ( -34.50000000000000000, -114.9922651054798308, 10.46846006712531008 ) ) ;
#21400 = CYLINDRICAL_SURFACE ( 'NONE', #2791, 11.00000000000001066 ) ;
#21401 = ADVANCED_FACE ( 'NONE', ( #72 ), #35032, .T. ) ;
#21402 = CARTESIAN_POINT ( 'NONE',  ( -37.99994980024369085, -114.9929510916434339, 12.62670525340494621 ) ) ;
#21403 = DIRECTION ( 'NONE',  ( -1.000000000000000000, 0.000000000000000000, 0.000000000000000000 ) ) ;
#21404 = EDGE_CURVE ( 'NONE', #14060, #32241, #19703, .T. ) ;
#21405 = CARTESIAN_POINT ( 'NONE',  ( -34.50000000000000000, -114.9929510916434339, 10.51725893871048889 ) ) ;
#21406 = CARTESIAN_POINT ( 'NONE',  ( -4.000000000000000000, 0.000000000000000000, 65.00000000000000000 ) ) ;
#21407 = DIRECTION ( 'NONE',  ( -1.000000000000000000, 0.000000000000000000, 0.000000000000000000 ) ) ;
#21408 = DIRECTION ( 'NONE',  ( -1.000000000000000000, 0.000000000000000000, -0.000000000000000000 ) ) ;
#21409 = VERTEX_POINT ( 'NONE', #29437 ) ;
#21410 = CARTESIAN_POINT ( 'NONE',  ( 55.00000000000000711, -25.98076211353320986, 84.99999999999994316 ) ) ;
#21411 = CYLINDRICAL_SURFACE ( 'NONE', #30166, 9.499000000000000554 ) ;
#21412 = ORIENTED_EDGE ( 'NONE', *, *, #16558, .T. ) ;
#21413 = VECTOR ( 'NONE', #35335, 1000.000000000000000 ) ;
#21414 = CARTESIAN_POINT ( 'NONE',  ( -38.00000000000000711, -114.9929510916434339, 12.59102132592608925 ) ) ;
#21415 = ORIENTED_EDGE ( 'NONE', *, *, #29026, .F. ) ;
#21416 = VECTOR ( 'NONE', #26559, 1000.000000000000000 ) ;
#21417 = CARTESIAN_POINT ( 'NONE',  ( -36.23083527818512550, -116.0245472910329880, 6.284774454178450043 ) ) ;
#21418 = FACE_OUTER_BOUND ( 'NONE', #32308, .T. ) ;
#21419 = ORIENTED_EDGE ( 'NONE', *, *, #2777, .F. ) ;
#21420 = ORIENTED_EDGE ( 'NONE', *, *, #18568, .T. ) ;
#21421 = CARTESIAN_POINT ( 'NONE',  ( 5.400000000000085620, -1.000000000000049516, -44.50000000000000000 ) ) ;
#21422 = ORIENTED_EDGE ( 'NONE', *, *, #31008, .F. ) ;
#21423 = CARTESIAN_POINT ( 'NONE',  ( -38.45611840935523418, -115.3723087153909432, 8.066024454178448266 ) ) ;
#21424 = AXIS2_PLACEMENT_3D ( 'NONE', #24176, #32449, #16042 ) ;
#21425 = DIRECTION ( 'NONE',  ( 0.1305261922200477154, 0.9914448613738109373, 2.653430841701508438E-16 ) ) ;
#21426 = CARTESIAN_POINT ( 'NONE',  ( 0.9999999999999453770, -6.008326913195871199, -0.7999999999999951594 ) ) ;
#21427 = ORIENTED_EDGE ( 'NONE', *, *, #29991, .F. ) ;
#21428 = VERTEX_POINT ( 'NONE', #24212 ) ;
#21429 = CARTESIAN_POINT ( 'NONE',  ( 0.000000000000000000, -44.75336757549789013, 14.30704879393590545 ) ) ;
#21430 = EDGE_CURVE ( 'NONE', #6464, #27557, #8799, .T. ) ;
#21431 = FACE_BOUND ( 'NONE', #23472, .T. ) ;
#21432 = VERTEX_POINT ( 'NONE', #35201 ) ;
#21433 = ORIENTED_EDGE ( 'NONE', *, *, #33432, .F. ) ;
#21434 = CARTESIAN_POINT ( 'NONE',  ( -34.50000000000000000, -112.3070160848889429, 2.749963775944984867 ) ) ;
#21435 = EDGE_CURVE ( 'NONE', #33466, #17702, #9974, .T. ) ;
#21436 = CIRCLE ( 'NONE', #22001, 9.999999999999994671 ) ;
#21437 = AXIS2_PLACEMENT_3D ( 'NONE', #14568, #25938, #34035 ) ;
#21438 = DIRECTION ( 'NONE',  ( -1.000000000000000000, 0.000000000000000000, 0.000000000000000000 ) ) ;
#21439 = ORIENTED_EDGE ( 'NONE', *, *, #24718, .F. ) ;
#21440 = CARTESIAN_POINT ( 'NONE',  ( -35.50000000000000711, -114.9492820284331742, 10.20776876943783940 ) ) ;
#21441 = CARTESIAN_POINT ( 'NONE',  ( -34.50000000000000000, -113.9929510916436470, 10.50625754673586876 ) ) ;
#21442 = CARTESIAN_POINT ( 'NONE',  ( 3.799999999999999822, 0.000000000000000000, -55.00000000000000000 ) ) ;
#21443 = CARTESIAN_POINT ( 'NONE',  ( 0.000000000000000000, -32.00046193115124282, -34.40241257139719977 ) ) ;
#21444 = CARTESIAN_POINT ( 'NONE',  ( -37.99599240977853754, -113.9929510916434339, 12.68378527132499656 ) ) ;
#21445 = CARTESIAN_POINT ( 'NONE',  ( -36.00585935943765747, -115.9929510916434481, 13.11852578240983291 ) ) ;
#21446 = CARTESIAN_POINT ( 'NONE',  ( 1.519999999999993578, 5.015999999999978698, 1.387778780781445676E-14 ) ) ;
#21447 = VECTOR ( 'NONE', #8763, 1000.000000000000000 ) ;
#21448 = DIRECTION ( 'NONE',  ( -1.000000000000000000, 0.000000000000000000, 0.000000000000000000 ) ) ;
#21449 = VECTOR ( 'NONE', #11987, 1000.000000000000000 ) ;
#21450 = EDGE_LOOP ( 'NONE', ( #33134, #30049, #24405, #10126 ) ) ;
#21451 = FACE_OUTER_BOUND ( 'NONE', #35457, .T. ) ;
#21452 = CARTESIAN_POINT ( 'NONE',  ( 4.000000000000000000, 4.898587196589412829E-16, 65.00000000000000000 ) ) ;
#21453 = DIRECTION ( 'NONE',  ( 1.282131172192753642E-16, -6.938893903907203726E-17, -1.000000000000000000 ) ) ;
#21454 = EDGE_LOOP ( 'NONE', ( #23607, #4772, #26060, #1456 ) ) ;
#21455 = DIRECTION ( 'NONE',  ( -1.000000000000000000, -0.000000000000000000, -0.000000000000000000 ) ) ;
#21456 = VECTOR ( 'NONE', #4216, 1000.000000000000000 ) ;
#21457 = VECTOR ( 'NONE', #1810, 1000.000000000000000 ) ;
#21458 = CARTESIAN_POINT ( 'NONE',  ( -35.50000000000000000, -113.0140978167139991, 0.8752176474014555785 ) ) ;
#21459 = DIRECTION ( 'NONE',  ( 0.000000000000000000, 0.000000000000000000, -1.000000000000000000 ) ) ;
#21460 = CIRCLE ( 'NONE', #32401, 52.00000000000000711 ) ;
#21461 = CARTESIAN_POINT ( 'NONE',  ( -35.50000000000000711, -114.9929510916434339, 12.56351784598954424 ) ) ;
#21462 = DIRECTION ( 'NONE',  ( 0.000000000000000000, 0.000000000000000000, 1.000000000000000000 ) ) ;
#21463 = EDGE_LOOP ( 'NONE', ( #25990, #28789, #28463, #33102 ) ) ;
#21464 = CARTESIAN_POINT ( 'NONE',  ( 0.000000000000000000, 0.000000000000000000, -40.00000000000000711 ) ) ;
#21465 = CARTESIAN_POINT ( 'NONE',  ( -35.50000000000000000, -112.1946304249441795, 2.703640693953100804 ) ) ;
#21466 = VERTEX_POINT ( 'NONE', #2803 ) ;
#21467 = ORIENTED_EDGE ( 'NONE', *, *, #20809, .T. ) ;
#21468 = CARTESIAN_POINT ( 'NONE',  ( -37.35495115944176092, -112.9754527089670688, 8.534774454178448266 ) ) ;
#21469 = LINE ( 'NONE', #15713, #23292 ) ;
#21470 = ORIENTED_EDGE ( 'NONE', *, *, #24985, .T. ) ;
#21471 = ORIENTED_EDGE ( 'NONE', *, *, #836, .T. ) ;
#21472 = CARTESIAN_POINT ( 'NONE',  ( -34.50000000000000000, -113.0140978167138712, -0.4997823525984338988 ) ) ;
#21473 = EDGE_CURVE ( 'NONE', #29218, #33428, #18975, .T. ) ;
#21474 = CARTESIAN_POINT ( 'NONE',  ( 0.000000000000000000, -2.710505431213761085E-17, 54.99999999999999289 ) ) ;
#21475 = CARTESIAN_POINT ( 'NONE',  ( 55.00000000000000711, -25.98076211353320986, 84.99999999999994316 ) ) ;
#21476 = CIRCLE ( 'NONE', #25510, 52.00000000000000711 ) ;
#21477 = CARTESIAN_POINT ( 'NONE',  ( -38.00000000000000711, -114.9929510916434339, 12.53051367006571937 ) ) ;
#21478 = VECTOR ( 'NONE', #4784, 1000.000000000000000 ) ;
#21479 = CARTESIAN_POINT ( 'NONE',  ( 0.000000000000000000, 0.000000000000000000, 65.00000000000000000 ) ) ;
#21480 = DIRECTION ( 'NONE',  ( 0.000000000000000000, 0.000000000000000000, 1.000000000000000000 ) ) ;
#21481 = ADVANCED_FACE ( 'NONE', ( #13235 ), #10350, .T. ) ;
#21482 = CARTESIAN_POINT ( 'NONE',  ( -34.50000000000000000, -114.8474311500471572, -1.624782352598427959 ) ) ;
#21483 = DIRECTION ( 'NONE',  ( 0.000000000000000000, 0.000000000000000000, -1.000000000000000000 ) ) ;
#21484 = AXIS2_PLACEMENT_3D ( 'NONE', #5382, #27696, #35445 ) ;
#21485 = DIRECTION ( 'NONE',  ( 1.000000000000000000, -0.000000000000000000, 0.000000000000000000 ) ) ;
#21486 = ORIENTED_EDGE ( 'NONE', *, *, #31089, .T. ) ;
#21487 = CARTESIAN_POINT ( 'NONE',  ( -37.99974912065192001, -115.9929510916434481, 12.63488142334838749 ) ) ;
#21488 = DIRECTION ( 'NONE',  ( -1.000000000000000000, -0.000000000000000000, 0.000000000000000000 ) ) ;
#21489 = CARTESIAN_POINT ( 'NONE',  ( 8.000000000000000000, 13.60411018104336023, -12.96676809804134400 ) ) ;
#21490 = PLANE ( 'NONE',  #19391 ) ;
#21491 = ORIENTED_EDGE ( 'NONE', *, *, #27880, .T. ) ;
#21492 = DIRECTION ( 'NONE',  ( 0.000000000000000000, -1.000000000000000000, 0.000000000000000000 ) ) ;
#21493 = CARTESIAN_POINT ( 'NONE',  ( 29.99999999999999289, 1.244980450007031636E-14, 3.000000000000002665 ) ) ;
#21494 = LINE ( 'NONE', #17913, #6155 ) ;
#21495 = DIRECTION ( 'NONE',  ( 0.000000000000000000, 0.9929510916431029122, -0.1185248058626136303 ) ) ;
#21496 = CARTESIAN_POINT ( 'NONE',  ( 0.000000000000000000, -46.11014828289849277, 9.022736828080537563 ) ) ;
#21497 = CARTESIAN_POINT ( 'NONE',  ( -34.50000000000000000, -114.0000000000000853, 2.000000000000001776 ) ) ;
#21498 = ORIENTED_EDGE ( 'NONE', *, *, #22194, .F. ) ;
#21499 = EDGE_LOOP ( 'NONE', ( #32230, #33483 ) ) ;
#21500 = CIRCLE ( 'NONE', #26126, 20.00000000000000711 ) ;
#21501 = CYLINDRICAL_SURFACE ( 'NONE', #2689, 19.99999999999998579 ) ;
#21502 = DIRECTION ( 'NONE',  ( -1.000000000000000000, 0.000000000000000000, 0.000000000000000000 ) ) ;
#21503 = DIRECTION ( 'NONE',  ( -1.000000000000000000, 0.000000000000000000, 0.000000000000000000 ) ) ;
#21504 = ORIENTED_EDGE ( 'NONE', *, *, #10155, .F. ) ;
#21505 = CARTESIAN_POINT ( 'NONE',  ( -38.37230871539094323, -115.4561184093552413, 9.058975545821551734 ) ) ;
#21506 = ORIENTED_EDGE ( 'NONE', *, *, #22416, .T. ) ;
#21507 =( LENGTH_UNIT ( ) NAMED_UNIT ( * ) SI_UNIT ( .MILLI., .METRE. ) );
#21508 = ORIENTED_EDGE ( 'NONE', *, *, #7503, .F. ) ;
#21509 = VERTEX_POINT ( 'NONE', #13761 ) ;
#21510 = CYLINDRICAL_SURFACE ( 'NONE', #1666, 4.000000000000000000 ) ;
#21511 = EDGE_CURVE ( 'NONE', #14882, #20125, #15144, .T. ) ;
#21512 = EDGE_CURVE ( 'NONE', #16196, #741, #18609, .T. ) ;
#21513 = CARTESIAN_POINT ( 'NONE',  ( 0.000000000000000000, -5.482169781018935595, 16.00140663693123599 ) ) ;
#21514 = ORIENTED_EDGE ( 'NONE', *, *, #17614, .T. ) ;
#21515 = ORIENTED_EDGE ( 'NONE', *, *, #13937, .T. ) ;
#21516 = DIRECTION ( 'NONE',  ( 0.000000000000000000, 0.000000000000000000, 1.000000000000000000 ) ) ;
#21517 = FACE_OUTER_BOUND ( 'NONE', #19611, .T. ) ;
#21518 = EDGE_CURVE ( 'NONE', #10719, #21916, #24939, .T. ) ;
#21519 = DIRECTION ( 'NONE',  ( -1.000000000000000000, 0.000000000000000000, 0.000000000000000000 ) ) ;
#21520 = CARTESIAN_POINT ( 'NONE',  ( -10.00000000000000178, 0.000000000000000000, 0.000000000000000000 ) ) ;
#21521 = CARTESIAN_POINT ( 'NONE',  ( 8.000000000000000000, 0.000000000000000000, 0.000000000000000000 ) ) ;
#21522 = CIRCLE ( 'NONE', #25589, 6.000000000000005329 ) ;
#21523 = CARTESIAN_POINT ( 'NONE',  ( -39.02454729103295961, -114.7691647218148745, 3.659774454178448710 ) ) ;
#21524 = CARTESIAN_POINT ( 'NONE',  ( -37.52454134262689678, -115.9929510916434481, 14.11837420659362152 ) ) ;
#21525 = CARTESIAN_POINT ( 'NONE',  ( 0.000000000000000000, 0.000000000000000000, -40.89999999999999858 ) ) ;
#21526 = AXIS2_PLACEMENT_3D ( 'NONE', #1414, #25552, #1239 ) ;
#21527 = FACE_OUTER_BOUND ( 'NONE', #12772, .T. ) ;
#21528 = DIRECTION ( 'NONE',  ( -1.783119874454246424E-31, -1.187911941725854497E-31, 1.000000000000000000 ) ) ;
#21529 = DIRECTION ( 'NONE',  ( 0.000000000000000000, 0.000000000000000000, 1.000000000000000000 ) ) ;
#21530 = DIRECTION ( 'NONE',  ( -1.000000000000000000, -0.000000000000000000, 0.000000000000000000 ) ) ;
#21531 = LINE ( 'NONE', #30027, #33916 ) ;
#21532 = VERTEX_POINT ( 'NONE', #13403 ) ;
#21533 = CARTESIAN_POINT ( 'NONE',  ( -34.92058450342249643, -111.8367748094582197, 8.308975545821549957 ) ) ;
#21534 = CARTESIAN_POINT ( 'NONE',  ( 0.000000000000000000, -2.494040418455483188, 18.62763138773849292 ) ) ;
#21535 = CYLINDRICAL_SURFACE ( 'NONE', #34905, 5.000000000000011546 ) ;
#21536 = ADVANCED_FACE ( 'NONE', ( #29800 ), #4781, .T. ) ;
#21537 = DIRECTION ( 'NONE',  ( 0.000000000000000000, 0.000000000000000000, 1.000000000000000000 ) ) ;
#21538 = ORIENTED_EDGE ( 'NONE', *, *, #23938, .F. ) ;
#21539 = CIRCLE ( 'NONE', #859, 17.49900000000001654 ) ;
#21540 = ORIENTED_EDGE ( 'NONE', *, *, #26015, .T. ) ;
#21541 = PRODUCT_DEFINITION_CONTEXT ( 'detailed design', #18376, 'design' ) ;
#21542 = DIRECTION ( 'NONE',  ( -1.174092375852890260E-15, 4.222049128630259891E-16, 1.000000000000000000 ) ) ;
#21543 = CARTESIAN_POINT ( 'NONE',  ( -34.49999999999998579, -13.92619866229204106, 93.69175626110634880 ) ) ;
#21544 = EDGE_LOOP ( 'NONE', ( #4360, #22967, #8394, #17239 ) ) ;
#21545 = ORIENTED_EDGE ( 'NONE', *, *, #9065, .F. ) ;
#21546 = CIRCLE ( 'NONE', #26172, 8.000000000000014211 ) ;
#21547 = EDGE_CURVE ( 'NONE', #33707, #13869, #3100, .T. ) ;
#21548 = CARTESIAN_POINT ( 'NONE',  ( 7.999999999999992895, 26.17370628620655637, 39.63700417846175128 ) ) ;
#21549 = CIRCLE ( 'NONE', #23280, 3.799999999999999822 ) ;
#21550 = EDGE_CURVE ( 'NONE', #16904, #24590, #23809, .T. ) ;
#21551 = CARTESIAN_POINT ( 'NONE',  ( -38.99999999999999289, -114.0592624029313242, 9.246475545821551734 ) ) ;
#21552 = EDGE_CURVE ( 'NONE', #35587, #31214, #14576, .T. ) ;
#21553 = CARTESIAN_POINT ( 'NONE',  ( -21.09999999999999432, -25.98076211353322051, 84.99999999999995737 ) ) ;
#21554 = VECTOR ( 'NONE', #3194, 1000.000000000000000 ) ;
#21555 = CARTESIAN_POINT ( 'NONE',  ( 115.0000000000000000, 81.48267994499606459, 30.15054357219658954 ) ) ;
#21556 = ORIENTED_EDGE ( 'NONE', *, *, #17234, .F. ) ;
#21557 = ORIENTED_EDGE ( 'NONE', *, *, #21889, .T. ) ;
#21558 = CARTESIAN_POINT ( 'NONE',  ( -35.50000000000000711, -112.7549084230351752, -1.592823285203595285 ) ) ;
#21559 = VECTOR ( 'NONE', #35189, 1000.000000000000000 ) ;
#21560 = DIRECTION ( 'NONE',  ( -1.000000000000000000, 0.000000000000000000, 0.000000000000000000 ) ) ;
#21561 = EDGE_CURVE ( 'NONE', #30249, #6633, #34733, .T. ) ;
#21562 = FACE_OUTER_BOUND ( 'NONE', #1963, .T. ) ;
#21563 = ORIENTED_EDGE ( 'NONE', *, *, #5523, .T. ) ;
#21564 = FACE_OUTER_BOUND ( 'NONE', #32289, .T. ) ;
#21565 = EDGE_CURVE ( 'NONE', #32655, #27460, #30796, .T. ) ;
#21566 = CIRCLE ( 'NONE', #19282, 8.000000000000001776 ) ;
#21567 = CARTESIAN_POINT ( 'NONE',  ( -34.50000000000000000, -116.0140896356112989, -0.6575071456984549201 ) ) ;
#21568 = CARTESIAN_POINT ( 'NONE',  ( -36.03906250000000000, -114.9929510916434339, 14.11852480586264846 ) ) ;
#21569 = DIRECTION ( 'NONE',  ( -1.000000000000000000, -1.734723475976807094E-16, 0.000000000000000000 ) ) ;
#21570 = CARTESIAN_POINT ( 'NONE',  ( -38.00000000000000711, -114.9929510916434339, 11.91443571948719615 ) ) ;
#21571 = CYLINDRICAL_SURFACE ( 'NONE', #1901, 6.765000000000044977 ) ;
#21572 = CARTESIAN_POINT ( 'NONE',  ( -34.50000000000000000, -114.1414532730574507, 9.517316564499758158 ) ) ;
#21573 = FACE_OUTER_BOUND ( 'NONE', #30491, .T. ) ;
#21574 = CYLINDRICAL_SURFACE ( 'NONE', #21851, 19.99999999999998579 ) ;
#21575 = CARTESIAN_POINT ( 'NONE',  ( 8.000000000000000000, 0.000000000000000000, 0.000000000000000000 ) ) ;
#21576 = VERTEX_POINT ( 'NONE', #3492 ) ;
#21577 = FACE_OUTER_BOUND ( 'NONE', #25115, .T. ) ;
#21578 = CARTESIAN_POINT ( 'NONE',  ( 2.000000000000001332, 3.643388353322724362E-16, -4.724999999999999645 ) ) ;
#21579 = AXIS2_PLACEMENT_3D ( 'NONE', #32682, #27282, #21864 ) ;
#21580 = ORIENTED_EDGE ( 'NONE', *, *, #269, .F. ) ;
#21581 = CARTESIAN_POINT ( 'NONE',  ( -37.46093750000000711, -114.9929510916434339, 13.11852480586264669 ) ) ;
#21582 = ORIENTED_EDGE ( 'NONE', *, *, #33891, .F. ) ;
#21583 = CARTESIAN_POINT ( 'NONE',  ( -38.99999999999999289, -113.9407375970686900, 8.253524454178448266 ) ) ;
#21584 = AXIS2_PLACEMENT_3D ( 'NONE', #3850, #31729, #15507 ) ;
#21585 = CYLINDRICAL_SURFACE ( 'NONE', #3639, 4.000000000000000000 ) ;
#21586 = ADVANCED_FACE ( 'NONE', ( #8870 ), #22549, .T. ) ;
#21587 = CIRCLE ( 'NONE', #2065, 14.00000000000000000 ) ;
#21588 = EDGE_LOOP ( 'NONE', ( #33355, #7484, #10383, #10469 ) ) ;
#21589 = VERTEX_POINT ( 'NONE', #30845 ) ;
#21590 = CARTESIAN_POINT ( 'NONE',  ( 0.000000000000000000, -46.77034588191320097, 22.72740077717213936 ) ) ;
#21591 = DIRECTION ( 'NONE',  ( 0.000000000000000000, 0.000000000000000000, 1.000000000000000000 ) ) ;
#21592 = EDGE_CURVE ( 'NONE', #10152, #31214, #24919, .T. ) ;
#21593 = VERTEX_POINT ( 'NONE', #11940 ) ;
#21594 = CARTESIAN_POINT ( 'NONE',  ( -36.94073759706866156, -111.0000000000000284, 5.628524454178450043 ) ) ;
#21595 = CYLINDRICAL_SURFACE ( 'NONE', #12093, 0.6000000000000028644 ) ;
#21596 = CARTESIAN_POINT ( 'NONE',  ( -4.000000000000000000, 0.000000000000000000, 65.00000000000000000 ) ) ;
#21597 = EDGE_LOOP ( 'NONE', ( #28818, #23623, #20346, #32830, #24442, #34914 ) ) ;
#21598 = ORIENTED_EDGE ( 'NONE', *, *, #6021, .F. ) ;
#21599 = EDGE_CURVE ( 'NONE', #13238, #7361, #14690, .T. ) ;
#21600 = DIRECTION ( 'NONE',  ( -0.000000000000000000, 0.000000000000000000, -1.000000000000000000 ) ) ;
#21601 = EDGE_CURVE ( 'NONE', #23381, #519, #35416, .T. ) ;
#21602 = DIRECTION ( 'NONE',  ( 5.339440136655842133E-16, 1.000000000000000000, -1.918536189538073087E-16 ) ) ;
#21603 = VERTEX_POINT ( 'NONE', #16791 ) ;
#21604 = ORIENTED_EDGE ( 'NONE', *, *, #15417, .F. ) ;
#21605 = CARTESIAN_POINT ( 'NONE',  ( -34.50000000000000000, -111.0140978167138570, -0.3747823525984258497 ) ) ;
#21606 = AXIS2_PLACEMENT_3D ( 'NONE', #20024, #20569, #34091 ) ;
#21607 = CARTESIAN_POINT ( 'NONE',  ( 0.000000000000000000, -2.710505431213761085E-17, 45.00000000000000000 ) ) ;
#21608 = EDGE_LOOP ( 'NONE', ( #22167, #30733, #16820, #23332 ) ) ;
#21609 = CARTESIAN_POINT ( 'NONE',  ( -35.50000000000000711, -114.9929510916434339, 10.51725893871048889 ) ) ;
#21610 = COLOUR_RGB ( '', 0.72549020, 0.75294118, 0.79215686) ;
#21611 = CIRCLE ( 'NONE', #15852, 20.00000000000000711 ) ;
#21612 = EDGE_CURVE ( 'NONE', #31611, #10641, #34275, .T. ) ;
#21613 = AXIS2_PLACEMENT_3D ( 'NONE', #32150, #8010, #32688 ) ;
#21614 = CARTESIAN_POINT ( 'NONE',  ( -34.50000000000000000, -113.9929510916434339, 12.26648026267477398 ) ) ;
#21615 = CYLINDRICAL_SURFACE ( 'NONE', #13167, 52.00000000000000711 ) ;
#21616 = CARTESIAN_POINT ( 'NONE',  ( 8.000000000000000000, 0.000000000000000000, 0.000000000000000000 ) ) ;
#21617 = CARTESIAN_POINT ( 'NONE',  ( -34.50000000000000000, -113.9948283797722439, 10.50648163149984171 ) ) ;
#21618 = CARTESIAN_POINT ( 'NONE',  ( -35.99181955245763476, -115.9929510916434481, 13.11847460610632510 ) ) ;
#21619 = VECTOR ( 'NONE', #9455, 1000.000000000000000 ) ;
#21620 = DIRECTION ( 'NONE',  ( -1.000000000000000000, -1.387778780781445922E-16, -0.000000000000000000 ) ) ;
#21621 = CARTESIAN_POINT ( 'NONE',  ( -34.49999999999998579, -25.98076211353322051, 84.99999999999992895 ) ) ;
#21622 = ORIENTED_EDGE ( 'NONE', *, *, #5727, .F. ) ;
#21623 = CARTESIAN_POINT ( 'NONE',  ( -1.000000000000014655, -4.808326913196006913, -0.7999999999999951594 ) ) ;
#21624 = DIRECTION ( 'NONE',  ( 0.000000000000000000, 0.7705132427757861446, 0.6374239897486934092 ) ) ;
#21625 = LINE ( 'NONE', #18586, #20849 ) ;
#21626 = ADVANCED_FACE ( 'NONE', ( #11229 ), #594, .T. ) ;
#21627 = AXIS2_PLACEMENT_3D ( 'NONE', #12249, #9545, #20511 ) ;
#21628 = VERTEX_POINT ( 'NONE', #16965 ) ;
#21629 = CARTESIAN_POINT ( 'NONE',  ( 0.000000000000000000, 0.000000000000000000, 55.00000000000000000 ) ) ;
#21630 = ORIENTED_EDGE ( 'NONE', *, *, #4078, .T. ) ;
#21631 = EDGE_CURVE ( 'NONE', #19641, #26822, #28514, .T. ) ;
#21632 = VECTOR ( 'NONE', #25951, 1000.000000000000000 ) ;
#21633 = CARTESIAN_POINT ( 'NONE',  ( -35.50000000000000000, -113.0140978167137717, 0.8903425666012282358 ) ) ;
#21634 = DIRECTION ( 'NONE',  ( 0.000000000000000000, 0.000000000000000000, 1.000000000000000000 ) ) ;
#21635 = EDGE_CURVE ( 'NONE', #22478, #27575, #420, .T. ) ;
#21636 = CARTESIAN_POINT ( 'NONE',  ( -35.50000000000000711, -114.9929510916434339, 11.21034663311131929 ) ) ;
#21637 = CARTESIAN_POINT ( 'NONE',  ( 8.000000000000000000, -12.96676809804139197, -13.60411018104332292 ) ) ;
#21638 = VECTOR ( 'NONE', #15284, 1000.000000000000000 ) ;
#21639 = AXIS2_PLACEMENT_3D ( 'NONE', #13809, #32718, #24796 ) ;
#21640 = ORIENTED_EDGE ( 'NONE', *, *, #32346, .F. ) ;
#21641 = AXIS2_PLACEMENT_3D ( 'NONE', #12305, #20574, #20747 ) ;
#21642 = LINE ( 'NONE', #21290, #19335 ) ;
#21643 = CARTESIAN_POINT ( 'NONE',  ( -35.50000000000000000, -112.8920926830253677, 2.874852253704053062 ) ) ;
#21644 = ORIENTED_EDGE ( 'NONE', *, *, #1787, .T. ) ;
#21645 = ORIENTED_EDGE ( 'NONE', *, *, #8591, .T. ) ;
#21646 = ADVANCED_FACE ( 'NONE', ( #33904 ), #28324, .T. ) ;
#21647 = CARTESIAN_POINT ( 'NONE',  ( -37.74901162816869515, -114.6652019342044042, 8.066024454178448266 ) ) ;
#21648 = EDGE_CURVE ( 'NONE', #12363, #35108, #4376, .T. ) ;
#21649 = TOROIDAL_SURFACE ( 'NONE', #30861, 5.015999999999992909, 0.04100000000000673939 ) ;
#21650 = FILL_AREA_STYLE ('',( #35017 ) ) ;
#21651 = VECTOR ( 'NONE', #19157, 1000.000000000000000 ) ;
#21652 = DIRECTION ( 'NONE',  ( -1.000000000000000000, -0.000000000000000000, -0.000000000000000000 ) ) ;
#21653 = ORIENTED_EDGE ( 'NONE', *, *, #5784, .F. ) ;
#21654 = VERTEX_POINT ( 'NONE', #22728 ) ;
#21655 = CARTESIAN_POINT ( 'NONE',  ( -34.50000000000000000, -113.0140978167138712, -0.4685323525984296800 ) ) ;
#21656 = CARTESIAN_POINT ( 'NONE',  ( -42.49999999999999289, -24.48076211353314591, 80.99999999999991473 ) ) ;
#21657 = CARTESIAN_POINT ( 'NONE',  ( -44.00000000000000000, 12.99999999999999822, 1.592040838891558898E-15 ) ) ;
#21658 = LINE ( 'NONE', #31145, #31773 ) ;
#21659 = AXIS2_PLACEMENT_3D ( 'NONE', #156, #24479, #16878 ) ;
#21660 = VECTOR ( 'NONE', #16960, 1000.000000000000000 ) ;
#21661 = CARTESIAN_POINT ( 'NONE',  ( -37.89983305244309975, -114.9929510916434339, 12.92579853460519246 ) ) ;
#21662 = CARTESIAN_POINT ( 'NONE',  ( 0.000000000000000000, 44.47301969247469344, -16.68249143361863318 ) ) ;
#21663 = DIRECTION ( 'NONE',  ( -1.000000000000000000, 0.000000000000000000, 0.000000000000000000 ) ) ;
#21664 = CARTESIAN_POINT ( 'NONE',  ( -34.50000000000000000, -112.0140900043366088, -0.5935324770972457697 ) ) ;
#21665 = CIRCLE ( 'NONE', #9026, 13.99999999999999645 ) ;
#21666 = AXIS2_PLACEMENT_3D ( 'NONE', #10365, #28910, #26940 ) ;
#21667 = CARTESIAN_POINT ( 'NONE',  ( -36.06250000000000711, -115.9929510916434481, 14.11852480586265024 ) ) ;
#21668 = CARTESIAN_POINT ( 'NONE',  ( 0.000000000000000000, -16.94522934049218676, 8.128228055638807348 ) ) ;
#21669 = CIRCLE ( 'NONE', #6715, 8.000000000000000000 ) ;
#21670 = AXIS2_PLACEMENT_3D ( 'NONE', #35041, #26570, #12883 ) ;
#21671 = CARTESIAN_POINT ( 'NONE',  ( 26.99999999999999289, 45.00000000000000711, 0.000000000000000000 ) ) ;
#21673 = ORIENTED_EDGE ( 'NONE', *, *, #6781, .T. ) ;
#21672 = AXIS2_PLACEMENT_3D ( 'NONE', #29673, #16505, #27519 ) ;
#21674 = CARTESIAN_POINT ( 'NONE',  ( -38.00000000000000711, -115.9929510916434481, 12.59102132592609102 ) ) ;
#21675 = CARTESIAN_POINT ( 'NONE',  ( -49.99999999999998579, -60.00000000000000000, -25.00000000000000000 ) ) ;
#21676 = CARTESIAN_POINT ( 'NONE',  ( 46.00000000000000000, 0.000000000000000000, -8.000000000000000000 ) ) ;
#21677 = AXIS2_PLACEMENT_3D ( 'NONE', #929, #22886, #28477 ) ;
#21678 = DIRECTION ( 'NONE',  ( 1.000000000000000000, -0.000000000000000000, -0.000000000000000000 ) ) ;
#21679 = CARTESIAN_POINT ( 'NONE',  ( -34.49999999999998579, -27.48076211353329157, 98.91941090707497608 ) ) ;
#21680 = EDGE_LOOP ( 'NONE', ( #16448, #8052, #18103, #6947 ) ) ;
#21681 = CARTESIAN_POINT ( 'NONE',  ( -30.00000000000000000, 2.571758278209441661E-15, 0.000000000000000000 ) ) ;
#21682 = DIRECTION ( 'NONE',  ( 1.110223024625156540E-16, 1.000000000000000000, 0.000000000000000000 ) ) ;
#21683 = ADVANCED_FACE ( 'NONE', ( #30326, #244 ), #33721, .F. ) ;
#21684 = CARTESIAN_POINT ( 'NONE',  ( 5.400000000000015454, -1.000000000000002220, 38.00000000000000000 ) ) ;
#21685 = DIRECTION ( 'NONE',  ( -1.000000000000000000, 0.000000000000000000, 0.000000000000000000 ) ) ;
#21686 = CARTESIAN_POINT ( 'NONE',  ( 0.000000000000000000, -3.678165988948685516, 15.05623113391066070 ) ) ;
#21687 = DIRECTION ( 'NONE',  ( -1.000000000000000000, 0.000000000000000000, 0.000000000000000000 ) ) ;
#21688 = VERTEX_POINT ( 'NONE', #9058 ) ;
#21689 = CIRCLE ( 'NONE', #22840, 3.799999999999999822 ) ;
#21690 = ORIENTED_EDGE ( 'NONE', *, *, #7880, .T. ) ;
#21691 = FACE_OUTER_BOUND ( 'NONE', #2342, .T. ) ;
#21692 = AXIS2_PLACEMENT_3D ( 'NONE', #16916, #24700, #33153 ) ;
#21693 = FACE_OUTER_BOUND ( 'NONE', #5944, .T. ) ;
#21694 = CARTESIAN_POINT ( 'NONE',  ( 4.000000000000000000, 4.898587196589412829E-16, 60.90000000000001279 ) ) ;
#21695 = VERTEX_POINT ( 'NONE', #20017 ) ;
#21696 = CARTESIAN_POINT ( 'NONE',  ( -35.00000000000000000, -113.9407375970686900, 6.996475545821551734 ) ) ;
#21697 = ORIENTED_EDGE ( 'NONE', *, *, #7348, .F. ) ;
#21698 = AXIS2_PLACEMENT_3D ( 'NONE', #13445, #26781, #29302 ) ;
#21699 = AXIS2_PLACEMENT_3D ( 'NONE', #17511, #33553, #6717 ) ;
#21700 =( NAMED_UNIT ( * ) PLANE_ANGLE_UNIT ( ) SI_UNIT ( $, .RADIAN. ) );
#21701 = ORIENTED_EDGE ( 'NONE', *, *, #22026, .F. ) ;
#21702 = ORIENTED_EDGE ( 'NONE', *, *, #13307, .F. ) ;
#21703 = DIRECTION ( 'NONE',  ( -1.000000000000000000, 0.000000000000000000, 0.000000000000000000 ) ) ;
#21704 = CIRCLE ( 'NONE', #12511, 47.49900000000001654 ) ;
#21705 = CARTESIAN_POINT ( 'NONE',  ( 0.000000000000000000, 0.000000000000000000, 0.000000000000000000 ) ) ;
#21706 = ORIENTED_EDGE ( 'NONE', *, *, #27500, .F. ) ;
#21707 = ORIENTED_EDGE ( 'NONE', *, *, #35246, .F. ) ;
#21708 = CARTESIAN_POINT ( 'NONE',  ( 7.999999999999992895, -36.06787431788650622, -37.45808914225528952 ) ) ;
#21709 = DIRECTION ( 'NONE',  ( -1.000000000000000000, -1.734723475976807094E-16, 0.000000000000000000 ) ) ;
#21710 = DIRECTION ( 'NONE',  ( 9.266685234918781277E-17, -6.938893903907202493E-17, -1.000000000000000000 ) ) ;
#21711 = CIRCLE ( 'NONE', #19433, 3.799999999999999822 ) ;
#21712 = CARTESIAN_POINT ( 'NONE',  ( 0.000000000000000000, -2.710505431213761085E-17, 55.00000000000000000 ) ) ;
#21713 = DIRECTION ( 'NONE',  ( -1.174092375852890260E-15, 4.222049128630259891E-16, 1.000000000000000000 ) ) ;
#21714 = VECTOR ( 'NONE', #6839, 1000.000000000000000 ) ;
#21715 = CARTESIAN_POINT ( 'NONE',  ( 0.000000000000000000, -5.482169781018729537, -16.00140663693126086 ) ) ;
#21716 = CARTESIAN_POINT ( 'NONE',  ( -36.87500000000098765, -115.9929510916434481, 14.11852480586265024 ) ) ;
#21717 = DIRECTION ( 'NONE',  ( -1.000000000000000000, -0.000000000000000000, -0.000000000000000000 ) ) ;
#21718 = CIRCLE ( 'NONE', #21128, 20.00000000000000355 ) ;
#21719 = DIRECTION ( 'NONE',  ( -1.000000000000000000, 0.000000000000000000, 0.000000000000000000 ) ) ;
#21720 = CIRCLE ( 'NONE', #17111, 9.499000000000011212 ) ;
#21721 = DIRECTION ( 'NONE',  ( 0.000000000000000000, -0.9848077530122097967, 0.1736481776669208388 ) ) ;
#21722 = DIRECTION ( 'NONE',  ( -1.000000000000000000, 0.000000000000000000, 0.000000000000000000 ) ) ;
#21723 = EDGE_CURVE ( 'NONE', #31137, #22200, #23927, .T. ) ;
#21724 = DIRECTION ( 'NONE',  ( 0.000000000000000000, 0.000000000000000000, -1.000000000000000000 ) ) ;
#21725 = CARTESIAN_POINT ( 'NONE',  ( 8.000000000000000000, 16.53603053422208902, -8.931325931664652273 ) ) ;
#21726 = ORIENTED_EDGE ( 'NONE', *, *, #14808, .F. ) ;
#21727 = CARTESIAN_POINT ( 'NONE',  ( -38.30190309005061522, -111.0245472910330022, 8.027725545821551734 ) ) ;
#21728 = DIRECTION ( 'NONE',  ( -1.000000000000000000, 0.000000000000000000, -0.000000000000000000 ) ) ;
#21729 = DIRECTION ( 'NONE',  ( -1.000000000000000000, 0.000000000000000000, 0.000000000000000000 ) ) ;
#21730 = CARTESIAN_POINT ( 'NONE',  ( 8.000000000000000000, -6.860320204751237938, 13.89802171851381551 ) ) ;
#21731 = EDGE_LOOP ( 'NONE', ( #18920, #3760, #17072, #9508 ) ) ;
#21732 = ORIENTED_EDGE ( 'NONE', *, *, #28317, .T. ) ;
#21733 = DIRECTION ( 'NONE',  ( -1.000000000000000000, 0.000000000000000000, 0.000000000000000000 ) ) ;
#21734 = DIRECTION ( 'NONE',  ( -1.000000000000000000, -0.000000000000000000, 0.000000000000000000 ) ) ;
#21735 = ORIENTED_EDGE ( 'NONE', *, *, #11535, .F. ) ;
#21736 = EDGE_CURVE ( 'NONE', #24945, #17756, #5662, .T. ) ;
#21737 = ORIENTED_EDGE ( 'NONE', *, *, #17563, .F. ) ;
#21738 = PLANE ( 'NONE',  #851 ) ;
#21739 = CARTESIAN_POINT ( 'NONE',  ( -3.799999999999999822, 0.000000000000000000, -40.40000000000000568 ) ) ;
#21740 = AXIS2_PLACEMENT_3D ( 'NONE', #110, #30710, #281 ) ;
#21741 = CARTESIAN_POINT ( 'NONE',  ( 30.00000000000000000, 1.387778780781445676E-14, 70.00000000000000000 ) ) ;
#21742 = DIRECTION ( 'NONE',  ( 1.000000000000000000, -0.000000000000000000, -0.000000000000000000 ) ) ;
#21743 = VERTEX_POINT ( 'NONE', #33368 ) ;
#21744 = ORIENTED_EDGE ( 'NONE', *, *, #7994, .F. ) ;
#21745 = AXIS2_PLACEMENT_3D ( 'NONE', #11640, #12188, #9126 ) ;
#21746 = CARTESIAN_POINT ( 'NONE',  ( 7.999999999999992895, -30.93515269692089120, -36.04401931830286543 ) ) ;
#21747 = DIRECTION ( 'NONE',  ( -1.174092375852890260E-15, 4.222049128630259891E-16, 1.000000000000000000 ) ) ;
#21748 = VERTEX_POINT ( 'NONE', #16620 ) ;
#21749 = AXIS2_PLACEMENT_3D ( 'NONE', #24280, #21733, #27333 ) ;
#21750 = CARTESIAN_POINT ( 'NONE',  ( -37.49999999999999289, -11.52052244843579309, 115.1848168619253698 ) ) ;
#21751 = CARTESIAN_POINT ( 'NONE',  ( -34.50000000000000000, -112.2144317118258527, -1.239329810084414341 ) ) ;
#21752 = CARTESIAN_POINT ( 'NONE',  ( -36.00976557831293690, -114.9929510916434339, 14.11852773550420359 ) ) ;
#21753 = CARTESIAN_POINT ( 'NONE',  ( -42.49999999999999289, -42.98076211353323828, 83.49999999999991473 ) ) ;
#21754 = CARTESIAN_POINT ( 'NONE',  ( -35.50000000000000000, -113.9948283797722439, 10.50648163149984171 ) ) ;
#21755 = CARTESIAN_POINT ( 'NONE',  ( 0.000000000000000000, 43.83938735307295076, -18.28286404005752175 ) ) ;
#21756 = CARTESIAN_POINT ( 'NONE',  ( -35.93867112612154813, -114.9929510916434339, 14.11732072679899197 ) ) ;
#21757 = LINE ( 'NONE', #27714, #25122 ) ;
#21758 = CARTESIAN_POINT ( 'NONE',  ( 0.000000000000000000, -47.49120266317497396, 0.8606222198173640869 ) ) ;
#21759 = DIRECTION ( 'NONE',  ( -1.000000000000000000, 0.000000000000000000, 0.000000000000000000 ) ) ;
#21760 = EDGE_LOOP ( 'NONE', ( #14869, #25420 ) ) ;
#21761 = CARTESIAN_POINT ( 'NONE',  ( 8.000000000000000000, 16.59870953437685515, -3.253005020243678214 ) ) ;
#21762 = DIRECTION ( 'NONE',  ( -1.000000000000000000, 0.000000000000000000, 0.000000000000000000 ) ) ;
#21763 = ADVANCED_FACE ( 'NONE', ( #2971 ), #13930, .T. ) ;
#21764 = VERTEX_POINT ( 'NONE', #7239 ) ;
#21765 = EDGE_CURVE ( 'NONE', #22834, #8928, #12473, .T. ) ;
#21766 = CARTESIAN_POINT ( 'NONE',  ( -36.24999999999983658, -114.9929510916434339, 13.11852480586264669 ) ) ;
#21767 = ORIENTED_EDGE ( 'NONE', *, *, #28925, .T. ) ;
#21768 = VECTOR ( 'NONE', #16821, 1000.000000000000000 ) ;
#21769 = CARTESIAN_POINT ( 'NONE',  ( -36.23083527818512550, -116.0245472910329880, 7.784774454178451819 ) ) ;
#21770 = VECTOR ( 'NONE', #32974, 1000.000000000000000 ) ;
#21771 = CARTESIAN_POINT ( 'NONE',  ( 0.000000000000000000, -2.710505431213761085E-17, -30.00000000000000711 ) ) ;
#21772 = ORIENTED_EDGE ( 'NONE', *, *, #34360, .F. ) ;
#21773 = AXIS2_PLACEMENT_3D ( 'NONE', #17717, #34115, #28715 ) ;
#21774 = VERTEX_POINT ( 'NONE', #6707 ) ;
#21775 = DIRECTION ( 'NONE',  ( -1.000000000000000000, 0.000000000000000000, 0.000000000000000000 ) ) ;
#21776 = CARTESIAN_POINT ( 'NONE',  ( 0.000000000000000000, -27.79676263918161894, -37.88001506494798321 ) ) ;
#21777 = EDGE_CURVE ( 'NONE', #4539, #30241, #14134, .T. ) ;
#21778 = ORIENTED_EDGE ( 'NONE', *, *, #24826, .F. ) ;
#21779 = CARTESIAN_POINT ( 'NONE',  ( -40.02454729103296671, -115.1833782841879525, 6.659774454178448266 ) ) ;
#21780 = ADVANCED_FACE ( 'NONE', ( #12291 ), #34082, .T. ) ;
#21781 = DIRECTION ( 'NONE',  ( 0.000000000000000000, 0.000000000000000000, 1.000000000000000000 ) ) ;
#21782 = CARTESIAN_POINT ( 'NONE',  ( 8.000000000000007105, -9.919332006307262972, 5.363026430117087351 ) ) ;
#21783 = EDGE_LOOP ( 'NONE', ( #6117, #1454, #27738, #9300 ) ) ;
#21784 = ORIENTED_EDGE ( 'NONE', *, *, #3953, .F. ) ;
#21785 = DIRECTION ( 'NONE',  ( -1.000000000000000000, 0.000000000000000000, 0.000000000000000000 ) ) ;
#21786 = SURFACE_SIDE_STYLE ('',( #32255 ) ) ;
#21787 = FACE_OUTER_BOUND ( 'NONE', #12130, .T. ) ;
#21788 = VERTEX_POINT ( 'NONE', #1677 ) ;
#21789 = ORIENTED_EDGE ( 'NONE', *, *, #18068, .T. ) ;
#21790 = CARTESIAN_POINT ( 'NONE',  ( -34.50000000000000000, -112.7319952733504635, 2.855726801009121463 ) ) ;
#21791 = CIRCLE ( 'NONE', #28753, 8.000000000000001776 ) ;
#21792 = LINE ( 'NONE', #16379, #5302 ) ;
#21793 = ORIENTED_EDGE ( 'NONE', *, *, #11387, .T. ) ;
#21794 = CARTESIAN_POINT ( 'NONE',  ( -35.50000000000000711, -114.0743172650041686, 9.508870970061893857 ) ) ;
#21795 = EDGE_CURVE ( 'NONE', #30905, #34581, #29034, .T. ) ;
#21796 = CIRCLE ( 'NONE', #34466, 3.799999999999999822 ) ;
#21797 = CARTESIAN_POINT ( 'NONE',  ( -36.03906250000000000, -113.9929510916434339, 14.11852480586265024 ) ) ;
#21798 = CARTESIAN_POINT ( 'NONE',  ( 4.000000000000003553, 19.74581912682909390, -48.10512059033372623 ) ) ;
#21799 = CARTESIAN_POINT ( 'NONE',  ( -3.799999999999999822, 0.000000000000000000, -50.00000000000000000 ) ) ;
#21800 = MECHANICAL_DESIGN_GEOMETRIC_PRESENTATION_REPRESENTATION (  '', ( #20061 ), #6288 ) ;
#21801 = CARTESIAN_POINT ( 'NONE',  ( -34.50000000000000000, -113.9929510916434339, 12.60752341388803721 ) ) ;
#21803 = DIRECTION ( 'NONE',  ( 0.000000000000000000, 0.000000000000000000, -1.000000000000000000 ) ) ;
#21802 = CIRCLE ( 'NONE', #2311, 4.000000000000000000 ) ;
#21804 = CARTESIAN_POINT ( 'NONE',  ( -38.00000000000000711, -115.9929510916434481, 11.73841344789285657 ) ) ;
#21805 = CARTESIAN_POINT ( 'NONE',  ( 0.000000000000000000, 17.06000345190455647, -10.43821259704003523 ) ) ;
#21806 = DIRECTION ( 'NONE',  ( -1.000000000000000000, 0.000000000000000000, 0.000000000000000000 ) ) ;
#21807 = ADVANCED_FACE ( 'NONE', ( #12659 ), #23636, .T. ) ;
#21808 = EDGE_CURVE ( 'NONE', #180, #34183, #18742, .T. ) ;
#21809 = VERTEX_POINT ( 'NONE', #1308 ) ;
#21810 = EDGE_CURVE ( 'NONE', #14212, #31835, #2655, .T. ) ;
#21811 = DIRECTION ( 'NONE',  ( 0.000000000000000000, 0.000000000000000000, 1.000000000000000000 ) ) ;
#21812 = CARTESIAN_POINT ( 'NONE',  ( 0.000000000000000000, -21.63912866391140710, 3.968388925834730685 ) ) ;
#21813 = PLANE ( 'NONE',  #7094 ) ;
#21814 = ORIENTED_EDGE ( 'NONE', *, *, #27375, .F. ) ;
#21815 = CARTESIAN_POINT ( 'NONE',  ( -1.498621416870348888, 9.750686088500505778E-16, 4.980000000000000426 ) ) ;
#21816 = VERTEX_POINT ( 'NONE', #34623 ) ;
#21817 = CARTESIAN_POINT ( 'NONE',  ( -35.50000000000000000, -113.0140978167137717, 0.8752176474015607166 ) ) ;
#21818 = CARTESIAN_POINT ( 'NONE',  ( -0.3000000000000016542, -14.69693845669907439, -1.200000000000006617 ) ) ;
#21819 = CARTESIAN_POINT ( 'NONE',  ( -37.74901162816869515, -114.6652019342044042, 8.066024454178448266 ) ) ;
#21820 = VECTOR ( 'NONE', #8373, 1000.000000000000000 ) ;
#21821 = CARTESIAN_POINT ( 'NONE',  ( -35.50000000000000711, -114.9929510916434339, 12.59652202191340642 ) ) ;
#21822 = LINE ( 'NONE', #25062, #7874 ) ;
#21823 = EDGE_CURVE ( 'NONE', #30224, #14334, #28688, .T. ) ;
#21824 = ORIENTED_EDGE ( 'NONE', *, *, #10023, .F. ) ;
#21825 = AXIS2_PLACEMENT_3D ( 'NONE', #12778, #20141, #6474 ) ;
#21826 = CARTESIAN_POINT ( 'NONE',  ( -42.49999999999999289, -13.10640646055107084, 90.70096189432331357 ) ) ;
#21827 = CARTESIAN_POINT ( 'NONE',  ( -35.50000000000000000, -111.4147656069378058, -1.853877267569947529 ) ) ;
#21828 = VERTEX_POINT ( 'NONE', #4210 ) ;
#21829 = ORIENTED_EDGE ( 'NONE', *, *, #7100, .F. ) ;
#21830 = CARTESIAN_POINT ( 'NONE',  ( -37.05926240293131713, -115.9999999999999858, 3.378524454178448710 ) ) ;
#21831 = AXIS2_PLACEMENT_3D ( 'NONE', #22423, #5707, #16667 ) ;
#21832 = ORIENTED_EDGE ( 'NONE', *, *, #24081, .F. ) ;
#21833 = AXIS2_PLACEMENT_3D ( 'NONE', #3217, #24995, #11480 ) ;
#21834 = ADVANCED_FACE ( 'NONE', ( #1141 ), #18219, .T. ) ;
#21835 = DIRECTION ( 'NONE',  ( 0.000000000000000000, 0.000000000000000000, 1.000000000000000000 ) ) ;
#21836 = ORIENTED_EDGE ( 'NONE', *, *, #23028, .F. ) ;
#21837 = ORIENTED_EDGE ( 'NONE', *, *, #6475, .T. ) ;
#21838 = CARTESIAN_POINT ( 'NONE',  ( -34.50000000000000000, -115.0140978167138712, -0.6247823525984407267 ) ) ;
#21839 = CARTESIAN_POINT ( 'NONE',  ( -46.00000000000000000, 0.000000000000000000, 78.00000000000001421 ) ) ;
#21840 = CARTESIAN_POINT ( 'NONE',  ( -46.00000000000000000, -25.98076211353320275, 73.99999999999992895 ) ) ;
#21841 = EDGE_CURVE ( 'NONE', #17706, #334, #32517, .T. ) ;
#21842 = DIRECTION ( 'NONE',  ( -1.000000000000000000, 0.000000000000000000, 0.000000000000000000 ) ) ;
#21843 = CARTESIAN_POINT ( 'NONE',  ( -35.50000000000000000, -113.9929510916433060, 10.50625754673589540 ) ) ;
#21844 = EDGE_CURVE ( 'NONE', #34282, #14117, #1861, .T. ) ;
#21845 = PLANE ( 'NONE',  #2346 ) ;
#21846 = VECTOR ( 'NONE', #34658, 1000.000000000000000 ) ;
#21847 = CARTESIAN_POINT ( 'NONE',  ( 0.000000000000000000, 3.975523202428290936, -13.42368113696666754 ) ) ;
#21848 = CARTESIAN_POINT ( 'NONE',  ( -34.50000000000000000, -115.0795240838853886, -1.623175561345890472 ) ) ;
#21849 = CARTESIAN_POINT ( 'NONE',  ( -35.50000000000000000, -114.2067765580549832, 8.517583185305328541 ) ) ;
#21850 = CARTESIAN_POINT ( 'NONE',  ( 0.000000000000000000, -2.710505431213761085E-17, 38.90000000000000568 ) ) ;
#21851 = AXIS2_PLACEMENT_3D ( 'NONE', #7386, #17991, #26482 ) ;
#21852 = EDGE_CURVE ( 'NONE', #14203, #16940, #903, .T. ) ;
#21853 = FACE_OUTER_BOUND ( 'NONE', #15050, .T. ) ;
#21854 = ORIENTED_EDGE ( 'NONE', *, *, #28476, .F. ) ;
#21855 = VECTOR ( 'NONE', #5154, 1000.000000000000000 ) ;
#21856 = CARTESIAN_POINT ( 'NONE',  ( -37.62959469683911351, -115.9929510916434481, 13.10254527216511633 ) ) ;
#21857 = CARTESIAN_POINT ( 'NONE',  ( 0.000000000000000000, -37.91532898920942074, 28.61088654061626357 ) ) ;
#21858 = ADVANCED_FACE ( 'NONE', ( #7060 ), #18037, .T. ) ;
#21859 = CARTESIAN_POINT ( 'NONE',  ( -39.49999999999999289, -12.31102132296306451, 91.73752798680880005 ) ) ;
#21860 = CONTEXT_DEPENDENT_SHAPE_REPRESENTATION ( #22101, #27395 ) ;
#21861 = PLANE ( 'NONE',  #33764 ) ;
#21862 = ORIENTED_EDGE ( 'NONE', *, *, #15402, .F. ) ;
#21863 = CYLINDRICAL_SURFACE ( 'NONE', #16479, 4.800000000000000711 ) ;
#21864 = DIRECTION ( 'NONE',  ( 0.000000000000000000, 0.000000000000000000, 1.000000000000000000 ) ) ;
#21865 = LINE ( 'NONE', #16632, #6741 ) ;
#21866 = CARTESIAN_POINT ( 'NONE',  ( 3.799999999999999822, 0.000000000000000000, 35.10000000000000142 ) ) ;
#21867 = CONTEXT_DEPENDENT_SHAPE_REPRESENTATION ( #12440, #21012 ) ;
#21868 = DIRECTION ( 'NONE',  ( -1.000000000000000000, 0.000000000000000000, 0.000000000000000000 ) ) ;
#21869 = LINE ( 'NONE', #4627, #28543 ) ;
#21870 = ORIENTED_EDGE ( 'NONE', *, *, #25819, .T. ) ;
#21871 = ORIENTED_EDGE ( 'NONE', *, *, #10966, .F. ) ;
#21872 = CARTESIAN_POINT ( 'NONE',  ( 8.000000000000007105, -5.363026430117185051, 9.919332006307207905 ) ) ;
#21873 = CARTESIAN_POINT ( 'NONE',  ( 46.00000000000000000, -25.98076211353320275, 73.99999999999992895 ) ) ;
#21874 = CARTESIAN_POINT ( 'NONE',  ( 8.000000000000000000, -4.460989585141086344, 16.92083251265324151 ) ) ;
#21875 = ORIENTED_EDGE ( 'NONE', *, *, #11219, .T. ) ;
#21876 = VECTOR ( 'NONE', #19310, 1000.000000000000000 ) ;
#21877 = CARTESIAN_POINT ( 'NONE',  ( -38.45611840935523418, -112.6276912846090568, 9.433975545821551734 ) ) ;
#21878 = EDGE_LOOP ( 'NONE', ( #7770, #34684 ) ) ;
#21879 = CONTEXT_DEPENDENT_SHAPE_REPRESENTATION ( #16098, #33141 ) ;
#21880 = ORIENTED_EDGE ( 'NONE', *, *, #22725, .F. ) ;
#21881 = CIRCLE ( 'NONE', #12690, 0.5000000000000004441 ) ;
#21882 = ORIENTED_EDGE ( 'NONE', *, *, #27913, .T. ) ;
#21883 = DIRECTION ( 'NONE',  ( 0.000000000000000000, 0.000000000000000000, 1.000000000000000000 ) ) ;
#21884 = AXIS2_PLACEMENT_3D ( 'NONE', #18231, #34271, #15518 ) ;
#21885 = AXIS2_PLACEMENT_3D ( 'NONE', #28094, #25033, #14554 ) ;
#21886 = ADVANCED_FACE ( 'NONE', ( #12833 ), #23815, .T. ) ;
#21887 = DIRECTION ( 'NONE',  ( 0.000000000000000000, 0.8660254037844398178, -0.4999999999999977796 ) ) ;
#21888 = ORIENTED_EDGE ( 'NONE', *, *, #7479, .T. ) ;
#21889 = EDGE_CURVE ( 'NONE', #8987, #25674, #14165, .T. ) ;
#21890 = CARTESIAN_POINT ( 'NONE',  ( -35.50000000000000711, -114.9929517792218689, 10.50900788599415314 ) ) ;
#21891 = CYLINDRICAL_SURFACE ( 'NONE', #13765, 19.99999999999998579 ) ;
#21892 = PLANE ( 'NONE',  #21154 ) ;
#21893 = LINE ( 'NONE', #10747, #25746 ) ;
#21894 = CYLINDRICAL_SURFACE ( 'NONE', #12837, 15.49899999999998457 ) ;
#21895 = CIRCLE ( 'NONE', #6348, 47.49900000000001654 ) ;
#21896 = DIRECTION ( 'NONE',  ( 1.000000000000000000, 0.000000000000000000, -0.000000000000000000 ) ) ;
#21897 = CARTESIAN_POINT ( 'NONE',  ( -36.01562499999997158, -115.9929510916434481, 14.11852480586265024 ) ) ;
#21898 = DIRECTION ( 'NONE',  ( 0.000000000000000000, -0.4999999999999890643, -0.8660254037844449249 ) ) ;
#21899 = DIRECTION ( 'NONE',  ( 0.000000000000000000, 0.000000000000000000, -1.000000000000000000 ) ) ;
#21900 = DIRECTION ( 'NONE',  ( -1.174092375852890260E-15, 4.222049128630259891E-16, 1.000000000000000000 ) ) ;
#21901 = PLANE ( 'NONE',  #874 ) ;
#21902 = DIRECTION ( 'NONE',  ( 0.000000000000000000, 0.000000000000000000, 1.000000000000000000 ) ) ;
#21903 =( NAMED_UNIT ( * ) PLANE_ANGLE_UNIT ( ) SI_UNIT ( $, .RADIAN. ) );
#21904 = ORIENTED_EDGE ( 'NONE', *, *, #12544, .F. ) ;
#21905 = CIRCLE ( 'NONE', #10996, 4.800000000000000711 ) ;
#21906 = COLOUR_RGB ( '', 0.72549020, 0.75294118, 0.79215686) ;
#21907 = CARTESIAN_POINT ( 'NONE',  ( -35.54388159064475872, -115.3723087153909432, 7.183975545821551734 ) ) ;
#21908 = AXIS2_PLACEMENT_3D ( 'NONE', #11307, #27530, #16516 ) ;
#21909 = CARTESIAN_POINT ( 'NONE',  ( 7.999999999999992895, -26.17370628620682638, 39.63700417846155233 ) ) ;
#21910 = CARTESIAN_POINT ( 'NONE',  ( 55.00000000000000711, -25.98076211353320986, 77.99999999999992895 ) ) ;
#21911 = DIRECTION ( 'NONE',  ( -1.000000000000000000, 0.000000000000000000, 0.000000000000000000 ) ) ;
#21912 = ORIENTED_EDGE ( 'NONE', *, *, #25529, .T. ) ;
#21913 = ORIENTED_EDGE ( 'NONE', *, *, #32356, .F. ) ;
#21914 = CARTESIAN_POINT ( 'NONE',  ( 7.999999999999992895, -42.60732521687556584, -19.80331771201704427 ) ) ;
#21915 = CARTESIAN_POINT ( 'NONE',  ( 0.000000000000000000, -21.63912866391137868, -3.968388925835033554 ) ) ;
#21916 = VERTEX_POINT ( 'NONE', #12116 ) ;
#21917 = ORIENTED_EDGE ( 'NONE', *, *, #17892, .T. ) ;
#21918 = CARTESIAN_POINT ( 'NONE',  ( 0.3000000000000016542, -14.69693845669907439, -1.200000000000006617 ) ) ;
#21919 = CARTESIAN_POINT ( 'NONE',  ( 0.000000000000000000, 0.3212489022565391261, 16.91141623315867193 ) ) ;
#21920 = AXIS2_PLACEMENT_3D ( 'NONE', #34170, #28942, #34350 ) ;
#21921 = DIRECTION ( 'NONE',  ( 1.110223024625156540E-16, -0.9396926207859082059, 0.3420201433256693790 ) ) ;
#21922 = FACE_OUTER_BOUND ( 'NONE', #7996, .T. ) ;
#21923 = VERTEX_POINT ( 'NONE', #5098 ) ;
#21924 = VERTEX_POINT ( 'NONE', #29930 ) ;
#21925 = EDGE_CURVE ( 'NONE', #31088, #16992, #935, .T. ) ;
#21926 = CARTESIAN_POINT ( 'NONE',  ( -34.49999999999998579, -25.98076211353322051, 84.99999999999992895 ) ) ;
#21927 = CARTESIAN_POINT ( 'NONE',  ( 7.999999999999992895, 0.000000000000000000, 0.000000000000000000 ) ) ;
#21928 = CIRCLE ( 'NONE', #21359, 13.99999999999999645 ) ;
#21929 = ORIENTED_EDGE ( 'NONE', *, *, #23774, .T. ) ;
#21930 = CIRCLE ( 'NONE', #11025, 4.000000000000000000 ) ;
#21931 = CARTESIAN_POINT ( 'NONE',  ( 0.000000000000000000, 0.000000000000000000, 35.10000000000000142 ) ) ;
#21932 = CARTESIAN_POINT ( 'NONE',  ( -34.50000000000000000, -112.9486715495423681, -1.623175561345890472 ) ) ;
#21933 = CARTESIAN_POINT ( 'NONE',  ( -35.80421860361284558, -114.9929510916434339, 14.10650203519841916 ) ) ;
#21934 = CARTESIAN_POINT ( 'NONE',  ( -35.50000000000000000, -113.9836614335179377, 10.50514867547815534 ) ) ;
#21935 = CARTESIAN_POINT ( 'NONE',  ( -42.49999999999999289, -26.38406014851792847, 79.52301627764165914 ) ) ;
#21936 = ADVANCED_FACE ( 'NONE', ( #27412 ), #4747, .T. ) ;
#21937 = CARTESIAN_POINT ( 'NONE',  ( -35.51674767832921731, -114.9929510916434339, 14.04194344061634503 ) ) ;
#21938 = DIRECTION ( 'NONE',  ( -1.000000000000000000, -0.000000000000000000, 0.000000000000000000 ) ) ;
#21939 = LINE ( 'NONE', #30061, #8053 ) ;
#21940 = CARTESIAN_POINT ( 'NONE',  ( 8.000000000000000000, -7.317194182740271557, 18.61340026142649151 ) ) ;
#21941 = CARTESIAN_POINT ( 'NONE',  ( 0.000000000000000000, -47.22458491092824318, 5.098390039074071289 ) ) ;
#21942 = DIRECTION ( 'NONE',  ( 0.000000000000000000, 0.000000000000000000, 1.000000000000000000 ) ) ;
#21943 = DIRECTION ( 'NONE',  ( -1.000000000000000000, 4.524158825347490025E-15, 1.174092375852883357E-15 ) ) ;
#21944 = VERTEX_POINT ( 'NONE', #24001 ) ;
#21945 = DIRECTION ( 'NONE',  ( -1.000000000000000000, 0.000000000000000000, -0.000000000000000000 ) ) ;
#21946 = ORIENTED_EDGE ( 'NONE', *, *, #21795, .T. ) ;
#21947 = CARTESIAN_POINT ( 'NONE',  ( -34.00000000000000000, -114.0592624029313242, 3.003524454178448710 ) ) ;
#21948 = DIRECTION ( 'NONE',  ( 1.000000000000000000, 0.000000000000000000, -1.691777834109591283E-31 ) ) ;
#21949 = ORIENTED_EDGE ( 'NONE', *, *, #29137, .T. ) ;
#21950 = ORIENTED_EDGE ( 'NONE', *, *, #33602, .T. ) ;
#21951 = DIRECTION ( 'NONE',  ( 0.000000000000000000, 0.000000000000000000, 1.000000000000000000 ) ) ;
#21952 = LINE ( 'NONE', #19247, #4268 ) ;
#21953 = AXIS2_PLACEMENT_3D ( 'NONE', #19263, #2750, #24690 ) ;
#21954 = VERTEX_POINT ( 'NONE', #13197 ) ;
#21955 = AXIS2_PLACEMENT_3D ( 'NONE', #31231, #34116, #6554 ) ;
#21956 = CARTESIAN_POINT ( 'NONE',  ( -33.97545270896703329, -115.1833782841879810, 4.090225545821551734 ) ) ;
#21957 = CARTESIAN_POINT ( 'NONE',  ( 8.000000000000000000, 14.48509162075963985, 8.733917826871412160 ) ) ;
#21958 = CYLINDRICAL_SURFACE ( 'NONE', #7315, 52.00000000000000711 ) ;
#21959 = ORIENTED_EDGE ( 'NONE', *, *, #14067, .T. ) ;
#21960 = ORIENTED_EDGE ( 'NONE', *, *, #20713, .T. ) ;
#21961 = CARTESIAN_POINT ( 'NONE',  ( 4.000000000000003553, 51.93417535146742381, -2.615612846549375536 ) ) ;
#21962 = FILL_AREA_STYLE ('',( #33650 ) ) ;
#21963 = DIRECTION ( 'NONE',  ( 1.000000000000000000, -0.000000000000000000, -0.000000000000000000 ) ) ;
#21964 = VERTEX_POINT ( 'NONE', #26703 ) ;
#21965 = ORIENTED_EDGE ( 'NONE', *, *, #631, .T. ) ;
#21966 = CIRCLE ( 'NONE', #16792, 20.00000000000000711 ) ;
#21967 = CARTESIAN_POINT ( 'NONE',  ( -34.50000000000000000, -117.0140978167138854, 0.0002176474015577929428 ) ) ;
#21968 = EDGE_CURVE ( 'NONE', #26304, #2304, #12424, .T. ) ;
#21969 = EDGE_CURVE ( 'NONE', #2504, #32249, #33146, .T. ) ;
#21970 = FACE_OUTER_BOUND ( 'NONE', #21293, .T. ) ;
#21971 = ORIENTED_EDGE ( 'NONE', *, *, #28893, .F. ) ;
#21972 = DIRECTION ( 'NONE',  ( 1.000000000000000000, 0.000000000000000000, 0.000000000000000000 ) ) ;
#21973 = CARTESIAN_POINT ( 'NONE',  ( -34.50000000000000000, -113.9929510916434339, 10.72628538622835670 ) ) ;
#21974 = CIRCLE ( 'NONE', #33490, 7.200000000000005507 ) ;
#21975 = CARTESIAN_POINT ( 'NONE',  ( 0.000000000000000000, 0.000000000000000000, -34.40000000000000568 ) ) ;
#21976 = DIRECTION ( 'NONE',  ( 0.000000000000000000, 0.9659258262890656477, 0.2588190451025308425 ) ) ;
#21977 = ADVANCED_FACE ( 'NONE', ( #27056 ), #4917, .T. ) ;
#21978 = AXIS2_PLACEMENT_3D ( 'NONE', #2126, #7327, #2472 ) ;
#21979 = CIRCLE ( 'NONE', #32347, 4.000000000000000000 ) ;
#21980 = CARTESIAN_POINT ( 'NONE',  ( -34.50000000000000000, -113.9929510916432207, 10.50625754673563250 ) ) ;
#21981 = CARTESIAN_POINT ( 'NONE',  ( -39.00000000000000711, -114.9929510916434339, 10.50625754673587231 ) ) ;
#21982 = CARTESIAN_POINT ( 'NONE',  ( -35.50000000000000711, -114.9929296450195721, 10.49869535309826674 ) ) ;
#21983 = DIRECTION ( 'NONE',  ( 0.000000000000000000, 0.8660254037844398178, -0.4999999999999977796 ) ) ;
#21984 = CARTESIAN_POINT ( 'NONE',  ( 0.000000000000000000, 0.000000000000000000, 0.000000000000000000 ) ) ;
#21985 = ORIENTED_EDGE ( 'NONE', *, *, #12632, .T. ) ;
#21986 = EDGE_LOOP ( 'NONE', ( #1118, #2720, #11000, #22690 ) ) ;
#21987 = DIRECTION ( 'NONE',  ( -1.000000000000000000, 0.000000000000000000, 0.000000000000000000 ) ) ;
#21988 = FACE_OUTER_BOUND ( 'NONE', #29870, .T. ) ;
#21989 = EDGE_LOOP ( 'NONE', ( #15663, #8272 ) ) ;
#21990 = AXIS2_PLACEMENT_3D ( 'NONE', #18344, #4690, #34566 ) ;
#21991 = CARTESIAN_POINT ( 'NONE',  ( 0.000000000000000000, 0.000000000000000000, 0.000000000000000000 ) ) ;
#21992 = EDGE_LOOP ( 'NONE', ( #11169, #4889 ) ) ;
#21993 = AXIS2_PLACEMENT_3D ( 'NONE', #19873, #28362, #8560 ) ;
#21994 = CARTESIAN_POINT ( 'NONE',  ( -35.50000000000000000, -113.0140978167138712, 0.6252176474015680441 ) ) ;
#21995 = CARTESIAN_POINT ( 'NONE',  ( 3.872983346207517386, -1.000000000000028644, 55.00000000000000711 ) ) ;
#21996 = CARTESIAN_POINT ( 'NONE',  ( -37.97545270896701908, -113.5265240346955977, 5.347274454178449155 ) ) ;
#21997 = CYLINDRICAL_SURFACE ( 'NONE', #7319, 4.800000000000000711 ) ;
#21998 = EDGE_CURVE ( 'NONE', #32241, #24079, #23952, .T. ) ;
#21999 = VERTEX_POINT ( 'NONE', #21805 ) ;
#22000 = CARTESIAN_POINT ( 'NONE',  ( -49.99999999999999289, -25.98076211353320275, 76.99999999999992895 ) ) ;
#22001 = AXIS2_PLACEMENT_3D ( 'NONE', #22915, #250, #25634 ) ;
#22002 = CARTESIAN_POINT ( 'NONE',  ( -35.50000000000000000, -115.2751396785629510, -2.608751991713152307 ) ) ;
#22003 = CIRCLE ( 'NONE', #21437, 20.00000000000000711 ) ;
#22004 = ORIENTED_EDGE ( 'NONE', *, *, #25856, .T. ) ;
#22005 = ORIENTED_EDGE ( 'NONE', *, *, #35245, .T. ) ;
#22006 = CARTESIAN_POINT ( 'NONE',  ( -36.94073759706868287, -112.0000000000000142, 4.128524454178449155 ) ) ;
#22007 = AXIS2_PLACEMENT_3D ( 'NONE', #2110, #21503, #18285 ) ;
#22008 = DIRECTION ( 'NONE',  ( -1.000000000000000000, 0.000000000000000000, 0.000000000000000000 ) ) ;
#22009 = EDGE_LOOP ( 'NONE', ( #12198, #23341, #25110, #733 ) ) ;
#22010 = ORIENTED_EDGE ( 'NONE', *, *, #35414, .T. ) ;
#22011 = CARTESIAN_POINT ( 'NONE',  ( -34.50000000000000000, -112.1859307030124739, 1.448610958621386224 ) ) ;
#22012 = CARTESIAN_POINT ( 'NONE',  ( 0.000000000000000000, 9.471478019455140895, 14.71414642875960332 ) ) ;
#22013 = EDGE_CURVE ( 'NONE', #26535, #26887, #32094, .T. ) ;
#22014 = EDGE_CURVE ( 'NONE', #33987, #8021, #11300, .T. ) ;
#22015 = EDGE_CURVE ( 'NONE', #20308, #14939, #32802, .T. ) ;
#22016 = PRODUCT_DEFINITION_CONTEXT ( 'detailed design', #16306, 'design' ) ;
#22017 = CYLINDRICAL_SURFACE ( 'NONE', #27558, 4.799999999999998934 ) ;
#22018 = CYLINDRICAL_SURFACE ( 'NONE', #7050, 7.199999999999993960 ) ;
#22019 = CIRCLE ( 'NONE', #34704, 17.49900000000001299 ) ;
#22020 = CIRCLE ( 'NONE', #25499, 7.199999999999992184 ) ;
#22021 = CARTESIAN_POINT ( 'NONE',  ( -35.50000000000000000, -113.9929510916434339, 10.50625754673586876 ) ) ;
#22022 = CARTESIAN_POINT ( 'NONE',  ( 37.99999999999999289, 10.58300524425836997, -3.000000000000002665 ) ) ;
#22023 = DIRECTION ( 'NONE',  ( 0.000000000000000000, 0.7705132427757904745, -0.6374239897486881912 ) ) ;
#22024 = EDGE_CURVE ( 'NONE', #16053, #5260, #25668, .T. ) ;
#22025 = CARTESIAN_POINT ( 'NONE',  ( -34.50000000000000000, -111.0278007905855588, 1.116632271043183078 ) ) ;
#22026 = EDGE_CURVE ( 'NONE', #22477, #31803, #10485, .T. ) ;
#22027 = CARTESIAN_POINT ( 'NONE',  ( -37.59808119975203766, -115.9929510916434481, 14.11551573851449071 ) ) ;
#22028 = DIRECTION ( 'NONE',  ( 0.000000000000000000, 0.000000000000000000, -1.000000000000000000 ) ) ;
#22030 = VECTOR ( 'NONE', #13546, 1000.000000000000000 ) ;
#22029 = CARTESIAN_POINT ( 'NONE',  ( 8.000000000000000000, -17.56975900509186062, 9.555290079479195953 ) ) ;
#22031 = AXIS2_PLACEMENT_3D ( 'NONE', #33066, #19190, #467 ) ;
#22032 = FACE_OUTER_BOUND ( 'NONE', #170, .T. ) ;
#22033 = VERTEX_POINT ( 'NONE', #21089 ) ;
#22034 = CARTESIAN_POINT ( 'NONE',  ( -35.50000000000000711, -114.1189822439768449, 9.514224058074130852 ) ) ;
#22035 = DIRECTION ( 'NONE',  ( -1.000000000000000000, 0.000000000000000000, 0.000000000000000000 ) ) ;
#22036 = CARTESIAN_POINT ( 'NONE',  ( 0.000000000000000000, -51.85248208264515313, -3.914090171286743747 ) ) ;
#22037 = FACE_OUTER_BOUND ( 'NONE', #4459, .T. ) ;
#22038 = CYLINDRICAL_SURFACE ( 'NONE', #29176, 52.00000000000000711 ) ;
#22039 = ORIENTED_EDGE ( 'NONE', *, *, #10968, .T. ) ;
#22040 = CARTESIAN_POINT ( 'NONE',  ( -3.799999999999999822, 0.000000000000000000, -49.10000000000000142 ) ) ;
#22041 = DIRECTION ( 'NONE',  ( -1.000000000000000000, 0.000000000000000000, 0.000000000000000000 ) ) ;
#22042 = DIRECTION ( 'NONE',  ( 0.000000000000000000, 0.000000000000000000, -1.000000000000000000 ) ) ;
#22043 = FACE_OUTER_BOUND ( 'NONE', #14937, .T. ) ;
#22044 = ITEM_DEFINED_TRANSFORMATION ( 'NONE', 'NONE', #19579,  #21307 ) ;
#22045 = DIRECTION ( 'NONE',  ( 0.000000000000000000, 0.000000000000000000, 1.000000000000000000 ) ) ;
#22046 = CARTESIAN_POINT ( 'NONE',  ( 8.000000000000000000, 4.460989585140964664, 16.92083251265327348 ) ) ;
#22047 = ADVANCED_FACE ( 'NONE', ( #7423 ), #27231, .T. ) ;
#22048 = AXIS2_PLACEMENT_3D ( 'NONE', #512, #12205, #28067 ) ;
#22049 = ORIENTED_EDGE ( 'NONE', *, *, #27833, .F. ) ;
#22050 = CARTESIAN_POINT ( 'NONE',  ( -42.49999999999999289, -24.48076211353328802, 98.91941090707499029 ) ) ;
#22051 = ADVANCED_FACE ( 'NONE', ( #24348, #24527 ), #16210, .T. ) ;
#22052 = CARTESIAN_POINT ( 'NONE',  ( 7.999999999999992895, -0.2227391519119825691, 46.98410307550729215 ) ) ;
#22053 = EDGE_LOOP ( 'NONE', ( #15261, #34340, #27099, #24680 ) ) ;
#22054 = CARTESIAN_POINT ( 'NONE',  ( -37.74901162816868805, -113.3347980657955958, 7.933975545821553510 ) ) ;
#22055 = EDGE_LOOP ( 'NONE', ( #21139, #27856, #31311, #6360 ) ) ;
#22056 = EDGE_CURVE ( 'NONE', #17845, #24505, #32443, .T. ) ;
#22057 = SHAPE_REPRESENTATION_RELATIONSHIP ( 'NONE' , 'NONE' ,  #27563, #9091 ) ;
#22058 = ORIENTED_EDGE ( 'NONE', *, *, #24272, .T. ) ;
#22059 = ORIENTED_EDGE ( 'NONE', *, *, #14560, .F. ) ;
#22060 = FACE_OUTER_BOUND ( 'NONE', #7694, .T. ) ;
#22061 = AXIS2_PLACEMENT_3D ( 'NONE', #23426, #29202, #15119 ) ;
#22062 = AXIS2_PLACEMENT_3D ( 'NONE', #636, #20406, #1354 ) ;
#22063 = ADVANCED_FACE ( 'NONE', ( #7950 ), #5440, .T. ) ;
#22064 = DIRECTION ( 'NONE',  ( 1.000000000000000000, 0.000000000000000000, 0.000000000000000000 ) ) ;
#22065 = CIRCLE ( 'NONE', #10062, 11.00000000000000000 ) ;
#22066 = CARTESIAN_POINT ( 'NONE',  ( 50.00000000000000000, 20.00000000000001776, 120.0000000000000000 ) ) ;
#22067 = DIRECTION ( 'NONE',  ( -1.000000000000000000, 0.000000000000000000, 0.000000000000000000 ) ) ;
#22068 = DIRECTION ( 'NONE',  ( -1.000000000000000000, -0.000000000000000000, -0.000000000000000000 ) ) ;
#22069 = EDGE_CURVE ( 'NONE', #22471, #30312, #16393, .T. ) ;
#22070 = AXIS2_PLACEMENT_3D ( 'NONE', #20996, #15766, #26609 ) ;
#22071 = CARTESIAN_POINT ( 'NONE',  ( 7.999999999999992895, 19.74581912682842244, 48.10512059033400334 ) ) ;
#22072 = LINE ( 'NONE', #10748, #5845 ) ;
#22073 = CARTESIAN_POINT ( 'NONE',  ( 7.999999999999992895, -22.82995208772657492, -41.06517797613687293 ) ) ;
#22074 = CARTESIAN_POINT ( 'NONE',  ( -39.00000206272865455, -115.9929510916434481, 12.61164896875035879 ) ) ;
#22075 = DIRECTION ( 'NONE',  ( -1.000000000000000000, 0.000000000000000000, 0.000000000000000000 ) ) ;
#22076 = PLANE ( 'NONE',  #30306 ) ;
#22077 = DIRECTION ( 'NONE',  ( -1.000000000000000000, 0.000000000000000000, 0.000000000000000000 ) ) ;
#22078 = DIRECTION ( 'NONE',  ( 0.000000000000000000, 0.000000000000000000, -1.000000000000000000 ) ) ;
#22079 = AXIS2_PLACEMENT_3D ( 'NONE', #13161, #15641, #24136 ) ;
#22080 = LINE ( 'NONE', #16493, #6128 ) ;
#22081 = ORIENTED_EDGE ( 'NONE', *, *, #15496, .T. ) ;
#22082 = CARTESIAN_POINT ( 'NONE',  ( -35.02454729103298803, -113.1123104723225197, 6.902725545821550845 ) ) ;
#22083 = DIRECTION ( 'NONE',  ( -1.000000000000000000, 0.000000000000000000, 0.000000000000000000 ) ) ;
#22084 = CARTESIAN_POINT ( 'NONE',  ( 7.999999999999992895, -5.871425383721907920, 51.66745943012281117 ) ) ;
#22085 = DIRECTION ( 'NONE',  ( -1.000000000000000000, 1.110223024625156540E-16, 0.000000000000000000 ) ) ;
#22086 = EDGE_CURVE ( 'NONE', #9715, #2578, #30977, .T. ) ;
#22087 = VERTEX_POINT ( 'NONE', #30626 ) ;
#22088 = ORIENTED_EDGE ( 'NONE', *, *, #14940, .T. ) ;
#22089 = EDGE_CURVE ( 'NONE', #17290, #3282, #10708, .T. ) ;
#22090 = CARTESIAN_POINT ( 'NONE',  ( 65.00000000000001421, -27.93100416606583636, 81.50764321173598148 ) ) ;
#22091 = CARTESIAN_POINT ( 'NONE',  ( 0.000000000000000000, -19.83898331853678343, -9.508666619816859011 ) ) ;
#22092 = ORIENTED_EDGE ( 'NONE', *, *, #14474, .F. ) ;
#22093 = ORIENTED_EDGE ( 'NONE', *, *, #14550, .F. ) ;
#22094 = CARTESIAN_POINT ( 'NONE',  ( -46.00000000000000000, 0.000000000000000000, 0.000000000000000000 ) ) ;
#22095 = LINE ( 'NONE', #25171, #26344 ) ;
#22096 = EDGE_CURVE ( 'NONE', #1657, #17643, #2118, .T. ) ;
#22097 = EDGE_CURVE ( 'NONE', #1656, #8278, #17101, .T. ) ;
#22098 = DIRECTION ( 'NONE',  ( 0.000000000000000000, 0.000000000000000000, 1.000000000000000000 ) ) ;
#22099 = ORIENTED_EDGE ( 'NONE', *, *, #27941, .T. ) ;
#22100 = ORIENTED_EDGE ( 'NONE', *, *, #23726, .T. ) ;
#22101 =( REPRESENTATION_RELATIONSHIP ('NONE','NONE', #26607, #2005 ) REPRESENTATION_RELATIONSHIP_WITH_TRANSFORMATION ( #9215 )SHAPE_REPRESENTATION_RELATIONSHIP( ) );
#22102 = CIRCLE ( 'NONE', #35364, 4.000000000000000000 ) ;
#22103 = AXIS2_PLACEMENT_3D ( 'NONE', #9687, #20818, #22824 ) ;
#22104 = DIRECTION ( 'NONE',  ( 1.000000000000000000, 0.000000000000000000, -0.000000000000000000 ) ) ;
#22105 = CYLINDRICAL_SURFACE ( 'NONE', #22980, 22.00000000000000000 ) ;
#22106 = ORIENTED_EDGE ( 'NONE', *, *, #32345, .T. ) ;
#22107 = DIRECTION ( 'NONE',  ( -1.000000000000000000, -0.000000000000000000, 0.000000000000000000 ) ) ;
#22108 = AXIS2_PLACEMENT_3D ( 'NONE', #12035, #11673, #22641 ) ;
#22109 = CARTESIAN_POINT ( 'NONE',  ( -34.50000000000000000, -114.8057644833805568, -1.624782352598427959 ) ) ;
#22110 = CARTESIAN_POINT ( 'NONE',  ( -39.00000000000000711, -114.9929510916434339, 12.59652202191340820 ) ) ;
#22111 = CARTESIAN_POINT ( 'NONE',  ( -38.00000000000000711, -114.9929510916434339, 11.73841344789285657 ) ) ;
#22112 = CARTESIAN_POINT ( 'NONE',  ( 8.000000000000000000, -18.62763138773848581, -2.494040418455559127 ) ) ;
#22113 = CARTESIAN_POINT ( 'NONE',  ( -35.95093014754292682, -114.9929510916434339, 14.11777216781842448 ) ) ;
#22114 = CARTESIAN_POINT ( 'NONE',  ( 8.000000000000000000, 0.000000000000000000, 0.000000000000000000 ) ) ;
#22115 = DIRECTION ( 'NONE',  ( -1.000000000000000000, 0.000000000000000000, 0.000000000000000000 ) ) ;
#22116 = PLANE ( 'NONE',  #22126 ) ;
#22117 = DIRECTION ( 'NONE',  ( 1.000000000000000000, 0.000000000000000000, 0.000000000000000000 ) ) ;
#22118 = FACE_OUTER_BOUND ( 'NONE', #20694, .T. ) ;
#22119 = ORIENTED_EDGE ( 'NONE', *, *, #22902, .F. ) ;
#22120 = DIRECTION ( 'NONE',  ( 0.000000000000000000, 1.000000000000000000, 3.497202527569241525E-15 ) ) ;
#22121 = ORIENTED_EDGE ( 'NONE', *, *, #33878, .F. ) ;
#22122 = CARTESIAN_POINT ( 'NONE',  ( -34.02454729103298092, -115.3019030900506294, 3.097274454178448710 ) ) ;
#22123 = LINE ( 'NONE', #32766, #30747 ) ;
#22124 = ORIENTED_EDGE ( 'NONE', *, *, #30556, .T. ) ;
#22125 = ORIENTED_EDGE ( 'NONE', *, *, #3827, .F. ) ;
#22126 = AXIS2_PLACEMENT_3D ( 'NONE', #331, #3898, #33114 ) ;
#22127 = EDGE_CURVE ( 'NONE', #15307, #21532, #27400, .T. ) ;
#22128 = DIRECTION ( 'NONE',  ( 0.000000000000000000, 0.5877852522924743583, -0.8090169943749466741 ) ) ;
#22129 = AXIS2_PLACEMENT_3D ( 'NONE', #120, #22078, #292 ) ;
#22130 = CARTESIAN_POINT ( 'NONE',  ( 8.000000000000000000, 12.49559743815781587, 9.169462670380628566 ) ) ;
#22131 = ORIENTED_EDGE ( 'NONE', *, *, #4691, .T. ) ;
#22132 = CARTESIAN_POINT ( 'NONE',  ( -39.16322519054178741, -111.9205845034225177, 3.433975545821550845 ) ) ;
#22133 = MANIFOLD_SOLID_BREP ( 'LPattern2', #34219 ) ;
#22134 = VECTOR ( 'NONE', #18670, 1000.000000000000000 ) ;
#22135 = AXIS2_PLACEMENT_3D ( 'NONE', #32653, #7977, #18959 ) ;
#22136 = DIRECTION ( 'NONE',  ( 0.000000000000000000, 1.000000000000000000, 0.000000000000000000 ) ) ;
#22137 = DIRECTION ( 'NONE',  ( -1.000000000000000000, 0.000000000000000000, 0.000000000000000000 ) ) ;
#22138 = ORIENTED_EDGE ( 'NONE', *, *, #28611, .T. ) ;
#22139 = EDGE_LOOP ( 'NONE', ( #14586, #10091, #8715, #28442 ) ) ;
#22140 = CARTESIAN_POINT ( 'NONE',  ( -9.999999999999994671, 0.000000000000000000, 0.000000000000000000 ) ) ;
#22141 = SURFACE_STYLE_USAGE ( .BOTH. , #16566 ) ;
#22142 = LINE ( 'NONE', #19447, #20760 ) ;
#22144 = ORIENTED_EDGE ( 'NONE', *, *, #11261, .T. ) ;
#22143 = VECTOR ( 'NONE', #27927, 1000.000000000000000 ) ;
#22145 = ORIENTED_EDGE ( 'NONE', *, *, #9496, .F. ) ;
#22146 = CARTESIAN_POINT ( 'NONE',  ( -34.50000000000000000, -116.7615919857705080, -1.632210089000343700 ) ) ;
#22147 = DIRECTION ( 'NONE',  ( -1.000000000000000000, 0.000000000000000000, 0.000000000000000000 ) ) ;
#22148 = EDGE_LOOP ( 'NONE', ( #20696, #12318, #3568, #2238 ) ) ;
#22149 = CARTESIAN_POINT ( 'NONE',  ( -35.93473953453761283, -114.9929510916434339, 13.11451721564123574 ) ) ;
#22150 = CARTESIAN_POINT ( 'NONE',  ( -35.07817881376918479, -113.9929510916434339, 13.81802396319203474 ) ) ;
#22151 = VECTOR ( 'NONE', #16842, 1000.000000000000114 ) ;
#22152 = DIRECTION ( 'NONE',  ( 0.000000000000000000, -0.8443279255020201823, 0.5358267949789887741 ) ) ;
#22153 = DIRECTION ( 'NONE',  ( -1.000000000000000000, 0.000000000000000000, 0.000000000000000000 ) ) ;
#22154 = CARTESIAN_POINT ( 'NONE',  ( -34.50000000000000000, -113.9929510916434339, 10.50625754673586876 ) ) ;
#22155 = CARTESIAN_POINT ( 'NONE',  ( -39.00000000000000711, -114.9929510916434339, 11.91443571948719615 ) ) ;
#22156 = AXIS2_PLACEMENT_3D ( 'NONE', #9651, #10002, #29280 ) ;
#22157 = CARTESIAN_POINT ( 'NONE',  ( -35.50000000000000711, -114.9927795562974069, 10.48735431211914815 ) ) ;
#22158 = SURFACE_STYLE_USAGE ( .BOTH. , #14403 ) ;
#22159 = DIRECTION ( 'NONE',  ( -1.000000000000000000, 0.000000000000000000, 0.000000000000000000 ) ) ;
#22160 = ORIENTED_EDGE ( 'NONE', *, *, #12085, .F. ) ;
#22161 = ORIENTED_EDGE ( 'NONE', *, *, #21435, .T. ) ;
#22162 = FACE_OUTER_BOUND ( 'NONE', #29165, .T. ) ;
#22163 = LINE ( 'NONE', #25239, #35290 ) ;
#22164 = CIRCLE ( 'NONE', #6644, 47.49900000000002365 ) ;
#22165 = VERTEX_POINT ( 'NONE', #14232 ) ;
#22166 = CARTESIAN_POINT ( 'NONE',  ( 7.999999999999992895, 0.000000000000000000, 52.00000000000000711 ) ) ;
#22167 = ORIENTED_EDGE ( 'NONE', *, *, #1421, .F. ) ;
#22168 = EDGE_CURVE ( 'NONE', #23898, #31607, #4984, .T. ) ;
#22169 = CARTESIAN_POINT ( 'NONE',  ( -35.50000000000000711, -115.1446187476384040, -1.616767172155725740 ) ) ;
#22170 = DIRECTION ( 'NONE',  ( -0.9914448613738104932, -0.1305261922200510738, 1.844340778863525675E-31 ) ) ;
#22171 = CARTESIAN_POINT ( 'NONE',  ( -36.94073759706868287, -112.0000000000000142, 4.128524454178449155 ) ) ;
#22172 = DIRECTION ( 'NONE',  ( 1.000000000000000000, 0.000000000000000000, 0.000000000000000000 ) ) ;
#22173 = ORIENTED_EDGE ( 'NONE', *, *, #26434, .F. ) ;
#22174 = AXIS2_PLACEMENT_3D ( 'NONE', #21148, #31780, #20958 ) ;
#22175 = CARTESIAN_POINT ( 'NONE',  ( -35.50000000000000711, -112.3465879560236687, 1.629585756119413364 ) ) ;
#22176 = ORIENTED_EDGE ( 'NONE', *, *, #6885, .F. ) ;
#22177 = ORIENTED_EDGE ( 'NONE', *, *, #13008, .F. ) ;
#22178 = CARTESIAN_POINT ( 'NONE',  ( -36.94073759706868287, -112.0000000000000142, 8.628524454178448266 ) ) ;
#22179 = EDGE_CURVE ( 'NONE', #10915, #20895, #25096, .T. ) ;
#22180 = AXIS2_PLACEMENT_3D ( 'NONE', #15245, #1236, #9331 ) ;
#22181 = LINE ( 'NONE', #19996, #9522 ) ;
#22182 = ORIENTED_EDGE ( 'NONE', *, *, #33002, .T. ) ;
#22183 = ORIENTED_EDGE ( 'NONE', *, *, #2451, .F. ) ;
#22184 = CARTESIAN_POINT ( 'NONE',  ( -34.50000000000000000, -115.0140978167138712, 0.0002176474015577929428 ) ) ;
#22185 = AXIS2_PLACEMENT_3D ( 'NONE', #14153, #24804, #5713 ) ;
#22186 = LINE ( 'NONE', #28311, #5099 ) ;
#22187 = AXIS2_PLACEMENT_3D ( 'NONE', #24767, #8357, #2990 ) ;
#22188 = CARTESIAN_POINT ( 'NONE',  ( -36.99999999999999289, -12.47865190846804495, 110.2774766518096925 ) ) ;
#22189 = AXIS2_PLACEMENT_3D ( 'NONE', #12383, #6977, #24098 ) ;
#22190 = CARTESIAN_POINT ( 'NONE',  ( -35.50000000000000000, -113.9929510916434197, 10.50625754673586876 ) ) ;
#22191 = CARTESIAN_POINT ( 'NONE',  ( -42.49999999999999289, -41.45319397786874305, 92.20096189432314304 ) ) ;
#22192 = FACE_OUTER_BOUND ( 'NONE', #14112, .T. ) ;
#22193 = CARTESIAN_POINT ( 'NONE',  ( -34.50000000000000000, -112.8920926830253677, 2.874852253704053062 ) ) ;
#22194 = EDGE_CURVE ( 'NONE', #21017, #35346, #9572, .T. ) ;
#22195 = CARTESIAN_POINT ( 'NONE',  ( -39.00000000000000000, -115.9929510916434481, 11.73841344789285657 ) ) ;
#22196 = UNCERTAINTY_MEASURE_WITH_UNIT (LENGTH_MEASURE( 1.000000000000000082E-05 ), #10200, 'distance_accuracy_value', 'NONE');
#22197 = CARTESIAN_POINT ( 'NONE',  ( 7.999999999999992895, 0.000000000000000000, 0.000000000000000000 ) ) ;
#22198 = CARTESIAN_POINT ( 'NONE',  ( -46.00000000000000000, 0.000000000000000000, 0.000000000000000000 ) ) ;
#22199 = CIRCLE ( 'NONE', #21606, 4.872650870659778199 ) ;
#22200 = VERTEX_POINT ( 'NONE', #33156 ) ;
#22201 = CARTESIAN_POINT ( 'NONE',  ( -38.00000000000000711, -115.9929510916434481, 12.50851088611646311 ) ) ;
#22202 = CARTESIAN_POINT ( 'NONE',  ( 7.999999999999992895, 24.72041153920790180, -40.55929306992661765 ) ) ;
#22203 = DIRECTION ( 'NONE',  ( -1.000000000000000000, 0.000000000000000000, -0.000000000000000000 ) ) ;
#22204 = CARTESIAN_POINT ( 'NONE',  ( 1.599999999999990319, 0.000000000000000000, 0.000000000000000000 ) ) ;
#22205 = ORIENTED_EDGE ( 'NONE', *, *, #1777, .F. ) ;
#22206 = CIRCLE ( 'NONE', #14167, 1.000000000000000888 ) ;
#22207 = DIRECTION ( 'NONE',  ( 0.000000000000000000, 0.000000000000000000, 1.000000000000000000 ) ) ;
#22208 = FACE_OUTER_BOUND ( 'NONE', #2122, .T. ) ;
#22209 = ADVANCED_FACE ( 'NONE', ( #8485 ), #5792, .T. ) ;
#22210 = DIRECTION ( 'NONE',  ( -0.000000000000000000, 0.000000000000000000, -1.000000000000000000 ) ) ;
#22211 = DIRECTION ( 'NONE',  ( -1.000000000000000000, 0.000000000000000000, 0.000000000000000000 ) ) ;
#22212 = EDGE_CURVE ( 'NONE', #34767, #31708, #11369, .T. ) ;
#22213 = ADVANCED_FACE ( 'NONE', ( #8653 ), #19620, .T. ) ;
#22214 = VECTOR ( 'NONE', #220, 1000.000000000000000 ) ;
#22215 = DIRECTION ( 'NONE',  ( 1.000000000000000000, -0.000000000000000000, -0.000000000000000000 ) ) ;
#22216 = DIRECTION ( 'NONE',  ( 0.000000000000000000, 0.000000000000000000, -1.000000000000000000 ) ) ;
#22217 = VECTOR ( 'NONE', #30718, 1000.000000000000000 ) ;
#22218 = ORIENTED_EDGE ( 'NONE', *, *, #9049, .F. ) ;
#22219 = CARTESIAN_POINT ( 'NONE',  ( -46.00000000000000000, -25.98076211353320275, 84.99999999999992895 ) ) ;
#22220 = CARTESIAN_POINT ( 'NONE',  ( -9.999999999999994671, 0.000000000000000000, 0.000000000000000000 ) ) ;
#22221 = DIRECTION ( 'NONE',  ( 0.000000000000000000, 0.000000000000000000, 1.000000000000000000 ) ) ;
#22222 = ORIENTED_EDGE ( 'NONE', *, *, #27797, .T. ) ;
#22223 = CARTESIAN_POINT ( 'NONE',  ( -36.02454729103297382, -113.5265240346956261, 5.402725545821552622 ) ) ;
#22224 = EDGE_CURVE ( 'NONE', #11512, #9304, #3263, .T. ) ;
#22225 = VERTEX_POINT ( 'NONE', #19969 ) ;
#22226 = ADVANCED_FACE ( 'NONE', ( #20515 ), #31333, .T. ) ;
#22227 =( NAMED_UNIT ( * ) PLANE_ANGLE_UNIT ( ) SI_UNIT ( $, .RADIAN. ) );
#22228 = AXIS2_PLACEMENT_3D ( 'NONE', #9851, #24096, #26612 ) ;
#22229 = ORIENTED_EDGE ( 'NONE', *, *, #29293, .F. ) ;
#22230 = ORIENTED_EDGE ( 'NONE', *, *, #9123, .T. ) ;
#22231 = CARTESIAN_POINT ( 'NONE',  ( -34.49999999999998579, -39.90017302060827831, 83.49999999999991473 ) ) ;
#22232 = CIRCLE ( 'NONE', #2144, 3.800000000000018918 ) ;
#22233 = CARTESIAN_POINT ( 'NONE',  ( -35.50000000000000711, -112.0140978167138712, 0.7189676474015718188 ) ) ;
#22234 = VECTOR ( 'NONE', #907, 1000.000000000000000 ) ;
#22235 = AXIS2_PLACEMENT_3D ( 'NONE', #27678, #13978, #19027 ) ;
#22236 = CARTESIAN_POINT ( 'NONE',  ( 7.999999999999992895, 3.872983346207531596, 1.000000000000000888 ) ) ;
#22237 = AXIS2_PLACEMENT_3D ( 'NONE', #26324, #3828, #29014 ) ;
#22238 = CARTESIAN_POINT ( 'NONE',  ( -35.50000000000000711, -114.0998638248492085, 9.511920366020609308 ) ) ;
#22239 = CARTESIAN_POINT ( 'NONE',  ( 50.00000000000000000, 20.00000000000001776, 120.0000000000000000 ) ) ;
#22240 = AXIS2_PLACEMENT_3D ( 'NONE', #27278, #2621, #35570 ) ;
#22241 = DIRECTION ( 'NONE',  ( -1.000000000000000000, -0.000000000000000000, -0.000000000000000000 ) ) ;
#22242 = ADVANCED_FACE ( 'NONE', ( #28814 ), #23224, .T. ) ;
#22243 = CARTESIAN_POINT ( 'NONE',  ( -34.50000000000000000, -114.9929510916434339, 12.26648026267477221 ) ) ;
#22244 = CARTESIAN_POINT ( 'NONE',  ( 7.999999999999992895, 46.87740477351717061, -3.172455868805379442 ) ) ;
#22245 = DIRECTION ( 'NONE',  ( 0.000000000000000000, 0.000000000000000000, 1.000000000000000000 ) ) ;
#22246 = CARTESIAN_POINT ( 'NONE',  ( -37.42187499999996447, -115.9929510916434481, 14.11852480586265024 ) ) ;
#22247 = DIRECTION ( 'NONE',  ( 0.000000000000000000, -0.4817536741017223734, 0.8763066800438596982 ) ) ;
#22248 = MANIFOLD_SOLID_BREP ( 'Keyway', #8324 ) ;
#22249 = DIRECTION ( 'NONE',  ( 0.000000000000000000, 0.000000000000000000, -1.000000000000000000 ) ) ;
#22250 = CYLINDRICAL_SURFACE ( 'NONE', #17608, 0.7500000000000006661 ) ;
#22251 = DIRECTION ( 'NONE',  ( 1.000000000000000000, -0.000000000000000000, 0.000000000000000000 ) ) ;
#22252 = CIRCLE ( 'NONE', #9020, 22.00000000000000000 ) ;
#22253 = ADVANCED_FACE ( 'NONE', ( #9187 ), #6842, .T. ) ;
#22254 = DIRECTION ( 'NONE',  ( -1.734723475976807094E-16, 1.000000000000000000, 0.000000000000000000 ) ) ;
#22255 = ORIENTED_EDGE ( 'NONE', *, *, #24145, .T. ) ;
#22256 = EDGE_CURVE ( 'NONE', #12175, #15307, #15310, .T. ) ;
#22257 = ADVANCED_FACE ( 'NONE', ( #15106 ), #26115, .T. ) ;
#22258 = CARTESIAN_POINT ( 'NONE',  ( -37.05926240293131713, -112.0000000000000142, 6.621475545821550845 ) ) ;
#22259 = CIRCLE ( 'NONE', #6740, 3.799999999999999822 ) ;
#22260 = CARTESIAN_POINT ( 'NONE',  ( 0.000000000000000000, -30.03615769709705319, -42.44795908869020451 ) ) ;
#22261 = CARTESIAN_POINT ( 'NONE',  ( 65.00000000000001421, -28.31857036507964764, 80.03062855292515110 ) ) ;
#22262 = AXIS2_PLACEMENT_3D ( 'NONE', #33035, #11420, #29813 ) ;
#22263 = CARTESIAN_POINT ( 'NONE',  ( -34.49999999999998579, -26.38406014851792847, 79.52301627764165914 ) ) ;
#22264 = EDGE_LOOP ( 'NONE', ( #31167, #15715 ) ) ;
#22265 = ORIENTED_EDGE ( 'NONE', *, *, #3104, .T. ) ;
#22266 = DIRECTION ( 'NONE',  ( -1.000000000000000000, 0.000000000000000000, 0.000000000000000000 ) ) ;
#22267 = LINE ( 'NONE', #33263, #30741 ) ;
#22268 = ORIENTED_EDGE ( 'NONE', *, *, #31892, .T. ) ;
#22269 = VECTOR ( 'NONE', #27113, 1000.000000000000000 ) ;
#22270 = ORIENTED_EDGE ( 'NONE', *, *, #12015, .F. ) ;
#22271 = EDGE_CURVE ( 'NONE', #30700, #32761, #1445, .T. ) ;
#22272 = FACE_OUTER_BOUND ( 'NONE', #23840, .T. ) ;
#22273 = CARTESIAN_POINT ( 'NONE',  ( 8.000000000000000000, -16.59870953437678409, -3.253005020244019718 ) ) ;
#22274 = CARTESIAN_POINT ( 'NONE',  ( -40.40000000000001279, -1.387778780781445676E-14, 110.0000000000000000 ) ) ;
#22275 = DIRECTION ( 'NONE',  ( 0.000000000000000000, 0.000000000000000000, 1.000000000000000000 ) ) ;
#22276 = ORIENTED_EDGE ( 'NONE', *, *, #5319, .F. ) ;
#22277 = ORIENTED_EDGE ( 'NONE', *, *, #25198, .T. ) ;
#22278 = VECTOR ( 'NONE', #32349, 1000.000000000000000 ) ;
#22279 = DIRECTION ( 'NONE',  ( 0.000000000000000000, 0.000000000000000000, 1.000000000000000000 ) ) ;
#22280 = DIRECTION ( 'NONE',  ( -1.000000000000000000, 0.000000000000000000, 0.000000000000000000 ) ) ;
#22281 = EDGE_LOOP ( 'NONE', ( #18058, #18862, #11161, #29956 ) ) ;
#22282 = LINE ( 'NONE', #25357, #20083 ) ;
#22283 = AXIS2_PLACEMENT_3D ( 'NONE', #28970, #3779, #23020 ) ;
#22284 = ADVANCED_FACE ( 'NONE', ( #14573 ), #23411, .T. ) ;
#22285 = CARTESIAN_POINT ( 'NONE',  ( -34.50000000000000000, -115.8137639216009234, -1.239329810084483841 ) ) ;
#22286 = AXIS2_PLACEMENT_3D ( 'NONE', #30563, #27340, #13827 ) ;
#22287 = CARTESIAN_POINT ( 'NONE',  ( -36.01562499999996447, -114.9929510916434339, 14.11852480586264846 ) ) ;
#22288 = EDGE_CURVE ( 'NONE', #17787, #21924, #17627, .T. ) ;
#22289 = CARTESIAN_POINT ( 'NONE',  ( -35.50000000000000000, -113.9929510916434339, 10.51175824272318415 ) ) ;
#22290 = CARTESIAN_POINT ( 'NONE',  ( 7.999999999999992895, 0.000000000000000000, 0.000000000000000000 ) ) ;
#22291 = CARTESIAN_POINT ( 'NONE',  ( -34.51922597003733273, -114.9929510916434339, 12.86289566494349224 ) ) ;
#22292 = FACE_OUTER_BOUND ( 'NONE', #23969, .T. ) ;
#22293 = CIRCLE ( 'NONE', #457, 4.000000000000000000 ) ;
#22294 = CARTESIAN_POINT ( 'NONE',  ( -42.49999999999999289, -27.48076211353305354, 71.08058909292485339 ) ) ;
#22295 = CARTESIAN_POINT ( 'NONE',  ( 0.000000000000000000, 5.871425383722286284, -51.66745943012276854 ) ) ;
#22296 = CARTESIAN_POINT ( 'NONE',  ( -12.55910585664919132, 0.7408941433508802188, -8.474091755303837753E-30 ) ) ;
#22297 = CARTESIAN_POINT ( 'NONE',  ( -3.799999999999999822, 4.653657836759942730E-16, 35.10000000000000142 ) ) ;
#22298 = ORIENTED_EDGE ( 'NONE', *, *, #20292, .T. ) ;
#22299 = LINE ( 'NONE', #19751, #8939 ) ;
#22300 = ORIENTED_EDGE ( 'NONE', *, *, #788, .F. ) ;
#22301 = EDGE_CURVE ( 'NONE', #9489, #16062, #4338, .T. ) ;
#22302 = CARTESIAN_POINT ( 'NONE',  ( -34.92058450342251064, -116.1632251905417945, 6.191024454178448266 ) ) ;
#22303 = EDGE_CURVE ( 'NONE', #16934, #15970, #1634, .T. ) ;
#22304 = DIRECTION ( 'NONE',  ( 0.000000000000000000, 0.000000000000000000, 1.000000000000000000 ) ) ;
#22305 = CARTESIAN_POINT ( 'NONE',  ( -35.50000000000000711, -114.1807644833817648, -1.624782352598427959 ) ) ;
#22306 = ORIENTED_EDGE ( 'NONE', *, *, #29084, .T. ) ;
#22307 = ORIENTED_EDGE ( 'NONE', *, *, #21765, .T. ) ;
#22308 = DIRECTION ( 'NONE',  ( -0.000000000000000000, 0.000000000000000000, -1.000000000000000000 ) ) ;
#22309 = CARTESIAN_POINT ( 'NONE',  ( 0.000000000000000000, -2.710505431213761085E-17, -45.00000000000000000 ) ) ;
#22310 = CIRCLE ( 'NONE', #15978, 17.49900000000001654 ) ;
#22311 = ORIENTED_EDGE ( 'NONE', *, *, #26677, .F. ) ;
#22312 = VECTOR ( 'NONE', #35363, 1000.000000000000000 ) ;
#22313 = LINE ( 'NONE', #33306, #12673 ) ;
#22314 = CARTESIAN_POINT ( 'NONE',  ( -1.479000000000008086, 0.000000000000000000, 0.000000000000000000 ) ) ;
#22315 = ORIENTED_EDGE ( 'NONE', *, *, #5799, .F. ) ;
#22316 = VERTEX_POINT ( 'NONE', #11886 ) ;
#22317 = CARTESIAN_POINT ( 'NONE',  ( -39.49999999999999289, -12.79398423610758684, 91.86693750936007064 ) ) ;
#22318 = CIRCLE ( 'NONE', #26954, 8.000000000000000000 ) ;
#22319 = SHAPE_REPRESENTATION_RELATIONSHIP ( 'NONE' , 'NONE' ,  #33742, #39 ) ;
#22320 = DIRECTION ( 'NONE',  ( -1.000000000000000000, 0.000000000000000000, 0.000000000000000000 ) ) ;
#22321 = EDGE_LOOP ( 'NONE', ( #3032, #10487 ) ) ;
#22322 = ORIENTED_EDGE ( 'NONE', *, *, #23985, .T. ) ;
#22323 = CARTESIAN_POINT ( 'NONE',  ( -34.50000000000000000, -117.0140978167138854, -0.1247823525984438492 ) ) ;
#22324 = ORIENTED_EDGE ( 'NONE', *, *, #16722, .T. ) ;
#22325 = CARTESIAN_POINT ( 'NONE',  ( -35.99181955245763476, -114.9929510916434339, 13.11847460610632687 ) ) ;
#22326 = ADVANCED_FACE ( 'NONE', ( #17639 ), #22864, .T. ) ;
#22327 = ADVANCED_FACE ( 'NONE', ( #34950 ), #23955, .T. ) ;
#22328 = CARTESIAN_POINT ( 'NONE',  ( -34.50000000000000000, -113.9929510916434339, 10.61627146648203990 ) ) ;
#22329 = FACE_OUTER_BOUND ( 'NONE', #11739, .T. ) ;
#22330 = CARTESIAN_POINT ( 'NONE',  ( 8.000000000000000000, 0.000000000000000000, 0.000000000000000000 ) ) ;
#22331 = CARTESIAN_POINT ( 'NONE',  ( -34.50000000000000000, -113.9929510916434339, 12.57451923796416260 ) ) ;
#22332 = DIRECTION ( 'NONE',  ( 0.000000000000000000, 0.000000000000000000, -1.000000000000000000 ) ) ;
#22333 = CIRCLE ( 'NONE', #10280, 4.000000000000000000 ) ;
#22334 = CARTESIAN_POINT ( 'NONE',  ( -35.50000000000000711, -114.8847986568751907, 10.03799953695244618 ) ) ;
#22335 = CARTESIAN_POINT ( 'NONE',  ( 4.000000000000003553, 49.25004636492413823, -16.68630974939705425 ) ) ;
#22336 = AXIS2_PLACEMENT_3D ( 'NONE', #1704, #18069, #29067 ) ;
#22337 = CARTESIAN_POINT ( 'NONE',  ( 7.999999999999992895, 9.744342220504046637, -46.48873837489789196 ) ) ;
#22338 = VERTEX_POINT ( 'NONE', #32754 ) ;
#22339 = ORIENTED_EDGE ( 'NONE', *, *, #24717, .T. ) ;
#22340 = FACE_OUTER_BOUND ( 'NONE', #14374, .T. ) ;
#22341 = DIRECTION ( 'NONE',  ( 0.000000000000000000, 0.000000000000000000, -1.000000000000000000 ) ) ;
#22342 = ORIENTED_EDGE ( 'NONE', *, *, #32265, .F. ) ;
#22343 = DIRECTION ( 'NONE',  ( 1.000000000000000000, -5.339440136655842133E-16, -1.047965281155519420E-16 ) ) ;
#22344 = ORIENTED_EDGE ( 'NONE', *, *, #230, .F. ) ;
#22345 = CARTESIAN_POINT ( 'NONE',  ( -35.50000000000000000, -115.0304602784513293, -0.6247823525985405357 ) ) ;
#22346 = CARTESIAN_POINT ( 'NONE',  ( 0.000000000000000000, -29.60891106212763191, -37.14118181634798788 ) ) ;
#22347 = CARTESIAN_POINT ( 'NONE',  ( -38.97545270896704039, -113.1123104723225197, 3.847274454178449599 ) ) ;
#22348 = CARTESIAN_POINT ( 'NONE',  ( -50.00000000000000000, 0.000000000000000000, 0.000000000000000000 ) ) ;
#22349 = ORIENTED_EDGE ( 'NONE', *, *, #11021, .T. ) ;
#22350 = CARTESIAN_POINT ( 'NONE',  ( 8.000000000000000000, -10.62435788049451624, 13.16139124467916588 ) ) ;
#22351 = CARTESIAN_POINT ( 'NONE',  ( -35.50000000000000711, -112.0140978167138712, 0.8127176474015721519 ) ) ;
#22352 = EDGE_LOOP ( 'NONE', ( #2423, #8991, #12317, #6960, #7426, #35525, #23975 ) ) ;
#22353 = ORIENTED_EDGE ( 'NONE', *, *, #33936, .F. ) ;
#22354 = CARTESIAN_POINT ( 'NONE',  ( 8.000000000000000000, 16.92083251265325572, 4.460989585141031277 ) ) ;
#22355 = VECTOR ( 'NONE', #11779, 1000.000000000000000 ) ;
#22356 = DIRECTION ( 'NONE',  ( 1.000000000000000000, -0.000000000000000000, -0.000000000000000000 ) ) ;
#22357 = ORIENTED_EDGE ( 'NONE', *, *, #7549, .F. ) ;
#22358 = VERTEX_POINT ( 'NONE', #26835 ) ;
#22359 = AXIS2_PLACEMENT_3D ( 'NONE', #28144, #948, #8686 ) ;
#22360 = CARTESIAN_POINT ( 'NONE',  ( -34.50000000000000000, -112.0140978167138712, 0.8127176474015721519 ) ) ;
#22361 = DIRECTION ( 'NONE',  ( 1.000000000000000000, -0.000000000000000000, -0.000000000000000000 ) ) ;
#22362 = ORIENTED_EDGE ( 'NONE', *, *, #10722, .T. ) ;
#22363 = PRODUCT_DEFINITION_CONTEXT ( 'detailed design', #8498, 'design' ) ;
#22364 = DIRECTION ( 'NONE',  ( -1.000000000000000000, 0.000000000000000000, 0.000000000000000000 ) ) ;
#22365 = MANIFOLD_SOLID_BREP ( 'Sweep3', #23278 ) ;
#22366 = EDGE_CURVE ( 'NONE', #34373, #14462, #17031, .T. ) ;
#22367 = CARTESIAN_POINT ( 'NONE',  ( -35.50000000000000000, -113.9929510916434339, 12.39849696637031684 ) ) ;
#22368 = CARTESIAN_POINT ( 'NONE',  ( 3.799999999999999822, 4.382607293638566128E-16, -46.00000000000000000 ) ) ;
#22369 = LINE ( 'NONE', #33899, #21660 ) ;
#22370 = CARTESIAN_POINT ( 'NONE',  ( -34.50000000000000000, -113.1451905347060460, 2.905063584339864668 ) ) ;
#22371 = CARTESIAN_POINT ( 'NONE',  ( -39.00000000000000000, -115.9929510916434481, 12.53051367006571937 ) ) ;
#22372 = DIRECTION ( 'NONE',  ( 0.000000000000000000, 0.000000000000000000, -1.000000000000000000 ) ) ;
#22373 = DIRECTION ( 'NONE',  ( -1.000000000000000000, -0.000000000000000000, -0.000000000000000000 ) ) ;
#22374 = ORIENTED_EDGE ( 'NONE', *, *, #27132, .T. ) ;
#22375 = CIRCLE ( 'NONE', #32164, 4.000000000000006217 ) ;
#22376 = EDGE_CURVE ( 'NONE', #11426, #24050, #13907, .T. ) ;
#22377 = DIRECTION ( 'NONE',  ( 1.000000000000000000, 0.000000000000000000, 0.000000000000000000 ) ) ;
#22378 = DIRECTION ( 'NONE',  ( -1.000000000000000000, -0.000000000000000000, 0.000000000000000000 ) ) ;
#22379 = DIRECTION ( 'NONE',  ( 0.000000000000000000, 0.000000000000000000, 1.000000000000000000 ) ) ;
#22380 = ORIENTED_EDGE ( 'NONE', *, *, #7347, .F. ) ;
#22381 = CIRCLE ( 'NONE', #4608, 4.800000000000006928 ) ;
#22382 = CARTESIAN_POINT ( 'NONE',  ( 8.000000000000000000, 11.19999565274265230, -10.71350075272062874 ) ) ;
#22383 = FACE_OUTER_BOUND ( 'NONE', #27900, .T. ) ;
#22384 = FACE_OUTER_BOUND ( 'NONE', #27850, .T. ) ;
#22385 = CARTESIAN_POINT ( 'NONE',  ( 0.000000000000000000, -50.95304419620817526, -10.38206564895716255 ) ) ;
#22386 = CONTEXT_DEPENDENT_SHAPE_REPRESENTATION ( #21161, #14658 ) ;
#22387 = CIRCLE ( 'NONE', #24140, 52.00000000000000711 ) ;
#22388 = AXIS2_PLACEMENT_3D ( 'NONE', #12593, #3605, #26995 ) ;
#22389 = FACE_OUTER_BOUND ( 'NONE', #26729, .T. ) ;
#22390 = CARTESIAN_POINT ( 'NONE',  ( 65.00000000000001421, -37.13120097615721704, 79.35042362907756797 ) ) ;
#22391 = ORIENTED_EDGE ( 'NONE', *, *, #25863, .T. ) ;
#22392 = DIRECTION ( 'NONE',  ( 0.000000000000000000, 0.000000000000000000, 1.000000000000000000 ) ) ;
#22393 = CARTESIAN_POINT ( 'NONE',  ( -42.49999999999999289, -25.98076211353322051, 84.99999999999992895 ) ) ;
#22394 = DIRECTION ( 'NONE',  ( 0.000000000000000000, 0.000000000000000000, 1.000000000000000000 ) ) ;
#22395 = EDGE_LOOP ( 'NONE', ( #30650, #17677, #30111, #27855 ) ) ;
#22396 = CARTESIAN_POINT ( 'NONE',  ( -37.97545270896702618, -114.4734759653044023, 3.152725545821551734 ) ) ;
#22397 = ORIENTED_EDGE ( 'NONE', *, *, #22096, .F. ) ;
#22398 = SURFACE_STYLE_FILL_AREA ( #25121 ) ;
#22399 = ORIENTED_EDGE ( 'NONE', *, *, #3178, .F. ) ;
#22400 = ORIENTED_EDGE ( 'NONE', *, *, #13439, .T. ) ;
#22401 = DIRECTION ( 'NONE',  ( 0.000000000000000000, 0.000000000000000000, -1.000000000000000000 ) ) ;
#22402 = CARTESIAN_POINT ( 'NONE',  ( -35.50000000000000711, -116.0140896356112989, -0.6575071456984549201 ) ) ;
#22403 = CARTESIAN_POINT ( 'NONE',  ( 8.000000000000000000, 8.128228055639098670, -16.94522934049206242 ) ) ;
#22404 = AXIS2_PLACEMENT_3D ( 'NONE', #8081, #19422, #22115 ) ;
#22405 = ADVANCED_FACE ( 'NONE', ( #7387 ), #35301, .T. ) ;
#22406 = CARTESIAN_POINT ( 'NONE',  ( -35.50000000000000711, -114.1152303497977414, 9.513755561829650986 ) ) ;
#22407 = DIRECTION ( 'NONE',  ( -0.000000000000000000, 0.000000000000000000, -1.000000000000000000 ) ) ;
#22408 = ADVANCED_FACE ( 'NONE', ( #27192 ), #5054, .T. ) ;
#22409 = COLOUR_RGB ( '', 0.31764706, 0.68627451, 0.89019608) ;
#22410 = ORIENTED_EDGE ( 'NONE', *, *, #17694, .T. ) ;
#22411 = FACE_OUTER_BOUND ( 'NONE', #21011, .T. ) ;
#22412 = AXIS2_PLACEMENT_3D ( 'NONE', #22452, #25180, #11137 ) ;
#22413 = LINE ( 'NONE', #8559, #30897 ) ;
#22414 = DIRECTION ( 'NONE',  ( -1.000000000000000000, 0.000000000000000000, -0.000000000000000000 ) ) ;
#22415 = FACE_OUTER_BOUND ( 'NONE', #14764, .T. ) ;
#22416 = EDGE_CURVE ( 'NONE', #24291, #21688, #4734, .T. ) ;
#22417 = CARTESIAN_POINT ( 'NONE',  ( -35.50000000000000000, -114.2253558743059330, 8.519800927820798009 ) ) ;
#22418 = CARTESIAN_POINT ( 'NONE',  ( -35.50000000000000711, -112.0157046079661995, -0.6902086197697556713 ) ) ;
#22419 = CARTESIAN_POINT ( 'NONE',  ( 3.872983346207489852, 0.9999999999999522604, 45.00000000000000711 ) ) ;
#22420 = DIRECTION ( 'NONE',  ( 1.000000000000000000, -5.339440136655842133E-16, -1.047965281155519420E-16 ) ) ;
#22421 = DIRECTION ( 'NONE',  ( 0.000000000000000000, 0.8660254037844410391, -0.4999999999999958367 ) ) ;
#22422 = DIRECTION ( 'NONE',  ( -1.000000000000000000, 0.000000000000000000, 0.000000000000000000 ) ) ;
#22423 = CARTESIAN_POINT ( 'NONE',  ( 0.000000000000000000, 0.000000000000000000, 0.000000000000000000 ) ) ;
#22424 = ORIENTED_EDGE ( 'NONE', *, *, #30642, .T. ) ;
#22425 = CIRCLE ( 'NONE', #4064, 4.800000000000000711 ) ;
#22426 = CARTESIAN_POINT ( 'NONE',  ( -37.05926240293131713, -112.0000000000000142, 8.121475545821549957 ) ) ;
#22427 = CARTESIAN_POINT ( 'NONE',  ( -1.566204647097432900, -6.822536405429440620, -0.7999999999999951594 ) ) ;
#22428 = LINE ( 'NONE', #22600, #20465 ) ;
#22429 = CARTESIAN_POINT ( 'NONE',  ( 30.00000000000000000, 1.359357947053562196E-14, 0.000000000000000000 ) ) ;
#22430 = EDGE_LOOP ( 'NONE', ( #792, #30828, #12595, #33305 ) ) ;
#22431 = AXIS2_PLACEMENT_3D ( 'NONE', #21191, #34361, #24097 ) ;
#22432 = ORIENTED_EDGE ( 'NONE', *, *, #33440, .F. ) ;
#22433 = CARTESIAN_POINT ( 'NONE',  ( 8.000000000000000000, -12.96676809804157848, 13.60411018104313641 ) ) ;
#22434 = CARTESIAN_POINT ( 'NONE',  ( 8.000000000000007105, -0.3151488735046864553, -11.27190672109269798 ) ) ;
#22435 = ORIENTED_EDGE ( 'NONE', *, *, #14296, .F. ) ;
#22436 = ORIENTED_EDGE ( 'NONE', *, *, #18138, .T. ) ;
#22437 = VECTOR ( 'NONE', #9999, 1000.000000000000000 ) ;
#22438 = CIRCLE ( 'NONE', #28188, 14.00000000000000000 ) ;
#22439 = AXIS2_PLACEMENT_3D ( 'NONE', #26511, #12454, #31711 ) ;
#22440 = EDGE_CURVE ( 'NONE', #1552, #31085, #9305, .T. ) ;
#22441 = FACE_OUTER_BOUND ( 'NONE', #20479, .T. ) ;
#22442 = DIRECTION ( 'NONE',  ( 1.000000000000000000, -0.000000000000000000, 0.000000000000000000 ) ) ;
#22443 = APPLICATION_PROTOCOL_DEFINITION ( 'draft international standard', 'automotive_design', 1998, #10554 ) ;
#22444 = DIRECTION ( 'NONE',  ( 0.000000000000000000, 0.8660254037844398178, -0.4999999999999978906 ) ) ;
#22445 = ORIENTED_EDGE ( 'NONE', *, *, #5805, .T. ) ;
#22446 = ORIENTED_EDGE ( 'NONE', *, *, #2954, .F. ) ;
#22447 = EDGE_CURVE ( 'NONE', #2304, #7406, #5313, .T. ) ;
#22448 = DIRECTION ( 'NONE',  ( 0.000000000000000000, 0.000000000000000000, 1.000000000000000000 ) ) ;
#22449 = EDGE_CURVE ( 'NONE', #15607, #27203, #7907, .T. ) ;
#22450 = CIRCLE ( 'NONE', #20726, 2.999999999999988898 ) ;
#22451 = EDGE_CURVE ( 'NONE', #33603, #21198, #7651, .T. ) ;
#22452 = CARTESIAN_POINT ( 'NONE',  ( 7.999999999999992895, 0.000000000000000000, 0.000000000000000000 ) ) ;
#22453 = ORIENTED_EDGE ( 'NONE', *, *, #17655, .F. ) ;
#22454 = CARTESIAN_POINT ( 'NONE',  ( 5.400000000000085620, -1.000000000000049516, 55.00000000000000711 ) ) ;
#22455 = CARTESIAN_POINT ( 'NONE',  ( -34.50000000000000000, -112.9977353549762000, -0.6247823525983134951 ) ) ;
#22456 = DIRECTION ( 'NONE',  ( 0.000000000000000000, 0.000000000000000000, -1.000000000000000000 ) ) ;
#22457 = DIRECTION ( 'NONE',  ( 1.032573497605238773E-16, -6.938893903907203726E-17, -1.000000000000000000 ) ) ;
#22458 = CARTESIAN_POINT ( 'NONE',  ( -34.50000000000000000, -114.2114213871176958, 8.518137620934190579 ) ) ;
#22459 = FACE_OUTER_BOUND ( 'NONE', #17172, .T. ) ;
#22460 = DIRECTION ( 'NONE',  ( 0.000000000000000000, -0.6845471059286794002, -0.7289686274214203232 ) ) ;
#22461 = EDGE_CURVE ( 'NONE', #8976, #35528, #22526, .T. ) ;
#22462 = AXIS2_PLACEMENT_3D ( 'NONE', #18943, #10675, #21634 ) ;
#22463 = CARTESIAN_POINT ( 'NONE',  ( -37.24999999999992895, -114.9929510916434339, 14.11852480586264846 ) ) ;
#22465 = CARTESIAN_POINT ( 'NONE',  ( 4.000000000000003553, -9.637487275700962641, -10.15474465512058977 ) ) ;
#22464 = AXIS2_PLACEMENT_3D ( 'NONE', #24155, #7936, #2020 ) ;
#22466 = ADVANCED_FACE ( 'NONE', ( #12789 ), #4533, .T. ) ;
#22467 = DIRECTION ( 'NONE',  ( 1.836970198721029934E-16, -1.000000000000000000, 0.000000000000000000 ) ) ;
#22468 =( GEOMETRIC_REPRESENTATION_CONTEXT ( 3 ) GLOBAL_UNCERTAINTY_ASSIGNED_CONTEXT ( ( #8771 ) ) GLOBAL_UNIT_ASSIGNED_CONTEXT ( ( #6997, #28795, #14739 ) ) REPRESENTATION_CONTEXT ( 'NONE', 'WORKASPACE' ) );
#22469 = DIRECTION ( 'NONE',  ( 0.1305261922200477154, 0.9914448613738109373, 2.653430841701508438E-16 ) ) ;
#22470 = DIRECTION ( 'NONE',  ( -1.000000000000000000, 0.000000000000000000, -0.000000000000000000 ) ) ;
#22471 = VERTEX_POINT ( 'NONE', #5403 ) ;
#22472 = CARTESIAN_POINT ( 'NONE',  ( -38.00000000000000711, -114.9929510916434339, 11.91443571948719615 ) ) ;
#22473 = ORIENTED_EDGE ( 'NONE', *, *, #20937, .T. ) ;
#22474 = CARTESIAN_POINT ( 'NONE',  ( -34.92058450342251064, -116.1632251905417945, 4.691024454178447378 ) ) ;
#22475 = DIRECTION ( 'NONE',  ( -1.047965281155519667E-16, -6.938893903907193865E-17, -1.000000000000000000 ) ) ;
#22476 = CARTESIAN_POINT ( 'NONE',  ( -35.50000000000000711, -114.8474311500471572, -1.624782352598427959 ) ) ;
#22477 = VERTEX_POINT ( 'NONE', #21940 ) ;
#22478 = VERTEX_POINT ( 'NONE', #22774 ) ;
#22479 = CARTESIAN_POINT ( 'NONE',  ( 7.999999999999992895, -13.85708833599938217, -45.43276465116679930 ) ) ;
#22480 = DIRECTION ( 'NONE',  ( -1.174092375852890260E-15, 4.222049128630259891E-16, 1.000000000000000000 ) ) ;
#22481 = VERTEX_POINT ( 'NONE', #1188 ) ;
#22482 = MANIFOLD_SOLID_BREP ( 'LPattern5', #25620 ) ;
#22483 = ADVANCED_FACE ( 'NONE', ( #17367 ), #6049, .F. ) ;
#22484 = FACE_OUTER_BOUND ( 'NONE', #22645, .T. ) ;
#22485 = FACE_OUTER_BOUND ( 'NONE', #29643, .T. ) ;
#22486 = ORIENTED_EDGE ( 'NONE', *, *, #1087, .F. ) ;
#22488 = ORIENTED_EDGE ( 'NONE', *, *, #14000, .T. ) ;
#22487 = EDGE_CURVE ( 'NONE', #21017, #32022, #25677, .T. ) ;
#22489 = DIRECTION ( 'NONE',  ( 0.000000000000000000, -0.9848077530122063550, -0.1736481776669404342 ) ) ;
#22491 = EDGE_CURVE ( 'NONE', #31548, #10765, #22955, .T. ) ;
#22490 = VECTOR ( 'NONE', #12806, 1000.000000000000000 ) ;
#22492 = VECTOR ( 'NONE', #32737, 1000.000000000000000 ) ;
#22493 = DIRECTION ( 'NONE',  ( 0.000000000000000000, 9.406921877466749789E-15, -1.000000000000000000 ) ) ;
#22494 = ORIENTED_EDGE ( 'NONE', *, *, #30609, .F. ) ;
#22495 = ORIENTED_EDGE ( 'NONE', *, *, #30244, .T. ) ;
#22496 = CARTESIAN_POINT ( 'NONE',  ( -34.50000000000000000, -116.2431927316855109, -2.224114562372550008 ) ) ;
#22497 = EDGE_CURVE ( 'NONE', #32738, #25838, #32388, .T. ) ;
#22498 = ORIENTED_EDGE ( 'NONE', *, *, #32106, .T. ) ;
#22499 = EDGE_CURVE ( 'NONE', #29247, #24192, #17011, .T. ) ;
#22500 = CARTESIAN_POINT ( 'NONE',  ( -35.60016694755736921, -114.9929510916434339, 12.92579853460621209 ) ) ;
#22501 = CARTESIAN_POINT ( 'NONE',  ( -34.50000000000000000, -114.1712995509219724, 9.522174004479579068 ) ) ;
#22502 = CARTESIAN_POINT ( 'NONE',  ( -55.00000000000000000, -25.98076211353320275, 84.99999999999994316 ) ) ;
#22503 = DIRECTION ( 'NONE',  ( 1.000000000000000000, -5.339440136655842133E-16, -1.047965281155519420E-16 ) ) ;
#22504 = CARTESIAN_POINT ( 'NONE',  ( -34.50000000000000000, -113.9929510916434339, 11.38636890470581164 ) ) ;
#22505 = EDGE_CURVE ( 'NONE', #34240, #8132, #23178, .T. ) ;
#22506 = CARTESIAN_POINT ( 'NONE',  ( -38.00000000000000711, -115.9929510916434481, 12.26648026267477221 ) ) ;
#22507 = DIRECTION ( 'NONE',  ( -1.000000000000000000, 0.000000000000000000, 0.000000000000000000 ) ) ;
#22508 = DIRECTION ( 'NONE',  ( 0.000000000000000000, 0.7535859266250380939, 0.6573494133204066392 ) ) ;
#22509 = ORIENTED_EDGE ( 'NONE', *, *, #17193, .T. ) ;
#22510 = ORIENTED_EDGE ( 'NONE', *, *, #20118, .T. ) ;
#22511 = AXIS2_PLACEMENT_3D ( 'NONE', #8472, #33143, #27046 ) ;
#22512 = COLOUR_RGB ( '', 0.40784314, 0.44705882, 0.49803922) ;
#22513 = CARTESIAN_POINT ( 'NONE',  ( 8.000000000000007105, 9.604183132802424083, -5.908880290975567995 ) ) ;
#22514 = CIRCLE ( 'NONE', #6996, 20.00000000000000355 ) ;
#22515 = DIRECTION ( 'NONE',  ( 0.000000000000000000, 1.000000000000000000, 0.000000000000000000 ) ) ;
#22516 = ORIENTED_EDGE ( 'NONE', *, *, #14477, .T. ) ;
#22517 = DIRECTION ( 'NONE',  ( 1.000000000000000000, 0.000000000000000000, 0.000000000000000000 ) ) ;
#22518 = ORIENTED_EDGE ( 'NONE', *, *, #11259, .T. ) ;
#22519 = CARTESIAN_POINT ( 'NONE',  ( -35.50000000000000000, -113.0140978167139991, -0.6247823525984269599 ) ) ;
#22520 = DIRECTION ( 'NONE',  ( -1.000000000000000000, 0.000000000000000000, 0.000000000000000000 ) ) ;
#22521 = CARTESIAN_POINT ( 'NONE',  ( -36.23083527818512550, -116.0245472910329880, 3.284774454178449155 ) ) ;
#22522 = ORIENTED_EDGE ( 'NONE', *, *, #5182, .T. ) ;
#22523 = CARTESIAN_POINT ( 'NONE',  ( -39.49999999999999289, -3.734562119078910225, 144.3977620171895637 ) ) ;
#22524 = EDGE_CURVE ( 'NONE', #4315, #9203, #8256, .T. ) ;
#22525 = EDGE_LOOP ( 'NONE', ( #7414, #10916, #8198, #19285 ) ) ;
#22526 = CIRCLE ( 'NONE', #33456, 3.799999999999999822 ) ;
#22527 = ADVANCED_FACE ( 'NONE', ( #20236 ), #14486, .T. ) ;
#22528 = CYLINDRICAL_SURFACE ( 'NONE', #25678, 4.000000000000003553 ) ;
#22529 = CARTESIAN_POINT ( 'NONE',  ( -35.50000000000000711, -112.6043641208289188, 1.789429170677330649 ) ) ;
#22530 = VERTEX_POINT ( 'NONE', #25496 ) ;
#22531 = VERTEX_POINT ( 'NONE', #14315 ) ;
#22532 = CARTESIAN_POINT ( 'NONE',  ( -44.00000000000000000, 10.58300524425835398, -3.000000000000002665 ) ) ;
#22533 = DIRECTION ( 'NONE',  ( 0.000000000000000000, 0.000000000000000000, 1.000000000000000000 ) ) ;
#22534 = ORIENTED_EDGE ( 'NONE', *, *, #1867, .T. ) ;
#22535 = ORIENTED_EDGE ( 'NONE', *, *, #29962, .T. ) ;
#22536 = CARTESIAN_POINT ( 'NONE',  ( -34.50000000000000000, -115.0140978167138712, 0.3752176474015737617 ) ) ;
#22537 = LINE ( 'NONE', #8858, #30378 ) ;
#22538 = ADVANCED_FACE ( 'NONE', ( #6227 ), #5863, .T. ) ;
#22539 = ORIENTED_EDGE ( 'NONE', *, *, #6558, .F. ) ;
#22540 = AXIS2_PLACEMENT_3D ( 'NONE', #30532, #14129, #5514 ) ;
#22541 = ORIENTED_EDGE ( 'NONE', *, *, #10206, .F. ) ;
#22542 = FACE_OUTER_BOUND ( 'NONE', #20474, .T. ) ;
#22543 = MANIFOLD_SOLID_BREP ( 'Cut-Extrude-Thin1', #22711 ) ;
#22544 = CARTESIAN_POINT ( 'NONE',  ( -35.50000000000000000, -113.9929510916434339, 10.50625754673586876 ) ) ;
#22545 = FACE_OUTER_BOUND ( 'NONE', #8345, .T. ) ;
#22546 = DIRECTION ( 'NONE',  ( 0.000000000000000000, 0.000000000000000000, 1.000000000000000000 ) ) ;
#22547 = CARTESIAN_POINT ( 'NONE',  ( -34.50000000000000000, -116.0140978167138712, 0.8752176474015622709 ) ) ;
#22548 = CARTESIAN_POINT ( 'NONE',  ( -38.98077402996267438, -115.9929510916434481, 12.86289566494346204 ) ) ;
#22549 = CYLINDRICAL_SURFACE ( 'NONE', #11267, 20.00000000000000355 ) ;
#22550 = CIRCLE ( 'NONE', #6443, 52.00000000000000711 ) ;
#22551 = CARTESIAN_POINT ( 'NONE',  ( 8.000000000000000000, -8.128228055638727412, -16.94522934049221519 ) ) ;
#22552 = CYLINDRICAL_SURFACE ( 'NONE', #18839, 3.799999999999999822 ) ;
#22553 = DIRECTION ( 'NONE',  ( -1.000000000000000000, 0.000000000000000000, -0.000000000000000000 ) ) ;
#22554 = DIRECTION ( 'NONE',  ( 9.615983791445651082E-17, -6.938893903907203726E-17, -1.000000000000000000 ) ) ;
#22555 = ORIENTED_EDGE ( 'NONE', *, *, #31805, .T. ) ;
#22556 = CARTESIAN_POINT ( 'NONE',  ( 50.00000000000000000, -25.98076211353320275, 73.99999999999992895 ) ) ;
#22557 = DIRECTION ( 'NONE',  ( 0.000000000000000000, -0.3420201433256758738, 0.9396926207859057634 ) ) ;
#22558 = AXIS2_PLACEMENT_3D ( 'NONE', #20184, #26151, #20727 ) ;
#22559 = DIRECTION ( 'NONE',  ( 0.000000000000000000, 1.000000000000000000, 9.406921877466749789E-15 ) ) ;
#22560 = LINE ( 'NONE', #433, #29943 ) ;
#22561 = ITEM_DEFINED_TRANSFORMATION ( 'NONE', 'NONE', #1208,  #21307 ) ;
#22562 = AXIS2_PLACEMENT_3D ( 'NONE', #30134, #8328, #28098 ) ;
#22563 = DIRECTION ( 'NONE',  ( 1.000000000000000000, -0.000000000000000000, -0.000000000000000000 ) ) ;
#22564 = CARTESIAN_POINT ( 'NONE',  ( 0.000000000000000000, 16.94522934049215124, 8.128228055638924587 ) ) ;
#22565 = EDGE_LOOP ( 'NONE', ( #27492, #31926, #27429, #7020 ) ) ;
#22566 = EDGE_CURVE ( 'NONE', #31574, #13189, #30584, .T. ) ;
#22567 = DIRECTION ( 'NONE',  ( 0.000000000000000000, 0.7705132427757903635, -0.6374239897486881912 ) ) ;
#22568 = DIRECTION ( 'NONE',  ( -0.000000000000000000, 0.000000000000000000, -1.000000000000000000 ) ) ;
#22569 = CYLINDRICAL_SURFACE ( 'NONE', #3064, 20.00000000000000355 ) ;
#22570 = ORIENTED_EDGE ( 'NONE', *, *, #3164, .F. ) ;
#22571 = CARTESIAN_POINT ( 'NONE',  ( -36.64504884055821776, -112.9754527089670688, 3.715225545821552178 ) ) ;
#22572 = VERTEX_POINT ( 'NONE', #29081 ) ;
#22574 = VERTEX_POINT ( 'NONE', #12881 ) ;
#22573 = AXIS2_PLACEMENT_3D ( 'NONE', #23822, #26348, #1681 ) ;
#22575 = ORIENTED_EDGE ( 'NONE', *, *, #22524, .F. ) ;
#22576 = CARTESIAN_POINT ( 'NONE',  ( 65.00000000000001421, 58.35354061212520804, 76.25822877525452270 ) ) ;
#22577 = AXIS2_PLACEMENT_3D ( 'NONE', #9067, #20023, #22918 ) ;
#22578 = CARTESIAN_POINT ( 'NONE',  ( -35.50000000000000711, -114.6807644833805000, -1.624782352598427959 ) ) ;
#22579 = CARTESIAN_POINT ( 'NONE',  ( 8.000000000000000000, 5.400000000000021672, 1.000000000000001776 ) ) ;
#22580 = VECTOR ( 'NONE', #12665, 1000.000000000000000 ) ;
#22581 = CARTESIAN_POINT ( 'NONE',  ( -35.50000000000000711, -114.9929501463477663, 10.50247632894551231 ) ) ;
#22582 = VECTOR ( 'NONE', #6837, 1000.000000000000000 ) ;
#22583 = CARTESIAN_POINT ( 'NONE',  ( 0.3000000000000016542, -14.69693845669907439, -1.200000000000006617 ) ) ;
#22584 = CARTESIAN_POINT ( 'NONE',  ( 0.2000000000000057288, -6.997142273814354496, -0.7999999999999951594 ) ) ;
#22585 = CARTESIAN_POINT ( 'NONE',  ( -34.50000000000000000, -114.4026847875275337, 9.592046023459676718 ) ) ;
#22586 = CARTESIAN_POINT ( 'NONE',  ( 4.000000000000003553, 15.17386234660384581, 15.92965478239621824 ) ) ;
#22587 = FACE_OUTER_BOUND ( 'NONE', #23448, .T. ) ;
#22588 = CARTESIAN_POINT ( 'NONE',  ( -35.50000000000000000, -115.9929510916434481, 10.68227981832981044 ) ) ;
#22589 = DIRECTION ( 'NONE',  ( -1.000000000000000000, 0.000000000000000000, 0.000000000000000000 ) ) ;
#22590 = MANIFOLD_SOLID_BREP ( 'InnerRace', #14657 ) ;
#22591 = CARTESIAN_POINT ( 'NONE',  ( 3.799999999999999822, -2.710505431213761085E-17, 29.09999999999999787 ) ) ;
#22592 = AXIS2_PLACEMENT_3D ( 'NONE', #9133, #14346, #33439 ) ;
#22593 = CARTESIAN_POINT ( 'NONE',  ( 7.999999999999992895, 0.000000000000000000, 0.000000000000000000 ) ) ;
#22594 = DIRECTION ( 'NONE',  ( -1.000000000000000000, 0.000000000000000000, 0.000000000000000000 ) ) ;
#22595 = DIRECTION ( 'NONE',  ( 0.000000000000000000, 0.9048270524660176894, 0.4257792915650767118 ) ) ;
#22596 = DIRECTION ( 'NONE',  ( 0.000000000000000000, 0.000000000000000000, 1.000000000000000000 ) ) ;
#22597 = VERTEX_POINT ( 'NONE', #15550 ) ;
#22598 = CARTESIAN_POINT ( 'NONE',  ( -38.99999999999999289, -114.0592624029313242, 7.746475545821551734 ) ) ;
#22599 = CARTESIAN_POINT ( 'NONE',  ( 0.000000000000000000, 14.30000000000000071, 0.000000000000000000 ) ) ;
#22600 = CARTESIAN_POINT ( 'NONE',  ( 4.000000000000000000, -7.317194182740013098, -18.61340026142654480 ) ) ;
#22601 = DIRECTION ( 'NONE',  ( 0.000000000000000000, 0.6427876096865403621, -0.7660444431189772363 ) ) ;
#22602 = ORIENTED_EDGE ( 'NONE', *, *, #8364, .T. ) ;
#22603 = ORIENTED_EDGE ( 'NONE', *, *, #28219, .T. ) ;
#22604 = VECTOR ( 'NONE', #31565, 1000.000000000000000 ) ;
#22605 = ADVANCED_FACE ( 'NONE', ( #1537 ), #17729, .T. ) ;
#22606 = DIRECTION ( 'NONE',  ( 0.000000000000000000, 0.000000000000000000, 1.000000000000000000 ) ) ;
#22607 = VECTOR ( 'NONE', #5571, 1000.000000000000000 ) ;
#22608 = CARTESIAN_POINT ( 'NONE',  ( 8.000000000000000000, -0.5097555531874721213, 19.99350267651955093 ) ) ;
#22609 = ORIENTED_EDGE ( 'NONE', *, *, #2684, .F. ) ;
#22610 = ADVANCED_FACE ( 'NONE', ( #34670 ), #7006, .T. ) ;
#22611 = ORIENTED_EDGE ( 'NONE', *, *, #15612, .T. ) ;
#22612 = CARTESIAN_POINT ( 'NONE',  ( -0.2000000000000612399, -6.997142273814382030, -0.7999999999999951594 ) ) ;
#22613 = FACE_OUTER_BOUND ( 'NONE', #9584, .T. ) ;
#22614 = EDGE_CURVE ( 'NONE', #32680, #21788, #20795, .T. ) ;
#22615 = CONTEXT_DEPENDENT_SHAPE_REPRESENTATION ( #11031, #26515 ) ;
#22616 = DIRECTION ( 'NONE',  ( 0.000000000000000000, -0.7535859266250379829, -0.6573494133204068612 ) ) ;
#22617 = VERTEX_POINT ( 'NONE', #20952 ) ;
#22618 = EDGE_LOOP ( 'NONE', ( #16116, #19647 ) ) ;
#22619 = DIRECTION ( 'NONE',  ( 1.000000000000000000, 0.000000000000000000, 0.000000000000000000 ) ) ;
#22620 = DIRECTION ( 'NONE',  ( 0.000000000000000000, 0.000000000000000000, -1.000000000000000000 ) ) ;
#22621 = EDGE_LOOP ( 'NONE', ( #28966, #10985, #32784, #21018 ) ) ;
#22622 = DIRECTION ( 'NONE',  ( 1.000000000000000000, -0.000000000000000000, 0.000000000000000000 ) ) ;
#22623 = CARTESIAN_POINT ( 'NONE',  ( -34.50000000000000000, -115.0140978167139707, -0.6091573525984161908 ) ) ;
#22624 = DIRECTION ( 'NONE',  ( 0.000000000000000000, 0.1253332335643045359, -0.9921147013144778759 ) ) ;
#22625 = DIRECTION ( 'NONE',  ( -1.000000000000000000, 0.000000000000000000, 0.000000000000000000 ) ) ;
#22626 = VECTOR ( 'NONE', #16012, 1000.000000000000000 ) ;
#22627 = CARTESIAN_POINT ( 'NONE',  ( -39.00000000000000711, -114.9929510916434339, 12.56351784598954779 ) ) ;
#22628 = AXIS2_PLACEMENT_3D ( 'NONE', #20059, #6749, #6562 ) ;
#22629 = FACE_OUTER_BOUND ( 'NONE', #32462, .T. ) ;
#22630 = DIRECTION ( 'NONE',  ( -1.000000000000000000, -0.000000000000000000, -0.000000000000000000 ) ) ;
#22631 = CARTESIAN_POINT ( 'NONE',  ( -34.50000000000000000, -114.3049001878960240, 8.530677542735578101 ) ) ;
#22632 = CARTESIAN_POINT ( 'NONE',  ( 7.999999999999992895, 42.60732521687570795, 19.80331771201672453 ) ) ;
#22633 = ADVANCED_FACE ( 'NONE', ( #31953 ), #18263, .T. ) ;
#22634 = CARTESIAN_POINT ( 'NONE',  ( 7.999999999999992895, 10.58300524425836109, 3.000000000000002665 ) ) ;
#22635 = DIRECTION ( 'NONE',  ( -1.000000000000000000, 0.000000000000000000, 0.000000000000000000 ) ) ;
#22636 = CARTESIAN_POINT ( 'NONE',  ( -36.49999999999999289, -11.24969279549607748, 111.5585998451919778 ) ) ;
#22637 = ORIENTED_EDGE ( 'NONE', *, *, #21330, .T. ) ;
#22638 = DIRECTION ( 'NONE',  ( 0.000000000000000000, 0.000000000000000000, 1.000000000000000000 ) ) ;
#22639 = ORIENTED_EDGE ( 'NONE', *, *, #431, .F. ) ;
#22640 = CARTESIAN_POINT ( 'NONE',  ( -39.16322519054179452, -116.0794154965774823, 5.066024454178449155 ) ) ;
#22641 = DIRECTION ( 'NONE',  ( 0.000000000000000000, 0.000000000000000000, 1.000000000000000000 ) ) ;
#22642 = CARTESIAN_POINT ( 'NONE',  ( -35.50000000000000711, -113.4307644833805000, -1.624782352598427959 ) ) ;
#22643 = ORIENTED_EDGE ( 'NONE', *, *, #6679, .T. ) ;
#22644 = AXIS2_PLACEMENT_3D ( 'NONE', #14274, #3322, #245 ) ;
#22645 = EDGE_LOOP ( 'NONE', ( #17091, #12516, #7470, #8468 ) ) ;
#22646 = EDGE_CURVE ( 'NONE', #11697, #32964, #4788, .T. ) ;
#22647 = CARTESIAN_POINT ( 'NONE',  ( 0.000000000000000000, -9.637487275701184686, 10.15474465512046542 ) ) ;
#22648 = CARTESIAN_POINT ( 'NONE',  ( -21.15833593587365513, -39.95319397786859383, 75.20096189432314304 ) ) ;
#22649 = EDGE_CURVE ( 'NONE', #15452, #11237, #34849, .T. ) ;
#22650 = EDGE_CURVE ( 'NONE', #18596, #34599, #32136, .T. ) ;
#22651 = ORIENTED_EDGE ( 'NONE', *, *, #19790, .T. ) ;
#22652 = MANIFOLD_SOLID_BREP ( 'Mirror1', #29050 ) ;
#22653 = AXIS2_PLACEMENT_3D ( 'NONE', #26988, #30039, #10770 ) ;
#22654 = CYLINDRICAL_SURFACE ( 'NONE', #34966, 4.000000000000003553 ) ;
#22655 = VECTOR ( 'NONE', #16002, 1000.000000000000000 ) ;
#22656 = ORIENTED_EDGE ( 'NONE', *, *, #19602, .F. ) ;
#22657 = ORIENTED_EDGE ( 'NONE', *, *, #28851, .T. ) ;
#22658 = CARTESIAN_POINT ( 'NONE',  ( -38.99999999999999289, -114.0592624029313242, 7.746475545821551734 ) ) ;
#22659 = EDGE_CURVE ( 'NONE', #19278, #5903, #2089, .T. ) ;
#22660 = EDGE_CURVE ( 'NONE', #10046, #22033, #22550, .T. ) ;
#22661 = AXIS2_PLACEMENT_3D ( 'NONE', #31299, #14721, #34187 ) ;
#22662 = FACE_OUTER_BOUND ( 'NONE', #33260, .T. ) ;
#22663 = EDGE_LOOP ( 'NONE', ( #13953, #9045, #7728, #58 ) ) ;
#22664 = VERTEX_POINT ( 'NONE', #2441 ) ;
#22665 = CARTESIAN_POINT ( 'NONE',  ( -35.50000000000000000, -111.0140978167138570, 0.8127176474015720409 ) ) ;
#22666 = CARTESIAN_POINT ( 'NONE',  ( 0.000000000000000000, -2.710505431213761085E-17, -46.00000000000000000 ) ) ;
#22667 = VERTEX_POINT ( 'NONE', #22036 ) ;
#22668 = CARTESIAN_POINT ( 'NONE',  ( -37.43749999999998579, -114.9929510916434339, 13.11852480586264669 ) ) ;
#22669 = CARTESIAN_POINT ( 'NONE',  ( -37.88878409051687157, -113.9929510916434339, 14.07058620477052280 ) ) ;
#22670 = CARTESIAN_POINT ( 'NONE',  ( 50.00000000000000000, 20.00000000000001776, 120.0000000000000000 ) ) ;
#22671 = DIRECTION ( 'NONE',  ( -1.000000000000000000, 0.000000000000000000, 0.000000000000000000 ) ) ;
#22672 = CARTESIAN_POINT ( 'NONE',  ( -35.90191880024782023, -113.9929510916434339, 14.11551573851449071 ) ) ;
#22673 = CARTESIAN_POINT ( 'NONE',  ( 0.000000000000000000, -5.667686777402029641, 46.64153600743602368 ) ) ;
#22674 = ADVANCED_FACE ( 'NONE', ( #16085, #32481 ), #5487, .F. ) ;
#22675 = CARTESIAN_POINT ( 'NONE',  ( -35.69272627125609176, -114.9929510916434339, 13.01835785830562209 ) ) ;
#22676 =( NAMED_UNIT ( * ) PLANE_ANGLE_UNIT ( ) SI_UNIT ( $, .RADIAN. ) );
#22678 = AXIS2_PLACEMENT_3D ( 'NONE', #20426, #23512, #20254 ) ;
#22677 = DIRECTION ( 'NONE',  ( 1.112002228190253556E-16, -6.938893903907203726E-17, -1.000000000000000000 ) ) ;
#22679 = FACE_OUTER_BOUND ( 'NONE', #19346, .T. ) ;
#22680 = VECTOR ( 'NONE', #11498, 1000.000000000000000 ) ;
#22681 = ORIENTED_EDGE ( 'NONE', *, *, #10871, .F. ) ;
#22682 = PRODUCT_DEFINITION ( 'UNKNOWN', '', #25884, #22363 ) ;
#22683 = ORIENTED_EDGE ( 'NONE', *, *, #16789, .F. ) ;
#22684 = EDGE_CURVE ( 'NONE', #30439, #31835, #2275, .T. ) ;
#22685 = CARTESIAN_POINT ( 'NONE',  ( 0.000000000000000000, -5.679790370316031733, 7.613867765417587030 ) ) ;
#22686 = CARTESIAN_POINT ( 'NONE',  ( 8.000000000000000000, 6.085920226791238008, -15.78165944574512203 ) ) ;
#22687 = AXIS2_PLACEMENT_3D ( 'NONE', #15249, #21008, #7353 ) ;
#22688 = ORIENTED_EDGE ( 'NONE', *, *, #5011, .T. ) ;
#22689 = FACE_OUTER_BOUND ( 'NONE', #34330, .T. ) ;
#22690 = ORIENTED_EDGE ( 'NONE', *, *, #13039, .F. ) ;
#22691 = CARTESIAN_POINT ( 'NONE',  ( -35.50000000000000000, -115.0140978167138712, -0.5622823525984408377 ) ) ;
#22692 = CARTESIAN_POINT ( 'NONE',  ( -34.49999999999998579, -28.31857036507959791, 80.03062855292519373 ) ) ;
#22693 = CARTESIAN_POINT ( 'NONE',  ( -35.54388159064475872, -112.6276912846090568, 5.816024454178449155 ) ) ;
#22694 = EDGE_CURVE ( 'NONE', #25236, #28380, #21966, .T. ) ;
#22695 = ADVANCED_FACE ( 'NONE', ( #24218 ), #35209, .T. ) ;
#22696 = ORIENTED_EDGE ( 'NONE', *, *, #14281, .F. ) ;
#22697 = CARTESIAN_POINT ( 'NONE',  ( -35.54388159064475872, -112.6276912846090568, 7.316024454178449155 ) ) ;
#22698 = CIRCLE ( 'NONE', #24448, 5.000000000000004441 ) ;
#22699 = VERTEX_POINT ( 'NONE', #2809 ) ;
#22700 = CARTESIAN_POINT ( 'NONE',  ( 0.000000000000000000, -16.92083251265322019, -4.460989585141143188 ) ) ;
#22701 = CARTESIAN_POINT ( 'NONE',  ( -35.50000000000000711, -112.1222502514821144, 1.343475657184566296 ) ) ;
#22702 = ORIENTED_EDGE ( 'NONE', *, *, #2260, .F. ) ;
#22703 = VERTEX_POINT ( 'NONE', #21676 ) ;
#22704 = CARTESIAN_POINT ( 'NONE',  ( -38.99999999999999289, -113.9407375970686900, 5.253524454178449155 ) ) ;
#22705 = EDGE_CURVE ( 'NONE', #12757, #2544, #10529, .T. ) ;
#22706 = CARTESIAN_POINT ( 'NONE',  ( 0.000000000000000000, -2.710505431213761085E-17, 45.10000000000000142 ) ) ;
#22707 = VERTEX_POINT ( 'NONE', #30150 ) ;
#22708 = EDGE_LOOP ( 'NONE', ( #9548, #5242, #26099, #18775 ) ) ;
#22709 = CARTESIAN_POINT ( 'NONE',  ( -34.50000000000000000, -115.0140978167138712, -0.4685323525984310122 ) ) ;
#22710 = LINE ( 'NONE', #9042, #29272 ) ;
#22711 = CLOSED_SHELL ( 'NONE', ( #30595, #30415, #30643, #2540, #31364, #22891, #17876, #10784, #27234, #4650, #32619, #9222, #22674, #13333, #5768, #32217, #4814, #29554, #13018, #18533, #23200, #26191, #6437, #12111, #26205, #871, #34891, #17803, #19522, #14546, #1170, #8747, #4740 ) ) ;
#22712 = PRODUCT_DEFINITION_SHAPE ( 'NONE', 'NONE',  #5129 ) ;
#22713 = AXIS2_PLACEMENT_3D ( 'NONE', #28372, #20416, #22959 ) ;
#22714 = ORIENTED_EDGE ( 'NONE', *, *, #35054, .F. ) ;
#22715 = PRODUCT_DEFINITION_CONTEXT ( 'detailed design', #16995, 'design' ) ;
#22716 = ORIENTED_EDGE ( 'NONE', *, *, #28565, .T. ) ;
#22717 = DIRECTION ( 'NONE',  ( 0.000000000000000000, 0.000000000000000000, 1.000000000000000000 ) ) ;
#22718 = MANIFOLD_SOLID_BREP ( 'Notch', #16383 ) ;
#22719 = CIRCLE ( 'NONE', #4377, 20.00000000000000000 ) ;
#22720 = VECTOR ( 'NONE', #25519, 1000.000000000000000 ) ;
#22721 = CARTESIAN_POINT ( 'NONE',  ( -36.15625000000007816, -113.9929510916434339, 13.11852480586264846 ) ) ;
#22722 = CARTESIAN_POINT ( 'NONE',  ( 0.000000000000000000, 30.03615769709734451, 42.44795908869000556 ) ) ;
#22723 = CARTESIAN_POINT ( 'NONE',  ( -42.49999999999999289, -21.76666049839542438, 84.29903810567665801 ) ) ;
#22724 = CARTESIAN_POINT ( 'NONE',  ( -34.50000000000000000, -111.0140978167138570, -0.1247823525984260717 ) ) ;
#22725 = EDGE_CURVE ( 'NONE', #25525, #6691, #9919, .T. ) ;
#22726 = CARTESIAN_POINT ( 'NONE',  ( -35.50640865667917723, -115.9929510916434481, 12.69998175888958691 ) ) ;
#22727 = CIRCLE ( 'NONE', #5509, 7.000000000000006217 ) ;
#22728 = CARTESIAN_POINT ( 'NONE',  ( 0.000000000000000000, 12.46108038583314936, 15.64357617739001860 ) ) ;
#22729 = EDGE_CURVE ( 'NONE', #30389, #25690, #2465, .T. ) ;
#22730 = FACE_OUTER_BOUND ( 'NONE', #2017, .T. ) ;
#22731 = EDGE_CURVE ( 'NONE', #23819, #4059, #7035, .T. ) ;
#22732 = CARTESIAN_POINT ( 'NONE',  ( -1.599999999999990319, 0.000000000000000000, 0.000000000000000000 ) ) ;
#22733 = DIRECTION ( 'NONE',  ( 0.000000000000000000, 0.000000000000000000, 1.000000000000000000 ) ) ;
#22734 = DIRECTION ( 'NONE',  ( 1.000000000000000000, -5.339440136655842133E-16, -1.047965281155519420E-16 ) ) ;
#22735 = EDGE_LOOP ( 'NONE', ( #26269, #14322, #21235, #20800 ) ) ;
#22736 = DIRECTION ( 'NONE',  ( -1.000000000000000000, 0.000000000000000000, 0.000000000000000000 ) ) ;
#22737 = FACE_OUTER_BOUND ( 'NONE', #10808, .T. ) ;
#22738 = CIRCLE ( 'NONE', #4371, 7.199999999999993072 ) ;
#22739 = DIRECTION ( 'NONE',  ( 1.000000000000000000, -0.000000000000000000, -0.000000000000000000 ) ) ;
#22740 = DIRECTION ( 'NONE',  ( -0.8432271980573221581, 4.787673685806302502E-16, -0.5375573387615479870 ) ) ;
#22741 = EDGE_CURVE ( 'NONE', #34512, #21171, #249, .T. ) ;
#22742 = EDGE_CURVE ( 'NONE', #52, #6257, #19660, .T. ) ;
#22743 = FACE_OUTER_BOUND ( 'NONE', #2233, .T. ) ;
#22744 = DIRECTION ( 'NONE',  ( 0.000000000000000000, -0.9980267284282708928, -0.06279051952932447611 ) ) ;
#22745 = VERTEX_POINT ( 'NONE', #19838 ) ;
#22746 = CIRCLE ( 'NONE', #7799, 20.00000000000001066 ) ;
#22747 = CARTESIAN_POINT ( 'NONE',  ( 7.999999999999992895, 0.000000000000000000, 0.000000000000000000 ) ) ;
#22748 = CARTESIAN_POINT ( 'NONE',  ( 8.000000000000000000, 18.48663108841359559, -3.384281271887881637 ) ) ;
#22749 = CARTESIAN_POINT ( 'NONE',  ( 7.999999999999992895, -5.667686777402029641, 46.64153600743602368 ) ) ;
#22750 = ORIENTED_EDGE ( 'NONE', *, *, #33674, .T. ) ;
#22751 = ORIENTED_EDGE ( 'NONE', *, *, #26594, .F. ) ;
#22752 = CARTESIAN_POINT ( 'NONE',  ( -37.66520193420439711, -114.7490116281687023, 7.558975545821551734 ) ) ;
#22753 = ORIENTED_EDGE ( 'NONE', *, *, #2860, .F. ) ;
#22754 = ORIENTED_EDGE ( 'NONE', *, *, #17657, .F. ) ;
#22755 = ORIENTED_EDGE ( 'NONE', *, *, #26210, .F. ) ;
#22756 = CARTESIAN_POINT ( 'NONE',  ( -55.00000000000000000, 0.000000000000000000, 70.00000000000000000 ) ) ;
#22757 = DIRECTION ( 'NONE',  ( -1.000000000000000000, 0.000000000000000000, 0.000000000000000000 ) ) ;
#22758 = CARTESIAN_POINT ( 'NONE',  ( -42.49999999999999289, -39.95319397786859383, 75.20096189432314304 ) ) ;
#22759 = AXIS2_PLACEMENT_3D ( 'NONE', #13205, #21100, #1497 ) ;
#22760 = CARTESIAN_POINT ( 'NONE',  ( -35.97955704204053262, -114.9929510916434339, 13.11812344617474579 ) ) ;
#22761 = CARTESIAN_POINT ( 'NONE',  ( -4.872650870659791522, 0.4273491293403324232, -0.7999999999999893863 ) ) ;
#22762 = CARTESIAN_POINT ( 'NONE',  ( -42.49999999999999289, -25.98076211353320986, 84.99999999999994316 ) ) ;
#22763 = VECTOR ( 'NONE', #21620, 1000.000000000000000 ) ;
#22764 = AXIS2_PLACEMENT_3D ( 'NONE', #24100, #29665, #35086 ) ;
#22765 = EDGE_CURVE ( 'NONE', #24903, #27346, #27975, .T. ) ;
#22766 = DIRECTION ( 'NONE',  ( -1.000000000000000000, -0.000000000000000000, 0.000000000000000000 ) ) ;
#22767 = FACE_OUTER_BOUND ( 'NONE', #12793, .T. ) ;
#22768 = AXIS2_PLACEMENT_3D ( 'NONE', #9422, #20031, #33920 ) ;
#22769 = EDGE_CURVE ( 'NONE', #32263, #30, #12210, .T. ) ;
#22770 = FACE_OUTER_BOUND ( 'NONE', #35470, .T. ) ;
#22771 = ORIENTED_EDGE ( 'NONE', *, *, #17895, .T. ) ;
#22772 = CARTESIAN_POINT ( 'NONE',  ( -39.00000000000000000, -115.9929510916434481, 10.50625754673587053 ) ) ;
#22773 = CARTESIAN_POINT ( 'NONE',  ( -35.50000000000000711, -112.0140978167138712, 0.8127176474015721519 ) ) ;
#22774 = CARTESIAN_POINT ( 'NONE',  ( -1.000000000000014655, -4.808326913196006913, -0.7999999999999951594 ) ) ;
#22775 = AXIS2_PLACEMENT_3D ( 'NONE', #16275, #32153, #29994 ) ;
#22776 = CYLINDRICAL_SURFACE ( 'NONE', #9582, 13.99999999999999822 ) ;
#22777 = CIRCLE ( 'NONE', #4434, 0.5000000000000004441 ) ;
#22778 = CYLINDRICAL_SURFACE ( 'NONE', #14175, 17.49900000000000233 ) ;
#22779 = FACE_OUTER_BOUND ( 'NONE', #7169, .T. ) ;
#22780 = DIRECTION ( 'NONE',  ( -1.000000000000000000, -0.000000000000000000, 0.000000000000000000 ) ) ;
#22781 = CARTESIAN_POINT ( 'NONE',  ( 0.000000000000000000, -27.43636312076294814, -38.14186064215180494 ) ) ;
#22782 = ORIENTED_EDGE ( 'NONE', *, *, #22646, .T. ) ;
#22783 = CARTESIAN_POINT ( 'NONE',  ( -36.02454729103297382, -113.5265240346956261, 5.402725545821552622 ) ) ;
#22784 = FACE_OUTER_BOUND ( 'NONE', #14450, .T. ) ;
#22785 = CARTESIAN_POINT ( 'NONE',  ( 8.000000000000000000, -17.06000345190431844, -10.43821259704038695 ) ) ;
#22786 = VERTEX_POINT ( 'NONE', #14276 ) ;
#22787 = CIRCLE ( 'NONE', #4508, 4.000000000000000000 ) ;
#22788 = ORIENTED_EDGE ( 'NONE', *, *, #24954, .F. ) ;
#22789 = DIRECTION ( 'NONE',  ( -1.000000000000000000, -0.000000000000000000, 0.000000000000000000 ) ) ;
#22790 = CIRCLE ( 'NONE', #25694, 8.000000000000008882 ) ;
#22791 = CARTESIAN_POINT ( 'NONE',  ( 0.000000000000000000, 0.000000000000000000, 65.00000000000000000 ) ) ;
#22792 = ORIENTED_EDGE ( 'NONE', *, *, #27375, .T. ) ;
#22793 = CARTESIAN_POINT ( 'NONE',  ( -35.81662171581203324, -110.9754527089670546, 5.215225545821552622 ) ) ;
#22794 = ORIENTED_EDGE ( 'NONE', *, *, #29385, .F. ) ;
#22795 = AXIS2_PLACEMENT_3D ( 'NONE', #12527, #2098, #13075 ) ;
#22796 = AXIS2_PLACEMENT_3D ( 'NONE', #17158, #27650, #28167 ) ;
#22797 = DIRECTION ( 'NONE',  ( 0.000000000000000000, 0.000000000000000000, -1.000000000000000000 ) ) ;
#22798 = CARTESIAN_POINT ( 'NONE',  ( 7.999999999999992895, 35.20873326984128227, -31.88259874183993503 ) ) ;
#22799 = AXIS2_PLACEMENT_3D ( 'NONE', #35353, #16228, #2247 ) ;
#22800 = SHAPE_DEFINITION_REPRESENTATION ( #28193, #31216 ) ;
#22801 = FACE_OUTER_BOUND ( 'NONE', #31932, .T. ) ;
#22803 = ORIENTED_EDGE ( 'NONE', *, *, #23949, .T. ) ;
#22802 = VECTOR ( 'NONE', #27107, 1000.000000000000000 ) ;
#22804 = ORIENTED_EDGE ( 'NONE', *, *, #8997, .T. ) ;
#22805 = CARTESIAN_POINT ( 'NONE',  ( -44.00000000000000000, -4.000000000000000000, 0.000000000000000000 ) ) ;
#22806 = CARTESIAN_POINT ( 'NONE',  ( 0.000000000000000000, -2.710505431213761085E-17, 45.99999999999998579 ) ) ;
#22807 = VERTEX_POINT ( 'NONE', #6010 ) ;
#22808 = CARTESIAN_POINT ( 'NONE',  ( 8.000000000000000000, -0.9861715913088822116, 17.47118961583599273 ) ) ;
#22809 = CIRCLE ( 'NONE', #33751, 47.49900000000002365 ) ;
#22810 = CARTESIAN_POINT ( 'NONE',  ( -34.50000000000000000, -115.0140978167138712, -0.3747823525984421145 ) ) ;
#22811 = CARTESIAN_POINT ( 'NONE',  ( -39.49999999999999289, -4.633167542791596816, 143.9590043477703887 ) ) ;
#22812 = DIRECTION ( 'NONE',  ( -1.000000000000000000, -0.000000000000000000, -0.000000000000000000 ) ) ;
#22813 = ADVANCED_FACE ( 'NONE', ( #25457 ), #425, .T. ) ;
#22814 = CARTESIAN_POINT ( 'NONE',  ( -34.50000000000000000, -115.9926080209513657, 10.46845107750242398 ) ) ;
#22815 = VECTOR ( 'NONE', #26924, 1000.000000000000000 ) ;
#22816 = CARTESIAN_POINT ( 'NONE',  ( -9.999999999999994671, 0.000000000000000000, 0.000000000000000000 ) ) ;
#22817 = CARTESIAN_POINT ( 'NONE',  ( -37.88768952767750164, -115.9754527089670262, 1.972274454178448710 ) ) ;
#22818 = CARTESIAN_POINT ( 'NONE',  ( -34.50000000000000000, -114.2183886307118428, 8.518969274377507617 ) ) ;
#22819 = CARTESIAN_POINT ( 'NONE',  ( 0.000000000000000000, 18.53613841426789577, 48.58406706613910586 ) ) ;
#22820 = AXIS2_PLACEMENT_3D ( 'NONE', #18812, #10900, #24401 ) ;
#22821 = CARTESIAN_POINT ( 'NONE',  ( 8.000000000000000000, 0.000000000000000000, 0.000000000000000000 ) ) ;
#22822 = CIRCLE ( 'NONE', #35503, 3.799999999999999822 ) ;
#22823 = DIRECTION ( 'NONE',  ( 0.000000000000000000, 0.000000000000000000, 1.000000000000000000 ) ) ;
#22824 = DIRECTION ( 'NONE',  ( 0.000000000000000000, 0.000000000000000000, -1.000000000000000000 ) ) ;
#22825 = ORIENTED_EDGE ( 'NONE', *, *, #35406, .T. ) ;
#22826 = AXIS2_PLACEMENT_3D ( 'NONE', #10585, #13298, #10763 ) ;
#22827 = CARTESIAN_POINT ( 'NONE',  ( 8.000000000000000000, 16.59870953437680896, 3.253005020243904255 ) ) ;
#22828 = ORIENTED_EDGE ( 'NONE', *, *, #12085, .T. ) ;
#22829 = CIRCLE ( 'NONE', #16509, 11.00000000000001066 ) ;
#22830 = EDGE_CURVE ( 'NONE', #793, #12715, #24860, .T. ) ;
#22831 = CARTESIAN_POINT ( 'NONE',  ( -38.30190309005061522, -111.0245472910330022, 3.527725545821551734 ) ) ;
#22832 = DIRECTION ( 'NONE',  ( 0.000000000000000000, 0.000000000000000000, 1.000000000000000000 ) ) ;
#22833 = CARTESIAN_POINT ( 'NONE',  ( -35.50000000000000711, -116.0140896356112989, -0.6575071456984549201 ) ) ;
#22834 = VERTEX_POINT ( 'NONE', #33206 ) ;
#22835 = ORIENTED_EDGE ( 'NONE', *, *, #34122, .T. ) ;
#22836 = LINE ( 'NONE', #8974, #17692 ) ;
#22837 = DIRECTION ( 'NONE',  ( 0.000000000000000000, 0.000000000000000000, 1.000000000000000000 ) ) ;
#22838 = ORIENTED_EDGE ( 'NONE', *, *, #3592, .F. ) ;
#22839 = ORIENTED_EDGE ( 'NONE', *, *, #25959, .F. ) ;
#22840 = AXIS2_PLACEMENT_3D ( 'NONE', #24792, #27145, #117 ) ;
#22841 = DIRECTION ( 'NONE',  ( 0.000000000000000000, 0.9848077530122085754, -0.1736481776669275556 ) ) ;
#22842 = VERTEX_POINT ( 'NONE', #16969 ) ;
#22843 = ORIENTED_EDGE ( 'NONE', *, *, #22303, .F. ) ;
#22844 = CARTESIAN_POINT ( 'NONE',  ( -38.37230871539094323, -115.4561184093552413, 6.058975545821551734 ) ) ;
#22845 = AXIS2_PLACEMENT_3D ( 'NONE', #1838, #12813, #18557 ) ;
#22846 = DIRECTION ( 'NONE',  ( 0.000000000000000000, 0.000000000000000000, 1.000000000000000000 ) ) ;
#22847 = DIRECTION ( 'NONE',  ( 0.000000000000000000, 0.000000000000000000, 1.000000000000000000 ) ) ;
#22848 = ORIENTED_EDGE ( 'NONE', *, *, #1833, .F. ) ;
#22849 = ORIENTED_EDGE ( 'NONE', *, *, #34662, .F. ) ;
#22850 = CARTESIAN_POINT ( 'NONE',  ( -35.50000000000000000, -116.9119893297194324, -1.269118781492768910 ) ) ;
#22851 = AXIS2_PLACEMENT_3D ( 'NONE', #13351, #21600, #7934 ) ;
#22852 = DIRECTION ( 'NONE',  ( -1.000000000000000000, -1.836970198721029934E-16, -0.000000000000000000 ) ) ;
#22853 = ORIENTED_EDGE ( 'NONE', *, *, #9976, .T. ) ;
#22854 = CARTESIAN_POINT ( 'NONE',  ( -37.42187499999997158, -114.9929510916434339, 13.11852480586264669 ) ) ;
#22855 = EDGE_CURVE ( 'NONE', #31626, #3021, #3027, .T. ) ;
#22856 = CARTESIAN_POINT ( 'NONE',  ( -39.00000000000000000, -113.9929510916434339, 12.59652202191340820 ) ) ;
#22857 = EDGE_CURVE ( 'NONE', #9043, #34436, #27744, .T. ) ;
#22858 = DIRECTION ( 'NONE',  ( 0.000000000000000000, 0.000000000000000000, 1.000000000000000000 ) ) ;
#22859 = DIRECTION ( 'NONE',  ( 1.000000000000000000, 1.836970198721029934E-16, 0.000000000000000000 ) ) ;
#22860 = CARTESIAN_POINT ( 'NONE',  ( -37.56132887387857267, -113.9929510916434339, 14.11732072679899197 ) ) ;
#22861 = CARTESIAN_POINT ( 'NONE',  ( 7.999999999999992895, 24.72041153920790180, -40.55929306992661765 ) ) ;
#22862 = CARTESIAN_POINT ( 'NONE',  ( -35.50000000000000711, -114.9929510916434339, 12.59652202191340642 ) ) ;
#22863 = VECTOR ( 'NONE', #26709, 1000.000000000000000 ) ;
#22864 = CYLINDRICAL_SURFACE ( 'NONE', #31445, 11.00000000000000000 ) ;
#22865 = ORIENTED_EDGE ( 'NONE', *, *, #21889, .F. ) ;
#22866 = CARTESIAN_POINT ( 'NONE',  ( 8.000000000000007105, 5.908880290975762506, -9.604183132802354805 ) ) ;
#22867 = LINE ( 'NONE', #33864, #3716 ) ;
#22868 = ORIENTED_EDGE ( 'NONE', *, *, #2660, .T. ) ;
#22869 = CARTESIAN_POINT ( 'NONE',  ( -35.50000000000000711, -114.9819937217110635, 10.35556074009299188 ) ) ;
#22870 = ORIENTED_EDGE ( 'NONE', *, *, #3298, .F. ) ;
#22871 = ADVANCED_FACE ( 'NONE', ( #16798 ), #14624, .T. ) ;
#22872 = CYLINDRICAL_SURFACE ( 'NONE', #26422, 47.49900000000001654 ) ;
#22873 = DIRECTION ( 'NONE',  ( 0.000000000000000000, 0.000000000000000000, -1.000000000000000000 ) ) ;
#22874 = CIRCLE ( 'NONE', #15958, 17.49900000000000944 ) ;
#22875 = EDGE_CURVE ( 'NONE', #15170, #13248, #14816, .T. ) ;
#22876 = EDGE_LOOP ( 'NONE', ( #5945, #2499, #34377, #27905 ) ) ;
#22877 = CIRCLE ( 'NONE', #30358, 4.000000000000003553 ) ;
#22878 = CARTESIAN_POINT ( 'NONE',  ( 1.479000000000008752, -4.846123502488801633E-16, -6.984000000000015085 ) ) ;
#22879 = VERTEX_POINT ( 'NONE', #33725 ) ;
#22880 = CARTESIAN_POINT ( 'NONE',  ( -35.50000000000000000, -115.0140978167138712, 0.3752176474015736507 ) ) ;
#22881 = DIRECTION ( 'NONE',  ( -1.000000000000000000, 0.000000000000000000, 0.000000000000000000 ) ) ;
#22882 = CARTESIAN_POINT ( 'NONE',  ( -35.00000000000000000, -114.0592624029313242, 3.003524454178448710 ) ) ;
#22883 = ORIENTED_EDGE ( 'NONE', *, *, #4071, .F. ) ;
#22884 = STYLED_ITEM ( 'NONE', ( #32539 ), #33931 ) ;
#22885 = CARTESIAN_POINT ( 'NONE',  ( -37.88768952767750164, -115.9754527089670262, 4.972274454178448266 ) ) ;
#22886 = DIRECTION ( 'NONE',  ( 1.000000000000000000, 0.000000000000000000, 0.000000000000000000 ) ) ;
#22887 = CARTESIAN_POINT ( 'NONE',  ( -35.50000000000000711, -112.0140900043366088, -0.5935324770972457697 ) ) ;
#22888 = ORIENTED_EDGE ( 'NONE', *, *, #25166, .T. ) ;
#22889 = ORIENTED_EDGE ( 'NONE', *, *, #26543, .T. ) ;
#22890 = DIRECTION ( 'NONE',  ( 0.000000000000000000, -0.6845471059286794002, -0.7289686274214203232 ) ) ;
#22891 = ADVANCED_FACE ( 'NONE', ( #19502 ), #9062, .T. ) ;
#22892 = CARTESIAN_POINT ( 'NONE',  ( 0.000000000000000000, 0.000000000000000000, -53.39999999999999858 ) ) ;
#22893 = VERTEX_POINT ( 'NONE', #33907 ) ;
#22894 = ORIENTED_EDGE ( 'NONE', *, *, #3697, .T. ) ;
#22895 = CARTESIAN_POINT ( 'NONE',  ( -34.50000000000000000, -115.1770117227680998, -1.611965039240062181 ) ) ;
#22896 = CARTESIAN_POINT ( 'NONE',  ( -35.50000000000000711, -112.4434344552011282, 1.705278471174987986 ) ) ;
#22897 = VERTEX_POINT ( 'NONE', #20193 ) ;
#22898 = ORIENTED_EDGE ( 'NONE', *, *, #13450, .T. ) ;
#22899 = DIRECTION ( 'NONE',  ( -1.000000000000000000, 0.000000000000000000, 0.000000000000000000 ) ) ;
#22900 = CIRCLE ( 'NONE', #17156, 47.49900000000000944 ) ;
#22901 = SHAPE_REPRESENTATION ( 'spur gear_iso_ISO - Spur gear 2M 12T 20PA 8FW ---S12A75H50L8.0S1', ( #21307 ), #27126 ) ;
#22902 = EDGE_CURVE ( 'NONE', #29247, #32761, #34656, .T. ) ;
#22903 = CARTESIAN_POINT ( 'NONE',  ( -35.99181955245763476, -113.9929510916434339, 13.11847460610632510 ) ) ;
#22904 = CARTESIAN_POINT ( 'NONE',  ( -34.50000000000000000, -112.8356783780338759, 1.859636627348750348 ) ) ;
#22905 = EDGE_CURVE ( 'NONE', #32382, #7789, #14100, .T. ) ;
#22906 = DIRECTION ( 'NONE',  ( 0.000000000000000000, 0.000000000000000000, -1.000000000000000000 ) ) ;
#22907 = EDGE_CURVE ( 'NONE', #12814, #33791, #12779, .T. ) ;
#22908 = CARTESIAN_POINT ( 'NONE',  ( -36.87500000000098765, -113.9929510916434339, 13.11852480586264846 ) ) ;
#22909 = CARTESIAN_POINT ( 'NONE',  ( -35.50000000000000000, -115.9915791193162420, 10.43066258751475139 ) ) ;
#22910 = DIRECTION ( 'NONE',  ( 0.000000000000000000, 0.000000000000000000, 1.000000000000000000 ) ) ;
#22911 = CYLINDRICAL_SURFACE ( 'NONE', #7724, 17.49900000000000233 ) ;
#22912 = EDGE_CURVE ( 'NONE', #32703, #24948, #29232, .T. ) ;
#22913 = DIRECTION ( 'NONE',  ( 0.000000000000000000, -0.8660254037844326014, -0.5000000000000102141 ) ) ;
#22914 = DIRECTION ( 'NONE',  ( 1.541976423090495387E-16, -1.000000000000000000, 0.000000000000000000 ) ) ;
#22915 = CARTESIAN_POINT ( 'NONE',  ( 55.00000000000000000, 10.00000000000000888, 110.0000000000000000 ) ) ;
#22916 = EDGE_CURVE ( 'NONE', #7584, #18156, #1869, .T. ) ;
#22917 = ORIENTED_EDGE ( 'NONE', *, *, #18842, .F. ) ;
#22918 = DIRECTION ( 'NONE',  ( -1.000000000000000000, 0.000000000000000000, 0.000000000000000000 ) ) ;
#22919 = CARTESIAN_POINT ( 'NONE',  ( 8.000000000000000000, 5.400000000000000355, 0.9999999999999985567 ) ) ;
#22920 = CARTESIAN_POINT ( 'NONE',  ( 8.000000000000007105, 0.000000000000000000, 0.000000000000000000 ) ) ;
#22921 = DIRECTION ( 'NONE',  ( 0.000000000000000000, -0.6845471059286952764, 0.7289686274214054462 ) ) ;
#22922 = FACE_BOUND ( 'NONE', #21597, .T. ) ;
#22923 = PLANE ( 'NONE',  #16449 ) ;
#22924 = ORIENTED_EDGE ( 'NONE', *, *, #17612, .T. ) ;
#22925 = VECTOR ( 'NONE', #2603, 1000.000000000000000 ) ;
#22926 = DIRECTION ( 'NONE',  ( 1.000000000000000000, -0.000000000000000000, -0.000000000000000000 ) ) ;
#22927 = CARTESIAN_POINT ( 'NONE',  ( 46.00000000000000000, -25.98076211353320275, 73.99999999999992895 ) ) ;
#22928 = DIRECTION ( 'NONE',  ( 0.000000000000000000, 0.8443279255020126328, 0.5358267949790005424 ) ) ;
#22929 = EDGE_LOOP ( 'NONE', ( #6416, #2561, #23168, #19952 ) ) ;
#22930 = ORIENTED_EDGE ( 'NONE', *, *, #4225, .T. ) ;
#22931 = CARTESIAN_POINT ( 'NONE',  ( -36.02454729103298092, -114.4734759653044307, 1.597274454178448932 ) ) ;
#22932 = ORIENTED_EDGE ( 'NONE', *, *, #6928, .T. ) ;
#22933 = ADVANCED_FACE ( 'NONE', ( #25821 ), #31735, .T. ) ;
#22934 =( LENGTH_UNIT ( ) NAMED_UNIT ( * ) SI_UNIT ( .MILLI., .METRE. ) );
#22935 = ORIENTED_EDGE ( 'NONE', *, *, #32420, .T. ) ;
#22936 = VERTEX_POINT ( 'NONE', #4577 ) ;
#22937 = LINE ( 'NONE', #30875, #19484 ) ;
#22938 = EDGE_CURVE ( 'NONE', #5386, #128, #31197, .T. ) ;
#22939 = CARTESIAN_POINT ( 'NONE',  ( 0.000000000000000000, 0.000000000000000000, 0.000000000000000000 ) ) ;
#22940 = DIRECTION ( 'NONE',  ( 0.000000000000000000, 0.000000000000000000, -1.000000000000000000 ) ) ;
#22941 = CARTESIAN_POINT ( 'NONE',  ( -35.50000000000000711, -114.9929510916434339, 10.61627146648203812 ) ) ;
#22942 = CARTESIAN_POINT ( 'NONE',  ( 7.999999999999992895, 0.000000000000000000, 0.000000000000000000 ) ) ;
#22943 = ADVANCED_FACE ( 'NONE', ( #34456 ), #28692, .T. ) ;
#22944 = CIRCLE ( 'NONE', #7434, 22.00000000000000000 ) ;
#22945 = DIRECTION ( 'NONE',  ( 0.000000000000000000, -8.881784197001252323E-16, -1.000000000000000000 ) ) ;
#22946 = EDGE_CURVE ( 'NONE', #33265, #32057, #20251, .T. ) ;
#22947 = CARTESIAN_POINT ( 'NONE',  ( -34.50000000000000000, -114.9860996047076895, 10.38555023491505835 ) ) ;
#22948 = DIRECTION ( 'NONE',  ( 0.000000000000000000, 0.000000000000000000, 1.000000000000000000 ) ) ;
#22949 = CIRCLE ( 'NONE', #27583, 14.70000000000000107 ) ;
#22950 = CARTESIAN_POINT ( 'NONE',  ( -36.49999999999999289, -15.63316754279159326, 121.0048025873809792 ) ) ;
#22951 = ORIENTED_EDGE ( 'NONE', *, *, #33966, .T. ) ;
#22952 = CIRCLE ( 'NONE', #10335, 4.980000000000017302 ) ;
#22953 = CARTESIAN_POINT ( 'NONE',  ( -39.00000000000000000, -115.9929510916434481, 10.85830208992306822 ) ) ;
#22954 = CARTESIAN_POINT ( 'NONE',  ( -35.50000000000000711, -113.1256619669233885, 1.895633585076891947 ) ) ;
#22955 = LINE ( 'NONE', #19879, #21449 ) ;
#22956 = FACE_OUTER_BOUND ( 'NONE', #11871, .T. ) ;
#22957 = CARTESIAN_POINT ( 'NONE',  ( 0.000000000000000000, -39.55064067543080597, 25.36340625197344778 ) ) ;
#22958 = FACE_OUTER_BOUND ( 'NONE', #9370, .T. ) ;
#22959 = DIRECTION ( 'NONE',  ( 0.000000000000000000, 0.000000000000000000, 1.000000000000000000 ) ) ;
#22960 = CARTESIAN_POINT ( 'NONE',  ( 7.999999999999992895, 41.20225022064671805, -23.63323037071357646 ) ) ;
#22961 = CYLINDRICAL_SURFACE ( 'NONE', #21263, 52.00000000000000711 ) ;
#22962 = VERTEX_POINT ( 'NONE', #4038 ) ;
#22963 = CARTESIAN_POINT ( 'NONE',  ( -36.64504884055821776, -112.9754527089670688, 6.715225545821551734 ) ) ;
#22964 = LINE ( 'NONE', #19889, #4321 ) ;
#22965 = DIRECTION ( 'NONE',  ( -1.000000000000000000, 5.339440136655842133E-16, 1.047965281155519420E-16 ) ) ;
#22966 = ORIENTED_EDGE ( 'NONE', *, *, #11943, .T. ) ;
#22967 = ORIENTED_EDGE ( 'NONE', *, *, #10637, .F. ) ;
#22968 =( LENGTH_UNIT ( ) NAMED_UNIT ( * ) SI_UNIT ( .MILLI., .METRE. ) );
#22969 = DIRECTION ( 'NONE',  ( -1.783119874454246424E-31, -1.187911941725854497E-31, 1.000000000000000000 ) ) ;
#22970 = ORIENTED_EDGE ( 'NONE', *, *, #14084, .F. ) ;
#22971 = CARTESIAN_POINT ( 'NONE',  ( -35.81662171581204746, -117.0245472910329738, 6.284774454178449155 ) ) ;
#22972 = ORIENTED_EDGE ( 'NONE', *, *, #4724, .T. ) ;
#22973 = EDGE_CURVE ( 'NONE', #15039, #27914, #17380, .T. ) ;
#22974 = AXIS2_PLACEMENT_3D ( 'NONE', #27180, #35114, #15989 ) ;
#22975 = EDGE_CURVE ( 'NONE', #28212, #25659, #29038, .T. ) ;
#22976 = DIRECTION ( 'NONE',  ( 5.339440136655842133E-16, 1.000000000000000000, -1.918536189538073087E-16 ) ) ;
#22977 = DIRECTION ( 'NONE',  ( 0.000000000000000000, 0.000000000000000000, 1.000000000000000000 ) ) ;
#22978 = VECTOR ( 'NONE', #1545, 1000.000000000000000 ) ;
#22979 = CARTESIAN_POINT ( 'NONE',  ( 8.000000000000000000, 4.898587196589412829E-16, -4.000000000000000000 ) ) ;
#22980 = AXIS2_PLACEMENT_3D ( 'NONE', #14347, #27871, #4804 ) ;
#22981 = APPLICATION_PROTOCOL_DEFINITION ( 'draft international standard', 'automotive_design', 1998, #8951 ) ;
#22982 = CARTESIAN_POINT ( 'NONE',  ( -46.00000000000000000, -25.98076211353320275, 84.99999999999992895 ) ) ;
#22983 = VERTEX_POINT ( 'NONE', #15334 ) ;
#22984 = ORIENTED_EDGE ( 'NONE', *, *, #9856, .T. ) ;
#22985 = DIRECTION ( 'NONE',  ( -1.000000000000000000, -1.836970198721029934E-16, -0.000000000000000000 ) ) ;
#22986 = CARTESIAN_POINT ( 'NONE',  ( 8.000000000000007105, -9.604183132802312173, -1.108880290975637228 ) ) ;
#22987 = ORIENTED_EDGE ( 'NONE', *, *, #28230, .T. ) ;
#22988 = CARTESIAN_POINT ( 'NONE',  ( -3.799999999999999822, 4.653657836759942730E-16, -52.50000000000000000 ) ) ;
#22989 = CARTESIAN_POINT ( 'NONE',  ( -34.50000000000000000, -112.8356783780338759, 1.859636627348750348 ) ) ;
#22990 = DIRECTION ( 'NONE',  ( 1.000000000000000000, -0.000000000000000000, 0.000000000000000000 ) ) ;
#22991 = CARTESIAN_POINT ( 'NONE',  ( 0.000000000000000000, 0.000000000000000000, -49.10000000000000142 ) ) ;
#22992 =( REPRESENTATION_RELATIONSHIP ('NONE','NONE', #26607, #31430 ) REPRESENTATION_RELATIONSHIP_WITH_TRANSFORMATION ( #22044 )SHAPE_REPRESENTATION_RELATIONSHIP( ) );
#22993 = CARTESIAN_POINT ( 'NONE',  ( -34.50000000000000000, -115.9929510916434481, 10.68227981832981044 ) ) ;
#22994 = AXIS2_PLACEMENT_3D ( 'NONE', #18792, #18615, #32666 ) ;
#22995 = DIRECTION ( 'NONE',  ( -1.000000000000000000, 0.000000000000000000, 0.000000000000000000 ) ) ;
#22996 = DIRECTION ( 'NONE',  ( 0.000000000000000000, 0.000000000000000000, 1.000000000000000000 ) ) ;
#22997 = CARTESIAN_POINT ( 'NONE',  ( -38.98797722933582577, -114.9929510916434339, 12.81430620224974959 ) ) ;
#22998 = CARTESIAN_POINT ( 'NONE',  ( 0.000000000000000000, 0.000000000000000000, -32.00000000000000000 ) ) ;
#22999 = DIRECTION ( 'NONE',  ( -1.000000000000000000, 0.000000000000000000, 0.000000000000000000 ) ) ;
#23000 = CIRCLE ( 'NONE', #28750, 7.999999999999992895 ) ;
#23001 = DIRECTION ( 'NONE',  ( -1.000000000000000000, -0.000000000000000000, -0.000000000000000000 ) ) ;
#23002 = DIRECTION ( 'NONE',  ( 0.000000000000000000, 0.000000000000000000, -1.000000000000000000 ) ) ;
#23003 = EDGE_LOOP ( 'NONE', ( #9150, #15670, #32939, #26728 ) ) ;
#23004 = FACE_OUTER_BOUND ( 'NONE', #33790, .T. ) ;
#23005 = ORIENTED_EDGE ( 'NONE', *, *, #28049, .T. ) ;
#23006 = CIRCLE ( 'NONE', #20114, 3.799999999999999822 ) ;
#23007 = AXIS2_PLACEMENT_3D ( 'NONE', #7213, #16015, #1837 ) ;
#23008 = CARTESIAN_POINT ( 'NONE',  ( -33.97545270896703329, -115.1833782841879810, 5.590225545821552622 ) ) ;
#23009 = CIRCLE ( 'NONE', #22439, 20.00000000000001421 ) ;
#23010 = DIRECTION ( 'NONE',  ( -1.000000000000000000, 0.000000000000000000, 0.000000000000000000 ) ) ;
#23011 = CARTESIAN_POINT ( 'NONE',  ( -35.50000000000000711, -116.0140978167138712, -0.3122823525984417259 ) ) ;
#23012 = ORIENTED_EDGE ( 'NONE', *, *, #15581, .T. ) ;
#23013 = VERTEX_POINT ( 'NONE', #34088 ) ;
#23015 = DIRECTION ( 'NONE',  ( -1.734723475976807094E-16, -0.4999999999999928946, -0.8660254037844427044 ) ) ;
#23014 = PRODUCT_DEFINITION_SHAPE ( 'NONE', 'NONE',  #35634 ) ;
#23016 = CYLINDRICAL_SURFACE ( 'NONE', #15177, 9.499000000000000554 ) ;
#23017 = ORIENTED_EDGE ( 'NONE', *, *, #30126, .F. ) ;
#23018 = ORIENTED_EDGE ( 'NONE', *, *, #19154, .F. ) ;
#23019 = EDGE_CURVE ( 'NONE', #9731, #352, #34083, .T. ) ;
#23020 = DIRECTION ( 'NONE',  ( -1.000000000000000000, 0.000000000000000000, 0.000000000000000000 ) ) ;
#23021 = ORIENTED_EDGE ( 'NONE', *, *, #24985, .F. ) ;
#23022 = CARTESIAN_POINT ( 'NONE',  ( -38.99999999999999289, -114.0592624029313242, 3.246475545821551734 ) ) ;
#23023 = DIRECTION ( 'NONE',  ( 0.000000000000000000, 0.000000000000000000, 1.000000000000000000 ) ) ;
#23024 = VERTEX_POINT ( 'NONE', #12664 ) ;
#23025 = ORIENTED_EDGE ( 'NONE', *, *, #24954, .T. ) ;
#23026 = AXIS2_PLACEMENT_3D ( 'NONE', #23721, #12570, #20815 ) ;
#23027 = CARTESIAN_POINT ( 'NONE',  ( -35.50000000000000000, -116.2431927316855109, -2.224114562372550008 ) ) ;
#23028 = EDGE_CURVE ( 'NONE', #11969, #6500, #23641, .T. ) ;
#23029 = FACE_OUTER_BOUND ( 'NONE', #21016, .T. ) ;
#23030 = AXIS2_PLACEMENT_3D ( 'NONE', #9604, #26715, #15161 ) ;
#23031 = AXIS2_PLACEMENT_3D ( 'NONE', #34690, #9662, #14872 ) ;
#23032 = ORIENTED_EDGE ( 'NONE', *, *, #30246, .F. ) ;
#23033 = CARTESIAN_POINT ( 'NONE',  ( -37.99959864031215773, -114.9929510916434339, 12.63896776382213538 ) ) ;
#23034 = AXIS2_PLACEMENT_3D ( 'NONE', #27171, #13476, #31841 ) ;
#23035 = CARTESIAN_POINT ( 'NONE',  ( -39.00000000000000000, -113.9929510916434339, 12.44250253426875119 ) ) ;
#23036 = CARTESIAN_POINT ( 'NONE',  ( 0.000000000000000000, 0.000000000000000000, 0.000000000000000000 ) ) ;
#23037 = CARTESIAN_POINT ( 'NONE',  ( 0.000000000000000000, 0.000000000000000000, 20.00000000000000000 ) ) ;
#23038 = CARTESIAN_POINT ( 'NONE',  ( -37.34375000000001421, -113.9929510916434339, 14.11852480586265024 ) ) ;
#23039 = LINE ( 'NONE', #22861, #21714 ) ;
#23040 = CARTESIAN_POINT ( 'NONE',  ( -36.06250000000002132, -114.9929510916434339, 13.11852480586264669 ) ) ;
#23041 = DIRECTION ( 'NONE',  ( 0.000000000000000000, -0.8090169943749405679, -0.5877852522924826850 ) ) ;
#23042 = VERTEX_POINT ( 'NONE', #9950 ) ;
#23043 = FACE_OUTER_BOUND ( 'NONE', #9674, .T. ) ;
#23044 = FACE_BOUND ( 'NONE', #10558, .T. ) ;
#23045 = ORIENTED_EDGE ( 'NONE', *, *, #7214, .T. ) ;
#23046 = CARTESIAN_POINT ( 'NONE',  ( -35.50000000000000711, -114.9912366357066986, 10.44580456020104720 ) ) ;
#23047 = EDGE_LOOP ( 'NONE', ( #23517, #25530, #3163, #18911 ) ) ;
#23048 = CIRCLE ( 'NONE', #19044, 8.000000000000001776 ) ;
#23049 = DIRECTION ( 'NONE',  ( 0.000000000000000000, 0.000000000000000000, 1.000000000000000000 ) ) ;
#23050 = ORIENTED_EDGE ( 'NONE', *, *, #8077, .F. ) ;
#23051 = DIRECTION ( 'NONE',  ( -1.734723475976806848E-16, -0.8660254037844350439, -0.5000000000000061062 ) ) ;
#23052 = ORIENTED_EDGE ( 'NONE', *, *, #15173, .F. ) ;
#23053 = CARTESIAN_POINT ( 'NONE',  ( -35.50000000000000000, -114.8057644833805853, -0.6247823525984269599 ) ) ;
#23054 = DIRECTION ( 'NONE',  ( 0.000000000000000000, 0.000000000000000000, 1.000000000000000000 ) ) ;
#23055 = DIRECTION ( 'NONE',  ( 0.000000000000000000, 0.000000000000000000, -1.000000000000000000 ) ) ;
#23056 = VECTOR ( 'NONE', #25244, 1000.000000000000000 ) ;
#23057 =( GEOMETRIC_REPRESENTATION_CONTEXT ( 3 ) GLOBAL_UNCERTAINTY_ASSIGNED_CONTEXT ( ( #33022 ) ) GLOBAL_UNIT_ASSIGNED_CONTEXT ( ( #22934, #14299, #11601 ) ) REPRESENTATION_CONTEXT ( 'NONE', 'WORKASPACE' ) );
#23058 = VERTEX_POINT ( 'NONE', #32099 ) ;
#23059 = AXIS2_PLACEMENT_3D ( 'NONE', #30047, #5385, #19046 ) ;
#23060 = CARTESIAN_POINT ( 'NONE',  ( -38.97545270896704039, -113.1123104723225197, 2.347274454178448710 ) ) ;
#23061 = CARTESIAN_POINT ( 'NONE',  ( 0.1717365941144993746, -6.008326913195982222, -0.7999999999999951594 ) ) ;
#23062 = ADVANCED_FACE ( 'NONE', ( #20912 ), #31909, .F. ) ;
#23063 = CARTESIAN_POINT ( 'NONE',  ( -35.50000000000000711, -112.0651520602111191, -0.9469505670458575608 ) ) ;
#23064 = ORIENTED_EDGE ( 'NONE', *, *, #23395, .F. ) ;
#23065 = EDGE_LOOP ( 'NONE', ( #33630, #25908, #33032, #32139 ) ) ;
#23066 = EDGE_CURVE ( 'NONE', #29327, #25342, #17973, .T. ) ;
#23067 = PLANE ( 'NONE',  #15908 ) ;
#23068 = SURFACE_STYLE_FILL_AREA ( #15132 ) ;
#23069 = DIRECTION ( 'NONE',  ( 0.000000000000000000, 0.000000000000000000, -1.000000000000000000 ) ) ;
#23070 = ORIENTED_EDGE ( 'NONE', *, *, #19007, .F. ) ;
#23071 = ORIENTED_EDGE ( 'NONE', *, *, #29968, .F. ) ;
#23072 = CARTESIAN_POINT ( 'NONE',  ( -34.50000000000000000, -116.0140978167138712, -0.3747823525984422255 ) ) ;
#23073 = CARTESIAN_POINT ( 'NONE',  ( -35.50000000000000711, -113.8159288351371714, 1.978028123174813802 ) ) ;
#23074 = ADVANCED_FACE ( 'NONE', ( #1145 ), #4215, .F. ) ;
#23075 = ORIENTED_EDGE ( 'NONE', *, *, #35406, .F. ) ;
#23076 = ORIENTED_EDGE ( 'NONE', *, *, #17174, .T. ) ;
#23077 = CARTESIAN_POINT ( 'NONE',  ( 0.000000000000000000, -0.6505223195679143977, -51.99593080916758936 ) ) ;
#23078 = CARTESIAN_POINT ( 'NONE',  ( -37.58145695302688694, -113.9929510916434339, 13.11211614918362756 ) ) ;
#23079 = DIRECTION ( 'NONE',  ( 0.000000000000000000, -1.000000000000000000, 0.000000000000000000 ) ) ;
#23080 = CARTESIAN_POINT ( 'NONE',  ( 0.000000000000000000, 0.000000000000000000, 0.000000000000000000 ) ) ;
#23081 = CIRCLE ( 'NONE', #20185, 3.799999999999999822 ) ;
#23082 = CIRCLE ( 'NONE', #2427, 20.00000000000000711 ) ;
#23083 = CARTESIAN_POINT ( 'NONE',  ( -35.50000000000000000, -113.9929510916434339, 10.61627146648203990 ) ) ;
#23084 = CARTESIAN_POINT ( 'NONE',  ( -35.50000000000000000, -115.9929510916434481, 12.53051367006571581 ) ) ;
#23085 = DIRECTION ( 'NONE',  ( -1.000000000000000000, -0.000000000000000000, -0.000000000000000000 ) ) ;
#23086 = CARTESIAN_POINT ( 'NONE',  ( 50.00005079999999680, 6.071532165918824830E-15, 1.000000000000000000 ) ) ;
#23087 = CARTESIAN_POINT ( 'NONE',  ( 7.999999999999992895, -35.20873326984057883, -31.88259874184068465 ) ) ;
#23088 = DIRECTION ( 'NONE',  ( 1.000000000000000000, 0.000000000000000000, 0.000000000000000000 ) ) ;
#23089 = DIRECTION ( 'NONE',  ( 0.000000000000000000, 0.000000000000000000, 1.000000000000000000 ) ) ;
#23090 = EDGE_CURVE ( 'NONE', #16551, #20133, #31788, .T. ) ;
#23091 = ORIENTED_EDGE ( 'NONE', *, *, #22376, .T. ) ;
#23092 = VECTOR ( 'NONE', #23133, 1000.000000000000000 ) ;
#23093 = CARTESIAN_POINT ( 'NONE',  ( 7.999999999999992895, -24.72041153920704915, -40.55929306992714345 ) ) ;
#23094 = CARTESIAN_POINT ( 'NONE',  ( -35.50000000000000711, -113.0796441757086939, 1.890140615870383956 ) ) ;
#23095 = CARTESIAN_POINT ( 'NONE',  ( 0.000000000000000000, 12.49559743815794199, -9.169462670380459812 ) ) ;
#23096 = ITEM_DEFINED_TRANSFORMATION ( 'NONE', 'NONE', #13847,  #21307 ) ;
#23097 = DIRECTION ( 'NONE',  ( 0.000000000000000000, 0.000000000000000000, 1.000000000000000000 ) ) ;
#23098 = PLANE ( 'NONE',  #11302 ) ;
#23099 = EDGE_LOOP ( 'NONE', ( #11457, #14598 ) ) ;
#23100 = CARTESIAN_POINT ( 'NONE',  ( 8.000000000000000000, -16.92083251265322374, -4.460989585141144076 ) ) ;
#23101 = ADVANCED_FACE ( 'NONE', ( #34265 ), #9597, .F. ) ;
#23102 = CARTESIAN_POINT ( 'NONE',  ( -34.50000000000000000, -111.7850029017436810, -2.224114562373086912 ) ) ;
#23103 = CARTESIAN_POINT ( 'NONE',  ( 4.000000000000003553, -46.77034588191288833, -22.72740077717277885 ) ) ;
#23104 = ORIENTED_EDGE ( 'NONE', *, *, #5170, .F. ) ;
#23105 = EDGE_LOOP ( 'NONE', ( #33125, #19261 ) ) ;
#23106 = EDGE_CURVE ( 'NONE', #15608, #5432, #16818, .T. ) ;
#23107 = CARTESIAN_POINT ( 'NONE',  ( -36.02454729103298092, -114.4734759653044307, 4.597274454178449155 ) ) ;
#23108 = EDGE_CURVE ( 'NONE', #10958, #14939, #11652, .T. ) ;
#23109 = VERTEX_POINT ( 'NONE', #2047 ) ;
#23110 = AXIS2_PLACEMENT_3D ( 'NONE', #1041, #34522, #23527 ) ;
#23111 = PRESENTATION_LAYER_ASSIGNMENT (  '', '', ( #3012 ) ) ;
#23112 = AXIS2_PLACEMENT_3D ( 'NONE', #24419, #2469, #26961 ) ;
#23113 =( NAMED_UNIT ( * ) PLANE_ANGLE_UNIT ( ) SI_UNIT ( $, .RADIAN. ) );
#23114 = VERTEX_POINT ( 'NONE', #4923 ) ;
#23115 = ORIENTED_EDGE ( 'NONE', *, *, #6391, .T. ) ;
#23116 = CARTESIAN_POINT ( 'NONE',  ( -34.50000000000000000, -113.3822401464312719, 0.9191614010536472978 ) ) ;
#23117 = EDGE_CURVE ( 'NONE', #17886, #10094, #2404, .T. ) ;
#23118 = CARTESIAN_POINT ( 'NONE',  ( 50.00000000000000000, -25.98076211353320275, 84.99999999999992895 ) ) ;
#23119 = EDGE_CURVE ( 'NONE', #9483, #3997, #32629, .T. ) ;
#23120 = DIRECTION ( 'NONE',  ( 1.000000000000000000, 0.000000000000000000, 0.000000000000000000 ) ) ;
#23121 = VECTOR ( 'NONE', #18446, 1000.000000000000000 ) ;
#23122 = CARTESIAN_POINT ( 'NONE',  ( -35.56312645773537895, -114.9929510916434339, 12.87038173996308998 ) ) ;
#23123 = CARTESIAN_POINT ( 'NONE',  ( 0.000000000000000000, -13.61301047812905907, -3.268936481846298925 ) ) ;
#23124 = CARTESIAN_POINT ( 'NONE',  ( 7.999999999999992895, 0.000000000000000000, 0.000000000000000000 ) ) ;
#23125 = CARTESIAN_POINT ( 'NONE',  ( -35.98977351030467986, -114.9929510916434339, 14.11852173794918386 ) ) ;
#23126 = LINE ( 'NONE', #26928, #32386 ) ;
#23127 = VECTOR ( 'NONE', #22503, 1000.000000000000000 ) ;
#23128 = DIRECTION ( 'NONE',  ( 1.000000000000000000, -0.000000000000000000, -0.000000000000000000 ) ) ;
#23129 = ORIENTED_EDGE ( 'NONE', *, *, #32376, .T. ) ;
#23130 = CARTESIAN_POINT ( 'NONE',  ( -35.50000000000000000, -115.9929492010520846, 10.50058572605509966 ) ) ;
#23132 = CARTESIAN_POINT ( 'NONE',  ( -35.50000000000000711, -112.0209493036498287, 0.9959249592223760050 ) ) ;
#23131 = CIRCLE ( 'NONE', #7613, 20.00000000000000711 ) ;
#23133 = DIRECTION ( 'NONE',  ( 0.1305261922200496583, 0.9914448613738107152, -1.707538432754661574E-31 ) ) ;
#23134 = DIRECTION ( 'NONE',  ( 0.000000000000000000, -0.9980267284282708928, -0.06279051952932436509 ) ) ;
#23135 = EDGE_CURVE ( 'NONE', #1926, #14743, #13397, .T. ) ;
#23136 = CARTESIAN_POINT ( 'NONE',  ( 0.000000000000000000, -15.17386234660370370, -15.92965478239635679 ) ) ;
#23137 = DIRECTION ( 'NONE',  ( -1.000000000000000000, 0.000000000000000000, 0.000000000000000000 ) ) ;
#23138 = DIRECTION ( 'NONE',  ( -1.000000000000000000, 0.000000000000000000, 0.000000000000000000 ) ) ;
#23139 = EDGE_CURVE ( 'NONE', #26512, #23627, #15869, .T. ) ;
#23140 = DIRECTION ( 'NONE',  ( 0.000000000000000000, -1.000000000000000000, 0.000000000000000000 ) ) ;
#23141 = CARTESIAN_POINT ( 'NONE',  ( 70.00000000000001421, 46.66021779527611102, 66.80632251401318911 ) ) ;
#23142 = ORIENTED_EDGE ( 'NONE', *, *, #18723, .T. ) ;
#23143 = EDGE_CURVE ( 'NONE', #2115, #23114, #20841, .T. ) ;
#23144 = CARTESIAN_POINT ( 'NONE',  ( -36.64504884055821776, -112.9754527089670688, 9.715225545821551734 ) ) ;
#23145 = DIRECTION ( 'NONE',  ( 0.000000000000000000, 0.000000000000000000, 1.000000000000000000 ) ) ;
#23146 = CARTESIAN_POINT ( 'NONE',  ( 7.999999999999992895, 43.83938735307269496, 18.28286404005814703 ) ) ;
#23147 = EDGE_LOOP ( 'NONE', ( #1846, #7690, #32495, #22270 ) ) ;
#23148 = ORIENTED_EDGE ( 'NONE', *, *, #230, .T. ) ;
#23149 = AXIS2_PLACEMENT_3D ( 'NONE', #19697, #17007, #28017 ) ;
#23150 =( NAMED_UNIT ( * ) SI_UNIT ( $, .STERADIAN. ) SOLID_ANGLE_UNIT ( ) );
#23151 = DIRECTION ( 'NONE',  ( -1.000000000000000000, 0.000000000000000000, 0.000000000000000000 ) ) ;
#23152 = ORIENTED_EDGE ( 'NONE', *, *, #29343, .F. ) ;
#23153 = ADVANCED_FACE ( 'NONE', ( #32277 ), #29935, .T. ) ;
#23154 = CARTESIAN_POINT ( 'NONE',  ( -39.97545270896702618, -115.3019030900506152, 9.152725545821551734 ) ) ;
#23155 = EDGE_CURVE ( 'NONE', #2210, #33416, #27768, .T. ) ;
#23156 = VERTEX_POINT ( 'NONE', #10489 ) ;
#23157 = LINE ( 'NONE', #23516, #18 ) ;
#23158 = CARTESIAN_POINT ( 'NONE',  ( -36.49999999999999289, -11.52052244843579309, 112.1848168619253840 ) ) ;
#23159 = AXIS2_PLACEMENT_3D ( 'NONE', #18625, #35210, #2620 ) ;
#23160 = DIRECTION ( 'NONE',  ( 1.000000000000000000, -0.000000000000000000, -0.000000000000000000 ) ) ;
#23161 = VECTOR ( 'NONE', #34752, 1000.000000000000000 ) ;
#23162 = DIRECTION ( 'NONE',  ( -1.783119874454246424E-31, -1.187911941725854497E-31, 1.000000000000000000 ) ) ;
#23163 = VECTOR ( 'NONE', #17338, 1000.000000000000000 ) ;
#23164 = APPLICATION_PROTOCOL_DEFINITION ( 'draft international standard', 'automotive_design', 1998, #16306 ) ;
#23165 = EDGE_CURVE ( 'NONE', #32375, #15577, #12236, .T. ) ;
#23166 = CARTESIAN_POINT ( 'NONE',  ( 0.000000000000000000, -13.24207120356955159, -14.98824707027455183 ) ) ;
#23167 = ORIENTED_EDGE ( 'NONE', *, *, #23998, .F. ) ;
#23168 = ORIENTED_EDGE ( 'NONE', *, *, #12552, .F. ) ;
#23169 = CARTESIAN_POINT ( 'NONE',  ( 70.00001200000001234, -28.43894899343287364, 88.19866736959266973 ) ) ;
#23170 = CARTESIAN_POINT ( 'NONE',  ( 8.000000000000007105, -9.604183132802312173, -1.108880290975637228 ) ) ;
#23171 = ORIENTED_EDGE ( 'NONE', *, *, #12100, .F. ) ;
#23172 = CARTESIAN_POINT ( 'NONE',  ( -34.49999999999998579, -21.98076211353320630, 84.99999999999994316 ) ) ;
#23173 = AXIS2_PLACEMENT_3D ( 'NONE', #6258, #22619, #33612 ) ;
#23174 = CARTESIAN_POINT ( 'NONE',  ( -34.50000000000000000, -115.0140978167138712, -0.6247823525984403936 ) ) ;
#23175 = DIRECTION ( 'NONE',  ( -1.000000000000000000, 0.000000000000000000, 0.000000000000000000 ) ) ;
#23176 = DIRECTION ( 'NONE',  ( 0.000000000000000000, 0.000000000000000000, 1.000000000000000000 ) ) ;
#23177 = CARTESIAN_POINT ( 'NONE',  ( -34.50000000000000000, -114.3049001878960240, 8.530677542735578101 ) ) ;
#23178 = CIRCLE ( 'NONE', #10544, 4.980000000000017302 ) ;
#23179 = DIRECTION ( 'NONE',  ( -1.000000000000000000, 0.000000000000000000, 0.000000000000000000 ) ) ;
#23180 = CARTESIAN_POINT ( 'NONE',  ( -38.37230871539094323, -112.5438815906447729, 2.441024454178448710 ) ) ;
#23181 = CARTESIAN_POINT ( 'NONE',  ( -37.69578139638701941, -114.9929510916434339, 14.10650203519847778 ) ) ;
#23182 = DIRECTION ( 'NONE',  ( -1.000000000000000000, 0.000000000000000000, 0.000000000000000000 ) ) ;
#23183 = ADVANCED_FACE ( 'NONE', ( #7596 ), #16214, .T. ) ;
#23184 = DIRECTION ( 'NONE',  ( 0.000000000000000000, -0.9980267284282708928, -0.06279051952932447611 ) ) ;
#23185 = LINE ( 'NONE', #34180, #4973 ) ;
#23186 = CARTESIAN_POINT ( 'NONE',  ( 0.000000000000000000, 7.162210897276456656, -51.50439529848821252 ) ) ;
#23187 = EDGE_CURVE ( 'NONE', #10728, #28744, #2235, .T. ) ;
#23188 = AXIS2_PLACEMENT_3D ( 'NONE', #24355, #16215, #2765 ) ;
#23189 = CIRCLE ( 'NONE', #1931, 47.49900000000000944 ) ;
#23190 = DIRECTION ( 'NONE',  ( -1.000000000000000000, 0.000000000000000000, 0.000000000000000000 ) ) ;
#23191 = ORIENTED_EDGE ( 'NONE', *, *, #34578, .T. ) ;
#23192 = CARTESIAN_POINT ( 'NONE',  ( -39.16322519054178741, -111.9205845034225177, 4.933975545821551734 ) ) ;
#23193 = DIRECTION ( 'NONE',  ( 0.000000000000000000, 0.000000000000000000, -1.000000000000000000 ) ) ;
#23194 = CARTESIAN_POINT ( 'NONE',  ( -35.50000000000000000, -113.0140978167138712, -0.5622823525984297355 ) ) ;
#23195 = ORIENTED_EDGE ( 'NONE', *, *, #26677, .T. ) ;
#23196 = ORIENTED_EDGE ( 'NONE', *, *, #29138, .F. ) ;
#23197 = CARTESIAN_POINT ( 'NONE',  ( 8.000000000000000000, -14.71414642875948608, -9.471478019455300768 ) ) ;
#23198 = DIRECTION ( 'NONE',  ( -1.000000000000000000, 0.000000000000000000, 0.000000000000000000 ) ) ;
#23199 = ORIENTED_EDGE ( 'NONE', *, *, #28778, .T. ) ;
#23200 = ADVANCED_FACE ( 'NONE', ( #24531, #35520 ), #18758, .T. ) ;
#23201 = VERTEX_POINT ( 'NONE', #21812 ) ;
#23202 = EDGE_CURVE ( 'NONE', #27071, #2828, #10513, .T. ) ;
#23203 = AXIS2_PLACEMENT_3D ( 'NONE', #13112, #6970, #27971 ) ;
#23204 = DIRECTION ( 'NONE',  ( -1.000000000000000000, 0.000000000000000000, 0.000000000000000000 ) ) ;
#23205 = CARTESIAN_POINT ( 'NONE',  ( -38.99999999999999289, -114.0592624029313242, 6.246475545821550845 ) ) ;
#23206 = CARTESIAN_POINT ( 'NONE',  ( 0.000000000000000000, 0.000000000000000000, 0.000000000000000000 ) ) ;
#23207 = DIRECTION ( 'NONE',  ( 1.000000000000000000, -0.000000000000000000, -0.000000000000000000 ) ) ;
#23208 = ORIENTED_EDGE ( 'NONE', *, *, #35495, .F. ) ;
#23209 = VERTEX_POINT ( 'NONE', #34742 ) ;
#23210 = CARTESIAN_POINT ( 'NONE',  ( -35.50000000000000000, -112.0066700803175763, -2.372276521656937920 ) ) ;
#23211 = VECTOR ( 'NONE', #13515, 1000.000000000000000 ) ;
#23212 = AXIS2_PLACEMENT_3D ( 'NONE', #35033, #21485, #7285 ) ;
#23213 = DIRECTION ( 'NONE',  ( -1.000000000000000000, 0.000000000000000000, 0.000000000000000000 ) ) ;
#23214 = UNCERTAINTY_MEASURE_WITH_UNIT (LENGTH_MEASURE( 1.000000000000000082E-05 ), #13706, 'distance_accuracy_value', 'NONE');
#23215 = CARTESIAN_POINT ( 'NONE',  ( 4.000000000000003553, -46.77034588191320097, 22.72740077717213936 ) ) ;
#23216 = VERTEX_POINT ( 'NONE', #4859 ) ;
#23217 = CARTESIAN_POINT ( 'NONE',  ( -37.56526046546250086, -114.9929510916434339, 13.11451721564129258 ) ) ;
#23218 = CARTESIAN_POINT ( 'NONE',  ( -34.50000000000000000, -114.1068310684433129, 9.512752019463897923 ) ) ;
#23219 = DIRECTION ( 'NONE',  ( -1.000000000000000000, 0.000000000000000000, 0.000000000000000000 ) ) ;
#23220 = CARTESIAN_POINT ( 'NONE',  ( 55.00000000000000711, -28.31857036507964764, 80.03062855292515110 ) ) ;
#23221 = CARTESIAN_POINT ( 'NONE',  ( -38.99984940073100148, -113.9929510916434339, 12.64306614848957544 ) ) ;
#23222 = DIRECTION ( 'NONE',  ( 0.000000000000000000, 0.000000000000000000, 1.000000000000000000 ) ) ;
#23223 = CARTESIAN_POINT ( 'NONE',  ( -37.42187499999997158, -114.9929510916434339, 13.11852480586264669 ) ) ;
#23224 = CYLINDRICAL_SURFACE ( 'NONE', #26228, 13.99999999999999822 ) ;
#23225 = ORIENTED_EDGE ( 'NONE', *, *, #19126, .T. ) ;
#23226 = DIRECTION ( 'NONE',  ( 0.000000000000000000, 0.000000000000000000, 1.000000000000000000 ) ) ;
#23227 = CARTESIAN_POINT ( 'NONE',  ( 0.000000000000000000, 36.05989434073613609, 30.12041790338630776 ) ) ;
#23228 = EDGE_CURVE ( 'NONE', #29583, #3694, #1798, .T. ) ;
#23229 = ORIENTED_EDGE ( 'NONE', *, *, #2694, .F. ) ;
#23230 = CARTESIAN_POINT ( 'NONE',  ( -35.50000000000000711, -114.9929510916434339, 11.21034663311131929 ) ) ;
#23231 = ORIENTED_EDGE ( 'NONE', *, *, #6659, .F. ) ;
#23232 = CARTESIAN_POINT ( 'NONE',  ( -38.99999999999999289, -113.9407375970686900, 2.253524454178449155 ) ) ;
#23233 = ORIENTED_EDGE ( 'NONE', *, *, #15817, .T. ) ;
#23234 = DIRECTION ( 'NONE',  ( 0.000000000000000000, 0.000000000000000000, 1.000000000000000000 ) ) ;
#23235 = EDGE_LOOP ( 'NONE', ( #33844, #17288, #25606, #22656 ) ) ;
#23236 = CIRCLE ( 'NONE', #30135, 20.00000000000000355 ) ;
#23237 = AXIS2_PLACEMENT_3D ( 'NONE', #34759, #20328, #10082 ) ;
#23238 = CARTESIAN_POINT ( 'NONE',  ( -34.50000000000000000, -113.0140978167137717, 0.8903425666012282358 ) ) ;
#23239 = CYLINDRICAL_SURFACE ( 'NONE', #646, 4.800000000000000711 ) ;
#23240 = CARTESIAN_POINT ( 'NONE',  ( 0.000000000000000000, -10.62435788049451624, 13.16139124467916588 ) ) ;
#23241 = ORIENTED_EDGE ( 'NONE', *, *, #8821, .F. ) ;
#23242 = CARTESIAN_POINT ( 'NONE',  ( -35.54388159064475872, -112.6276912846090568, 2.816024454178448710 ) ) ;
#23243 = DIRECTION ( 'NONE',  ( 0.000000000000000000, 1.000000000000000000, 0.000000000000000000 ) ) ;
#23244 = CARTESIAN_POINT ( 'NONE',  ( -35.50000000000000711, -112.0140978167138712, -0.3122823525984337878 ) ) ;
#23245 = ORIENTED_EDGE ( 'NONE', *, *, #11507, .T. ) ;
#23246 = ORIENTED_EDGE ( 'NONE', *, *, #9991, .T. ) ;
#23247 = CARTESIAN_POINT ( 'NONE',  ( 7.999999999999992895, -11.90021268425586953, 45.45261810511210143 ) ) ;
#23248 =( NAMED_UNIT ( * ) SI_UNIT ( $, .STERADIAN. ) SOLID_ANGLE_UNIT ( ) );
#23249 = CARTESIAN_POINT ( 'NONE',  ( 0.000000000000000000, 0.000000000000000000, 0.000000000000000000 ) ) ;
#23250 = VERTEX_POINT ( 'NONE', #29344 ) ;
#23251 = ORIENTED_EDGE ( 'NONE', *, *, #1289, .F. ) ;
#23252 = CARTESIAN_POINT ( 'NONE',  ( -34.50000000000000000, -112.8835768857893527, -1.616767172155725740 ) ) ;
#23253 = CARTESIAN_POINT ( 'NONE',  ( -35.50000000000000711, -112.7765286249690035, 1.847058736912741583 ) ) ;
#23254 = ORIENTED_EDGE ( 'NONE', *, *, #27033, .F. ) ;
#23255 = VERTEX_POINT ( 'NONE', #26104 ) ;
#23256 = CARTESIAN_POINT ( 'NONE',  ( 8.000000000000007105, 0.000000000000000000, 0.000000000000000000 ) ) ;
#23257 = CARTESIAN_POINT ( 'NONE',  ( -37.99899697755054717, -113.9929510916434339, 12.65121853911336913 ) ) ;
#23258 = AXIS2_PLACEMENT_3D ( 'NONE', #28418, #9147, #14714 ) ;
#23259 = DIRECTION ( 'NONE',  ( -1.000000000000000000, 0.000000000000000000, 0.000000000000000000 ) ) ;
#23260 = CARTESIAN_POINT ( 'NONE',  ( -36.07812499999994316, -113.9929510916434339, 13.11852480586264846 ) ) ;
#23261 = AXIS2_PLACEMENT_3D ( 'NONE', #16007, #2367, #20869 ) ;
#23262 = CARTESIAN_POINT ( 'NONE',  ( -35.50000000000000000, -115.9056129652226872, 9.909279992139808257 ) ) ;
#23263 = DIRECTION ( 'NONE',  ( 1.000000000000000000, -0.000000000000000000, -0.000000000000000000 ) ) ;
#23264 = DIRECTION ( 'NONE',  ( 0.000000000000000000, 0.000000000000000000, -1.000000000000000000 ) ) ;
#23265 = ADVANCED_FACE ( 'NONE', ( #23939 ), #7373, .F. ) ;
#23266 = CARTESIAN_POINT ( 'NONE',  ( 8.000000000000000000, 6.336799421340039373, -16.31134495048478428 ) ) ;
#23267 = DIRECTION ( 'NONE',  ( -1.000000000000000000, 0.000000000000000000, 0.000000000000000000 ) ) ;
#23268 = CARTESIAN_POINT ( 'NONE',  ( 4.000000000000000000, 4.898587196589412829E-16, 65.00000000000000000 ) ) ;
#23269 = ORIENTED_EDGE ( 'NONE', *, *, #13467, .T. ) ;
#23270 = CARTESIAN_POINT ( 'NONE',  ( 8.000000000000000000, -16.71027810728551799, 2.620268201065888203 ) ) ;
#23271 = CARTESIAN_POINT ( 'NONE',  ( -35.50000000000000711, -112.0221129971568104, -0.7553032835231431319 ) ) ;
#23272 = FACE_BOUND ( 'NONE', #26132, .T. ) ;
#23273 = CONTEXT_DEPENDENT_SHAPE_REPRESENTATION ( #11971, #9515 ) ;
#23274 = EDGE_CURVE ( 'NONE', #15107, #26850, #35252, .T. ) ;
#23275 = CARTESIAN_POINT ( 'NONE',  ( -35.50000000000000711, -114.8847986568751907, 10.03799953695244618 ) ) ;
#23276 = CARTESIAN_POINT ( 'NONE',  ( 0.000000000000000000, 0.000000000000000000, -0.7999999999999951594 ) ) ;
#23277 = ORIENTED_EDGE ( 'NONE', *, *, #25698, .T. ) ;
#23278 = CLOSED_SHELL ( 'NONE', ( #29282, #12587, #1298, #15166, #27967, #7790, #16534, #13405 ) ) ;
#23279 = DIRECTION ( 'NONE',  ( 0.000000000000000000, 0.000000000000000000, -1.000000000000000000 ) ) ;
#23280 = AXIS2_PLACEMENT_3D ( 'NONE', #16491, #32896, #24795 ) ;
#23281 = CARTESIAN_POINT ( 'NONE',  ( -34.50000000000000000, -113.3474311500483935, -2.624782352598442614 ) ) ;
#23282 = CARTESIAN_POINT ( 'NONE',  ( -21.15833593587365513, -12.00833024919776371, 94.79903810567661537 ) ) ;
#23283 = ORIENTED_EDGE ( 'NONE', *, *, #25562, .T. ) ;
#23284 = ORIENTED_EDGE ( 'NONE', *, *, #9986, .T. ) ;
#23285 = CARTESIAN_POINT ( 'NONE',  ( -37.97545270896701908, -113.5265240346955977, 3.847274454178448710 ) ) ;
#23286 = VERTEX_POINT ( 'NONE', #7181 ) ;
#23287 = AXIS2_PLACEMENT_3D ( 'NONE', #9114, #25332, #6410 ) ;
#23288 = SURFACE_STYLE_USAGE ( .BOTH. , #26008 ) ;
#23289 = ORIENTED_EDGE ( 'NONE', *, *, #27271, .T. ) ;
#23290 = ORIENTED_EDGE ( 'NONE', *, *, #17786, .F. ) ;
#23291 = CARTESIAN_POINT ( 'NONE',  ( -34.50000000000000000, -113.4742757288593964, 0.9301473394660054739 ) ) ;
#23292 = VECTOR ( 'NONE', #32465, 1000.000000000000000 ) ;
#23293 = CARTESIAN_POINT ( 'NONE',  ( 0.000000000000000000, -16.71027810728550733, 4.579731798933884157 ) ) ;
#23294 = EDGE_CURVE ( 'NONE', #3630, #27872, #32036, .T. ) ;
#23295 = CYLINDRICAL_SURFACE ( 'NONE', #27170, 17.49900000000000233 ) ;
#23296 = VECTOR ( 'NONE', #28992, 1000.000000000000114 ) ;
#23297 = CARTESIAN_POINT ( 'NONE',  ( -35.99181955245763476, -114.9929510916434339, 13.11847460610632687 ) ) ;
#23298 = FACE_OUTER_BOUND ( 'NONE', #246, .T. ) ;
#23299 = LINE ( 'NONE', #2034, #10250 ) ;
#23300 = CARTESIAN_POINT ( 'NONE',  ( -36.12500000000014211, -114.9929510916434339, 14.11852480586264846 ) ) ;
#23301 = CARTESIAN_POINT ( 'NONE',  ( -34.49999999999998579, -25.27980021920980036, 80.78589838486217900 ) ) ;
#23302 = EDGE_CURVE ( 'NONE', #19237, #15405, #25477, .T. ) ;
#23303 = PRODUCT_DEFINITION_SHAPE ( 'NONE', 'NONE',  #30188 ) ;
#23304 = CIRCLE ( 'NONE', #11240, 20.00000000000000355 ) ;
#23305 = EDGE_CURVE ( 'NONE', #25051, #28212, #2486, .T. ) ;
#23306 = CARTESIAN_POINT ( 'NONE',  ( 8.000000000000000000, -11.19999565274257414, 10.71350075272070512 ) ) ;
#23307 = ORIENTED_EDGE ( 'NONE', *, *, #29426, .T. ) ;
#23308 = EDGE_CURVE ( 'NONE', #27224, #31131, #1895, .T. ) ;
#23309 = CARTESIAN_POINT ( 'NONE',  ( -35.50000000000000000, -115.9929510916434481, 11.91443571948720148 ) ) ;
#23310 = CARTESIAN_POINT ( 'NONE',  ( -35.50000000000000711, -113.0974311500471714, -1.624782352598427959 ) ) ;
#23311 = PLANE ( 'NONE',  #32487 ) ;
#23312 = AXIS2_PLACEMENT_3D ( 'NONE', #26580, #20964, #12892 ) ;
#23313 = DIRECTION ( 'NONE',  ( -1.000000000000000000, 0.000000000000000000, 0.000000000000000000 ) ) ;
#23314 = DIRECTION ( 'NONE',  ( 1.000000000000000000, -5.339440136655842133E-16, -1.047965281155519420E-16 ) ) ;
#23315 = DIRECTION ( 'NONE',  ( 0.000000000000000000, 0.000000000000000000, -1.000000000000000000 ) ) ;
#23316 = AXIS2_PLACEMENT_3D ( 'NONE', #16776, #14601, #30826 ) ;
#23317 = CARTESIAN_POINT ( 'NONE',  ( 0.000000000000000000, -42.03146605346803000, 22.12489237027305577 ) ) ;
#23318 = DIRECTION ( 'NONE',  ( 0.000000000000000000, 0.5735764363510502672, -0.8191520442889889120 ) ) ;
#23319 = ORIENTED_EDGE ( 'NONE', *, *, #3122, .T. ) ;
#23320 = EDGE_CURVE ( 'NONE', #10552, #25051, #8216, .T. ) ;
#23321 = CARTESIAN_POINT ( 'NONE',  ( -36.02454729103297382, -113.5265240346956261, 8.402725545821549957 ) ) ;
#23322 = DIRECTION ( 'NONE',  ( 0.000000000000000000, 0.000000000000000000, 1.000000000000000000 ) ) ;
#23323 = DIRECTION ( 'NONE',  ( -1.783119874454246424E-31, -1.187911941725854497E-31, 1.000000000000000000 ) ) ;
#23324 = ADVANCED_FACE ( 'NONE', ( #15623 ), #10258, .T. ) ;
#23325 = ORIENTED_EDGE ( 'NONE', *, *, #143, .F. ) ;
#23326 = AXIS2_PLACEMENT_3D ( 'NONE', #11840, #22823, #14362 ) ;
#23327 = ORIENTED_EDGE ( 'NONE', *, *, #5817, .T. ) ;
#23328 = DIRECTION ( 'NONE',  ( 0.000000000000000000, 0.5000000000000092149, -0.8660254037844333785 ) ) ;
#23329 = CARTESIAN_POINT ( 'NONE',  ( 8.000000000000000000, -3.678165988948685516, 15.05623113391066070 ) ) ;
#23330 = ORIENTED_EDGE ( 'NONE', *, *, #16687, .F. ) ;
#23331 = CARTESIAN_POINT ( 'NONE',  ( -34.92058450342249643, -111.8367748094582197, 8.308975545821549957 ) ) ;
#23332 = ORIENTED_EDGE ( 'NONE', *, *, #18476, .F. ) ;
#23333 = DIRECTION ( 'NONE',  ( 0.000000000000000000, 0.000000000000000000, -1.000000000000000000 ) ) ;
#23334 = CARTESIAN_POINT ( 'NONE',  ( 4.000000000000003553, 30.03615769709734451, 42.44795908869000556 ) ) ;
#23335 = AXIS2_PLACEMENT_3D ( 'NONE', #30856, #14990, #17153 ) ;
#23336 = FACE_OUTER_BOUND ( 'NONE', #30401, .T. ) ;
#23337 = AXIS2_PLACEMENT_3D ( 'NONE', #22197, #25631, #958 ) ;
#23338 = ADVANCED_FACE ( 'NONE', ( #1977, #29168 ), #34933, .T. ) ;
#23339 = DIRECTION ( 'NONE',  ( -1.000000000000000000, 0.000000000000000000, 0.000000000000000000 ) ) ;
#23340 = EDGE_LOOP ( 'NONE', ( #31159, #26178, #34976, #23045 ) ) ;
#23341 = ORIENTED_EDGE ( 'NONE', *, *, #17002, .T. ) ;
#23342 = AXIS2_PLACEMENT_3D ( 'NONE', #34681, #25689, #29097 ) ;
#23343 = CARTESIAN_POINT ( 'NONE',  ( 70.00001200000001234, -27.99523803501680419, 88.49514555341693267 ) ) ;
#23344 = PRODUCT_RELATED_PRODUCT_CATEGORY ( 'part', '', ( #7526 ) ) ;
#23345 = DIRECTION ( 'NONE',  ( -1.000000000000000000, 1.110223024625156540E-16, 0.000000000000000000 ) ) ;
#23346 = VERTEX_POINT ( 'NONE', #32213 ) ;
#23347 = CARTESIAN_POINT ( 'NONE',  ( -34.49999999999998579, -14.60640646055094649, 76.70096189432339884 ) ) ;
#23348 = CIRCLE ( 'NONE', #25656, 15.49899999999998457 ) ;
#23349 = VECTOR ( 'NONE', #13806, 1000.000000000000000 ) ;
#23350 = DIRECTION ( 'NONE',  ( -1.783119874454246424E-31, -1.187911941725854497E-31, 1.000000000000000000 ) ) ;
#23351 = DIRECTION ( 'NONE',  ( 1.000000000000000000, 0.000000000000000000, -0.000000000000000000 ) ) ;
#23352 = CARTESIAN_POINT ( 'NONE',  ( -36.24999999999983658, -115.9929510916434481, 14.11852480586265024 ) ) ;
#23353 = EDGE_CURVE ( 'NONE', #14392, #1785, #9375, .T. ) ;
#23354 = EDGE_CURVE ( 'NONE', #10620, #28254, #4326, .T. ) ;
#23355 = DIRECTION ( 'NONE',  ( 0.000000000000000000, 0.000000000000000000, -1.000000000000000000 ) ) ;
#23356 = PLANE ( 'NONE',  #8231 ) ;
#23357 = EDGE_CURVE ( 'NONE', #1299, #31574, #5935, .T. ) ;
#23358 = CARTESIAN_POINT ( 'NONE',  ( -37.74437085908087397, -114.9929510916434339, 14.09929883582536903 ) ) ;
#23359 = CARTESIAN_POINT ( 'NONE',  ( 4.000000000000003553, 3.975523202428013381, 13.42368113696675103 ) ) ;
#23360 = DIRECTION ( 'NONE',  ( 0.000000000000000000, 1.000000000000000000, -1.067522139062650474E-15 ) ) ;
#23361 = AXIS2_PLACEMENT_3D ( 'NONE', #32049, #29182, #23766 ) ;
#23362 = CARTESIAN_POINT ( 'NONE',  ( 7.999999999999992895, 27.79676263918186052, 37.88001506494778425 ) ) ;
#23363 = CARTESIAN_POINT ( 'NONE',  ( 1.110223024625156540E-13, -1.000000000000042633, -40.00000000000000000 ) ) ;
#23364 = VECTOR ( 'NONE', #381, 1000.000000000000000 ) ;
#23365 = CARTESIAN_POINT ( 'NONE',  ( 0.000000000000000000, 30.93515269692114344, 36.04401931830264516 ) ) ;
#23366 = ORIENTED_EDGE ( 'NONE', *, *, #522, .T. ) ;
#23367 = CARTESIAN_POINT ( 'NONE',  ( -35.69809690994938478, -111.0245472910330022, 8.722274454178450043 ) ) ;
#23368 = AXIS2_PLACEMENT_3D ( 'NONE', #11541, #22507, #9006 ) ;
#23369 = CARTESIAN_POINT ( 'NONE',  ( 8.000000000000000000, -3.678165988948487009, -15.05623113391071044 ) ) ;
#23370 = CARTESIAN_POINT ( 'NONE',  ( -35.50000000000000000, -113.0140978167140702, 0.8752176474015694874 ) ) ;
#23371 = ADVANCED_FACE ( 'NONE', ( #12411 ), #15800, .T. ) ;
#23372 = ORIENTED_EDGE ( 'NONE', *, *, #22649, .F. ) ;
#23373 = ORIENTED_EDGE ( 'NONE', *, *, #31919, .T. ) ;
#23374 = AXIS2_PLACEMENT_3D ( 'NONE', #15345, #17333, #11956 ) ;
#23375 = CARTESIAN_POINT ( 'NONE',  ( 0.000000000000000000, 0.000000000000000000, 35.10000000000000142 ) ) ;
#23376 = DIRECTION ( 'NONE',  ( -1.783119874454246424E-31, -1.187911941725854497E-31, 1.000000000000000000 ) ) ;
#23377 = ORIENTED_EDGE ( 'NONE', *, *, #6366, .T. ) ;
#23378 = AXIS2_PLACEMENT_3D ( 'NONE', #4255, #23500, #29445 ) ;
#23379 = VERTEX_POINT ( 'NONE', #23572 ) ;
#23382 = ADVANCED_FACE ( 'NONE', ( #23396 ), #15091, .T. ) ;
#23381 = VERTEX_POINT ( 'NONE', #31506 ) ;
#23380 = VECTOR ( 'NONE', #11726, 1000.000000000000000 ) ;
#23383 = CIRCLE ( 'NONE', #2162, 52.00000000000000711 ) ;
#23384 = DIRECTION ( 'NONE',  ( 1.000000000000000000, -0.000000000000000000, -0.000000000000000000 ) ) ;
#23385 = CARTESIAN_POINT ( 'NONE',  ( -35.62769128460905677, -112.5438815906447729, 3.808975545821551290 ) ) ;
#23386 = DIRECTION ( 'NONE',  ( 0.000000000000000000, -0.9999978841041035071, 0.002057130845644337871 ) ) ;
#23387 = AXIS2_PLACEMENT_3D ( 'NONE', #2091, #31776, #23134 ) ;
#23388 = EDGE_CURVE ( 'NONE', #7932, #7369, #24349, .T. ) ;
#23389 = CARTESIAN_POINT ( 'NONE',  ( 0.000000000000000000, 0.000000000000000000, 60.00000000000000000 ) ) ;
#23390 = CIRCLE ( 'NONE', #31438, 20.00000000000000711 ) ;
#23391 = ORIENTED_EDGE ( 'NONE', *, *, #31320, .T. ) ;
#23392 = ORIENTED_EDGE ( 'NONE', *, *, #29524, .F. ) ;
#23393 = CARTESIAN_POINT ( 'NONE',  ( -35.50000000000000000, -117.0140978167138854, -0.3747823525984422255 ) ) ;
#23394 = CIRCLE ( 'NONE', #8459, 8.000000000000003553 ) ;
#23395 = EDGE_CURVE ( 'NONE', #14544, #26283, #20871, .T. ) ;
#23396 = FACE_OUTER_BOUND ( 'NONE', #30637, .T. ) ;
#23397 = CARTESIAN_POINT ( 'NONE',  ( 55.00000000000000000, 20.00000000000001776, 110.0000000000000000 ) ) ;
#23398 = ORIENTED_EDGE ( 'NONE', *, *, #17035, .T. ) ;
#23399 = CARTESIAN_POINT ( 'NONE',  ( -38.00000000000000711, -114.9929510916434339, 12.59102132592608925 ) ) ;
#23400 = AXIS2_PLACEMENT_3D ( 'NONE', #15877, #5286, #26902 ) ;
#23401 = CARTESIAN_POINT ( 'NONE',  ( -34.50000000000000000, -114.4026847875275337, 9.592046023459676718 ) ) ;
#23402 = CIRCLE ( 'NONE', #27457, 14.00000000000000000 ) ;
#23403 = CARTESIAN_POINT ( 'NONE',  ( 0.000000000000000000, -46.19362259308826424, -8.585149169758999221 ) ) ;
#23404 = ADVANCED_FACE ( 'NONE', ( #2345 ), #24466, .T. ) ;
#23405 = CARTESIAN_POINT ( 'NONE',  ( -37.43749999999998579, -114.9929510916434339, 13.11852480586264669 ) ) ;
#23406 = DIRECTION ( 'NONE',  ( -1.000000000000000000, 0.000000000000000000, -0.000000000000000000 ) ) ;
#23407 = ADVANCED_FACE ( 'NONE', ( #27177 ), #30405, .F. ) ;
#23408 = CARTESIAN_POINT ( 'NONE',  ( -37.43749999999998579, -113.9929510916434339, 14.11852480586265024 ) ) ;
#23409 = DIRECTION ( 'NONE',  ( 0.000000000000000000, 0.000000000000000000, -1.000000000000000000 ) ) ;
#23410 = CARTESIAN_POINT ( 'NONE',  ( -37.46874999999996447, -114.9929510916434339, 13.11852480586264669 ) ) ;
#23411 = PLANE ( 'NONE',  #13059 ) ;
#23412 = ORIENTED_EDGE ( 'NONE', *, *, #20765, .F. ) ;
#23413 = DIRECTION ( 'NONE',  ( -1.000000000000000000, -0.000000000000000000, -0.000000000000000000 ) ) ;
#23414 = DIRECTION ( 'NONE',  ( 0.000000000000000000, 0.000000000000000000, -1.000000000000000000 ) ) ;
#23415 = ORIENTED_EDGE ( 'NONE', *, *, #30599, .F. ) ;
#23416 = CARTESIAN_POINT ( 'NONE',  ( -35.60016694755736921, -114.9929510916434339, 12.92579853460621209 ) ) ;
#23417 = ORIENTED_EDGE ( 'NONE', *, *, #34979, .T. ) ;
#23418 = DIRECTION ( 'NONE',  ( 0.000000000000000000, 0.000000000000000000, -1.000000000000000000 ) ) ;
#23419 = CIRCLE ( 'NONE', #29753, 9.499000000000007660 ) ;
#23420 = EDGE_LOOP ( 'NONE', ( #20060, #27179, #26026, #2334 ) ) ;
#23421 = DIRECTION ( 'NONE',  ( 1.226634733346697831E-16, -0.2588190451025308425, 0.9659258262890655367 ) ) ;
#23422 = ORIENTED_EDGE ( 'NONE', *, *, #33233, .F. ) ;
#23423 = AXIS2_PLACEMENT_3D ( 'NONE', #1578, #12372, #9843 ) ;
#23424 = CARTESIAN_POINT ( 'NONE',  ( -34.50000000000000000, -113.0140978167138712, -0.5622823525984297355 ) ) ;
#23425 = CARTESIAN_POINT ( 'NONE',  ( 0.000000000000000000, 0.000000000000000000, 4.000000000000000000 ) ) ;
#23426 = CARTESIAN_POINT ( 'NONE',  ( -39.49999999999999289, -15.63316754279159326, 121.0048025873809792 ) ) ;
#23427 = ORIENTED_EDGE ( 'NONE', *, *, #21998, .F. ) ;
#23428 = CARTESIAN_POINT ( 'NONE',  ( -38.45611840935523418, -115.3723087153909432, 3.566024454178448710 ) ) ;
#23429 = AXIS2_PLACEMENT_3D ( 'NONE', #29483, #23899, #12913 ) ;
#23430 = AXIS2_PLACEMENT_3D ( 'NONE', #27212, #24150, #4554 ) ;
#23431 = AXIS2_PLACEMENT_3D ( 'NONE', #10294, #26860, #29735 ) ;
#23432 = DIRECTION ( 'NONE',  ( 1.000000000000000000, -0.000000000000000000, -0.000000000000000000 ) ) ;
#23433 = CARTESIAN_POINT ( 'NONE',  ( -35.50000000000000711, -115.6286452741999113, -1.424448457485488095 ) ) ;
#23434 = ORIENTED_EDGE ( 'NONE', *, *, #14323, .T. ) ;
#23435 = ORIENTED_EDGE ( 'NONE', *, *, #27132, .F. ) ;
#23436 = VECTOR ( 'NONE', #6945, 1000.000000000000000 ) ;
#23437 = CARTESIAN_POINT ( 'NONE',  ( 8.000000000000000000, -1.693188892523842082, 15.40623615209871566 ) ) ;
#23438 = CIRCLE ( 'NONE', #35534, 6.000000000000005329 ) ;
#23439 =( LENGTH_UNIT ( ) NAMED_UNIT ( * ) SI_UNIT ( .MILLI., .METRE. ) );
#23440 = EDGE_CURVE ( 'NONE', #35265, #19439, #2173, .T. ) ;
#23441 = FACE_OUTER_BOUND ( 'NONE', #1966, .T. ) ;
#23442 = VERTEX_POINT ( 'NONE', #13145 ) ;
#23443 = EDGE_LOOP ( 'NONE', ( #25350, #13044, #1496, #23325 ) ) ;
#23444 = CARTESIAN_POINT ( 'NONE',  ( -34.50000000000000000, -114.1807644833817648, -1.624782352598427959 ) ) ;
#23445 = CARTESIAN_POINT ( 'NONE',  ( -35.50000000000000711, -112.0141053790792114, 0.9054673897245171243 ) ) ;
#23446 = EDGE_CURVE ( 'NONE', #9169, #11290, #28370, .T. ) ;
#23447 = CARTESIAN_POINT ( 'NONE',  ( 0.000000000000000000, -8.128228055638727412, -16.94522934049221519 ) ) ;
#23448 = EDGE_LOOP ( 'NONE', ( #29595, #19078, #7941, #13461 ) ) ;
#23449 = ORIENTED_EDGE ( 'NONE', *, *, #7967, .T. ) ;
#23450 = DIRECTION ( 'NONE',  ( -1.000000000000000000, 0.000000000000000000, 0.000000000000000000 ) ) ;
#23451 = AXIS2_PLACEMENT_3D ( 'NONE', #34995, #32984, #5104 ) ;
#23452 = CIRCLE ( 'NONE', #19892, 5.000000000000011546 ) ;
#23453 = CARTESIAN_POINT ( 'NONE',  ( -35.52552712174883709, -113.9929510916434339, 12.77960891308624625 ) ) ;
#23454 = DIRECTION ( 'NONE',  ( 1.000000000000000000, -0.000000000000000000, -0.000000000000000000 ) ) ;
#23455 = CARTESIAN_POINT ( 'NONE',  ( -35.60016694755736211, -113.9929510916434339, 12.92579853460621386 ) ) ;
#23456 = CARTESIAN_POINT ( 'NONE',  ( -35.50000000000000000, -115.9926080209513657, 10.46845107750242398 ) ) ;
#23457 = DIRECTION ( 'NONE',  ( 0.000000000000000000, 1.000000000000000000, 0.000000000000000000 ) ) ;
#23458 = AXIS2_PLACEMENT_3D ( 'NONE', #4683, #13136, #24115 ) ;
#23459 = DIRECTION ( 'NONE',  ( 0.000000000000000000, 1.000000000000000000, 0.000000000000000000 ) ) ;
#23460 = ORIENTED_EDGE ( 'NONE', *, *, #24826, .T. ) ;
#23461 = FACE_OUTER_BOUND ( 'NONE', #33026, .T. ) ;
#23462 = DIRECTION ( 'NONE',  ( -1.000000000000000000, -0.000000000000000000, -0.000000000000000000 ) ) ;
#23463 = VECTOR ( 'NONE', #23015, 1000.000000000000227 ) ;
#23464 = CARTESIAN_POINT ( 'NONE',  ( 0.000000000000000000, -16.53603053422202862, -8.931325931664767737 ) ) ;
#23465 = ORIENTED_EDGE ( 'NONE', *, *, #9904, .T. ) ;
#23466 = CARTESIAN_POINT ( 'NONE',  ( -34.49999999999998579, -14.67619866229190784, 76.74125644078590369 ) ) ;
#23467 = CARTESIAN_POINT ( 'NONE',  ( -35.50000000000000711, -113.8474311500459777, -1.624782352598427959 ) ) ;
#23468 = LINE ( 'NONE', #6897, #20735 ) ;
#23469 = ITEM_DEFINED_TRANSFORMATION ( 'NONE', 'NONE', #11557,  #21307 ) ;
#23470 = PLANE ( 'NONE',  #30825 ) ;
#23471 = DIRECTION ( 'NONE',  ( -0.000000000000000000, 0.000000000000000000, -1.000000000000000000 ) ) ;
#23472 = EDGE_LOOP ( 'NONE', ( #34193, #34645 ) ) ;
#23473 = FACE_OUTER_BOUND ( 'NONE', #10647, .T. ) ;
#23474 = CARTESIAN_POINT ( 'NONE',  ( -34.50000000000000000, -117.0140978167138854, 0.3752176474015737617 ) ) ;
#23475 = DIRECTION ( 'NONE',  ( 1.000000000000000000, -1.110223024625156540E-16, 0.000000000000000000 ) ) ;
#23476 = ORIENTED_EDGE ( 'NONE', *, *, #28853, .T. ) ;
#23477 = VERTEX_POINT ( 'NONE', #2516 ) ;
#23478 = CARTESIAN_POINT ( 'NONE',  ( -36.64504884055823908, -115.0245472910329880, 3.284774454178449155 ) ) ;
#23479 = ORIENTED_EDGE ( 'NONE', *, *, #11474, .F. ) ;
#23480 = ORIENTED_EDGE ( 'NONE', *, *, #12177, .F. ) ;
#23481 = VECTOR ( 'NONE', #5992, 1000.000000000000000 ) ;
#23482 = CARTESIAN_POINT ( 'NONE',  ( -35.50000000000000000, -113.4307644833805142, -0.6247823525984269599 ) ) ;
#23483 = EDGE_CURVE ( 'NONE', #24879, #41, #17400, .T. ) ;
#23484 = AXIS2_PLACEMENT_3D ( 'NONE', #28382, #19894, #19719 ) ;
#23485 = PLANE ( 'NONE',  #12588 ) ;
#23486 = CARTESIAN_POINT ( 'NONE',  ( 0.000000000000000000, 41.20225022064671805, -23.63323037071357646 ) ) ;
#23487 = CARTESIAN_POINT ( 'NONE',  ( -36.87500000000098055, -114.9929510916434339, 13.11852480586264669 ) ) ;
#23488 = CARTESIAN_POINT ( 'NONE',  ( 0.000000000000000000, 0.000000000000000000, 0.000000000000000000 ) ) ;
#23489 = EDGE_CURVE ( 'NONE', #27865, #25795, #4800, .T. ) ;
#23490 = CARTESIAN_POINT ( 'NONE',  ( -34.51202277066418844, -114.9929510916434339, 12.81430620224972294 ) ) ;
#23491 = CARTESIAN_POINT ( 'NONE',  ( 7.999999999999992895, 0.000000000000000000, 0.000000000000000000 ) ) ;
#23492 = CARTESIAN_POINT ( 'NONE',  ( -3.799999999999999822, 4.382607293638566128E-16, -21.89999999999999858 ) ) ;
#23493 = ORIENTED_EDGE ( 'NONE', *, *, #15541, .F. ) ;
#23494 = AXIS2_PLACEMENT_3D ( 'NONE', #621, #31227, #5860 ) ;
#23495 = CARTESIAN_POINT ( 'NONE',  ( -36.12500000000014211, -115.9929510916434481, 13.11852480586264846 ) ) ;
#23496 = CARTESIAN_POINT ( 'NONE',  ( -35.50000000000000711, -116.0140978167138712, -0.3747823525984422255 ) ) ;
#23497 = PRESENTATION_STYLE_ASSIGNMENT (( #12520 ) ) ;
#23498 = CARTESIAN_POINT ( 'NONE',  ( 7.999999999999992895, 0.000000000000000000, 0.000000000000000000 ) ) ;
#23499 = VECTOR ( 'NONE', #29925, 1000.000000000000000 ) ;
#23500 = DIRECTION ( 'NONE',  ( 0.000000000000000000, 0.000000000000000000, -1.000000000000000000 ) ) ;
#23501 = CIRCLE ( 'NONE', #19465, 20.00000000000000711 ) ;
#23502 = CYLINDRICAL_SURFACE ( 'NONE', #24553, 8.000000000000000000 ) ;
#23503 = DIRECTION ( 'NONE',  ( -1.000000000000000000, -0.000000000000000000, -0.000000000000000000 ) ) ;
#23504 = FACE_OUTER_BOUND ( 'NONE', #11544, .T. ) ;
#23505 = DIRECTION ( 'NONE',  ( -0.000000000000000000, -0.000000000000000000, -1.000000000000000000 ) ) ;
#23506 = ORIENTED_EDGE ( 'NONE', *, *, #27315, .T. ) ;
#23507 = CARTESIAN_POINT ( 'NONE',  ( -37.47347596530441649, -113.0245472910329880, 9.527725545821551734 ) ) ;
#23508 = PLANE ( 'NONE',  #6636 ) ;
#23509 = LINE ( 'NONE', #34502, #32547 ) ;
#23510 = ORIENTED_EDGE ( 'NONE', *, *, #26040, .T. ) ;
#23511 = EDGE_LOOP ( 'NONE', ( #8511, #8241 ) ) ;
#23512 = DIRECTION ( 'NONE',  ( 0.000000000000000000, 0.000000000000000000, -1.000000000000000000 ) ) ;
#23513 = ORIENTED_EDGE ( 'NONE', *, *, #5952, .T. ) ;
#23514 = CARTESIAN_POINT ( 'NONE',  ( -38.18337828418796676, -117.0245472910329738, 7.465225545821552622 ) ) ;
#23515 = ORIENTED_EDGE ( 'NONE', *, *, #22224, .T. ) ;
#23516 = CARTESIAN_POINT ( 'NONE',  ( 4.000000000000000000, 4.898587196589412829E-16, 55.00000000000000000 ) ) ;
#23517 = ORIENTED_EDGE ( 'NONE', *, *, #30915, .F. ) ;
#23518 = DIRECTION ( 'NONE',  ( 0.000000000000000000, 0.6427876096865349220, 0.7660444431189816772 ) ) ;
#23519 = EDGE_CURVE ( 'NONE', #34652, #9372, #5733, .T. ) ;
#23520 = EDGE_CURVE ( 'NONE', #5065, #19248, #764, .T. ) ;
#23521 = DIRECTION ( 'NONE',  ( -0.000000000000000000, 0.000000000000000000, -1.000000000000000000 ) ) ;
#23522 = CIRCLE ( 'NONE', #1120, 17.49900000000001299 ) ;
#23523 = CARTESIAN_POINT ( 'NONE',  ( 0.000000000000000000, -12.46108038583301791, -15.64357617739007722 ) ) ;
#23524 = EDGE_LOOP ( 'NONE', ( #34691, #6853, #30172, #6315, #35321 ) ) ;
#23525 = VERTEX_POINT ( 'NONE', #5388 ) ;
#23526 = CIRCLE ( 'NONE', #10328, 9.499000000000000554 ) ;
#23527 = DIRECTION ( 'NONE',  ( 0.000000000000000000, -1.000000000000000000, 0.000000000000000000 ) ) ;
#23528 = CARTESIAN_POINT ( 'NONE',  ( 7.999999999999992895, -38.92705108641750655, 27.21837053747785973 ) ) ;
#23529 = ADVANCED_FACE ( 'NONE', ( #13663 ), #24909, .T. ) ;
#23531 = ORIENTED_EDGE ( 'NONE', *, *, #27539, .F. ) ;
#23530 = AXIS2_PLACEMENT_3D ( 'NONE', #18584, #13370, #18935 ) ;
#23532 = DIRECTION ( 'NONE',  ( -1.783119874454246424E-31, -1.187911941725854497E-31, 1.000000000000000000 ) ) ;
#23533 = DIRECTION ( 'NONE',  ( -1.000000000000000000, 0.000000000000000000, -0.000000000000000000 ) ) ;
#23534 = FACE_OUTER_BOUND ( 'NONE', #34045, .T. ) ;
#23535 = CARTESIAN_POINT ( 'NONE',  ( -35.93867112612154102, -115.9929510916434481, 14.11732072679899197 ) ) ;
#23536 = FACE_OUTER_BOUND ( 'NONE', #23831, .T. ) ;
#23537 = CARTESIAN_POINT ( 'NONE',  ( -35.54388159064475872, -112.6276912846090568, 2.816024454178448710 ) ) ;
#23538 = CARTESIAN_POINT ( 'NONE',  ( -34.54793860109200665, -115.9929510916434481, 13.00730889637958221 ) ) ;
#23539 = LINE ( 'NONE', #9683, #11898 ) ;
#23540 = DIRECTION ( 'NONE',  ( -1.000000000000000000, 0.000000000000000000, 0.000000000000000000 ) ) ;
#23541 = DIRECTION ( 'NONE',  ( 0.000000000000000000, 0.000000000000000000, -1.000000000000000000 ) ) ;
#23542 = CARTESIAN_POINT ( 'NONE',  ( 0.000000000000000000, 0.6505223195682995341, 51.99593080916758936 ) ) ;
#23543 = DIRECTION ( 'NONE',  ( 0.000000000000000000, -1.000000000000000000, 0.000000000000000000 ) ) ;
#23544 = FILL_AREA_STYLE_COLOUR ( '', #10354 ) ;
#23545 = ORIENTED_EDGE ( 'NONE', *, *, #32426, .T. ) ;
#23546 = AXIS2_PLACEMENT_3D ( 'NONE', #5177, #26779, #2474 ) ;
#23547 = CARTESIAN_POINT ( 'NONE',  ( -34.83677480945819838, -111.9205845034225462, 8.816024454178446490 ) ) ;
#23548 = DIRECTION ( 'NONE',  ( -1.734723475976807094E-16, 0.5000000000000092149, -0.8660254037844333785 ) ) ;
#23549 = EDGE_CURVE ( 'NONE', #2539, #5260, #5035, .T. ) ;
#23550 = CARTESIAN_POINT ( 'NONE',  ( -35.50000000000000000, -113.0140978167141128, -0.6247823525984907977 ) ) ;
#23551 = EDGE_LOOP ( 'NONE', ( #28330, #23702, #318, #27537, #5342, #12596, #15974, #21159, #2763, #28141, #24902, #20781, #15626, #12273, #21506, #29646, #30010, #15558, #17201, #11735, #9600, #20618, #29820, #23091, #19221 ) ) ;
#23552 = CIRCLE ( 'NONE', #22974, 8.000000000000007105 ) ;
#23553 = ORIENTED_EDGE ( 'NONE', *, *, #14324, .F. ) ;
#23554 = CARTESIAN_POINT ( 'NONE',  ( 115.0000000000000000, 81.48267994499606459, 25.65054357219660019 ) ) ;
#23555 = DIRECTION ( 'NONE',  ( 0.000000000000000000, 0.9048270524660175784, 0.4257792915650767673 ) ) ;
#23556 = EDGE_LOOP ( 'NONE', ( #30446, #22161 ) ) ;
#23557 = ORIENTED_EDGE ( 'NONE', *, *, #7227, .F. ) ;
#23558 = VECTOR ( 'NONE', #28374, 1000.000000000000114 ) ;
#23559 = DIRECTION ( 'NONE',  ( -6.058232658448418820E-17, -0.9730768813850325660, -0.2304807647374927382 ) ) ;
#23560 = AXIS2_PLACEMENT_3D ( 'NONE', #503, #30569, #17046 ) ;
#23561 = VERTEX_POINT ( 'NONE', #24294 ) ;
#23562 = EDGE_CURVE ( 'NONE', #33371, #19590, #31810, .T. ) ;
#23563 = CARTESIAN_POINT ( 'NONE',  ( 0.000000000000000000, 0.000000000000000000, 0.000000000000000000 ) ) ;
#23564 = ADVANCED_FACE ( 'NONE', ( #19049, #10786 ), #7890, .T. ) ;
#23565 = CARTESIAN_POINT ( 'NONE',  ( 7.999999999999992895, 46.90537658765329354, 2.727856614654466938 ) ) ;
#23566 = EDGE_CURVE ( 'NONE', #31804, #18147, #11109, .T. ) ;
#23567 = CARTESIAN_POINT ( 'NONE',  ( -22.00000000000000000, -3.306816626080788524E-15, 69.99999999999998579 ) ) ;
#23568 = CARTESIAN_POINT ( 'NONE',  ( -3.799999999999999822, 4.653657836759942730E-16, 60.00000000000000000 ) ) ;
#23569 = EDGE_LOOP ( 'NONE', ( #18941, #7776, #9388, #32494 ) ) ;
#23570 = ORIENTED_EDGE ( 'NONE', *, *, #28849, .F. ) ;
#23571 = CARTESIAN_POINT ( 'NONE',  ( -35.50000000000000000, -113.1807644833805426, -2.624782352598442614 ) ) ;
#23572 = CARTESIAN_POINT ( 'NONE',  ( -46.00000000000000000, -25.98076211353320275, 92.99999999999991473 ) ) ;
#23573 = EDGE_CURVE ( 'NONE', #11680, #16904, #18001, .T. ) ;
#23574 = DIRECTION ( 'NONE',  ( -1.000000000000000000, 0.000000000000000000, 0.000000000000000000 ) ) ;
#23575 = ORIENTED_EDGE ( 'NONE', *, *, #33158, .T. ) ;
#23576 = DIRECTION ( 'NONE',  ( 0.000000000000000000, 0.000000000000000000, -1.000000000000000000 ) ) ;
#23577 = EDGE_CURVE ( 'NONE', #31687, #26586, #35281, .T. ) ;
#23578 = CIRCLE ( 'NONE', #29915, 52.00000000000000711 ) ;
#23579 = CARTESIAN_POINT ( 'NONE',  ( -34.50000000000000000, -114.9929510916434339, 11.73841344789270202 ) ) ;
#23580 = CARTESIAN_POINT ( 'NONE',  ( 0.000000000000000000, -14.71414642875948608, -9.471478019455300768 ) ) ;
#23581 = CARTESIAN_POINT ( 'NONE',  ( -37.99359134332094357, -114.9929510916434339, 12.69998175888958158 ) ) ;
#23582 = CARTESIAN_POINT ( 'NONE',  ( -10.00000000000000000, 0.000000000000000000, 0.000000000000000000 ) ) ;
#23583 = PRESENTATION_LAYER_ASSIGNMENT (  '', '', ( #26451 ) ) ;
#23584 = VECTOR ( 'NONE', #11513, 1000.000000000000000 ) ;
#23585 = CARTESIAN_POINT ( 'NONE',  ( -34.50000000000000000, -114.8847986568751907, 10.03799953695244618 ) ) ;
#23586 = CARTESIAN_POINT ( 'NONE',  ( -4.000000000000000000, -2.710505431213761085E-17, 45.89999999999999858 ) ) ;
#23587 = CARTESIAN_POINT ( 'NONE',  ( -37.99959864031215773, -114.9929510916434339, 12.63896776382213538 ) ) ;
#23588 = CARTESIAN_POINT ( 'NONE',  ( 0.000000000000000000, 0.000000000000000000, 0.000000000000000000 ) ) ;
#23589 = ORIENTED_EDGE ( 'NONE', *, *, #31485, .T. ) ;
#23590 = CARTESIAN_POINT ( 'NONE',  ( 7.999999999999992895, 0.000000000000000000, 0.000000000000000000 ) ) ;
#23591 = DIRECTION ( 'NONE',  ( 0.000000000000000000, 0.000000000000000000, 1.000000000000000000 ) ) ;
#23592 = VERTEX_POINT ( 'NONE', #3741 ) ;
#23593 = CARTESIAN_POINT ( 'NONE',  ( -35.69272627125609176, -114.9929510916434339, 13.01835785830562209 ) ) ;
#23594 = ORIENTED_EDGE ( 'NONE', *, *, #25273, .T. ) ;
#23595 = CARTESIAN_POINT ( 'NONE',  ( 4.000000000000000000, 4.627536653468036720E-16, 54.99999999999999289 ) ) ;
#23596 = FACE_OUTER_BOUND ( 'NONE', #5070, .T. ) ;
#23597 = EDGE_CURVE ( 'NONE', #5410, #26512, #3073, .T. ) ;
#23598 = ORIENTED_EDGE ( 'NONE', *, *, #14126, .F. ) ;
#23599 = DIRECTION ( 'NONE',  ( -1.000000000000000000, -1.502314598737158292E-16, -8.673617379884052728E-17 ) ) ;
#23600 = ORIENTED_EDGE ( 'NONE', *, *, #21765, .F. ) ;
#23601 = CARTESIAN_POINT ( 'NONE',  ( -34.50000000000000000, -113.0140978167138712, -0.3747823525984258497 ) ) ;
#23602 = CARTESIAN_POINT ( 'NONE',  ( 0.000000000000000000, -13.42368113696662490, -3.975523202428152381 ) ) ;
#23603 = ADVANCED_FACE ( 'NONE', ( #31103 ), #844, .F. ) ;
#23604 = CARTESIAN_POINT ( 'NONE',  ( -35.54388159064475872, -112.6276912846090568, 8.816024454178448266 ) ) ;
#23605 = CIRCLE ( 'NONE', #12082, 52.00000000000000711 ) ;
#23606 = EDGE_CURVE ( 'NONE', #14329, #5886, #1940, .T. ) ;
#23607 = ORIENTED_EDGE ( 'NONE', *, *, #28577, .F. ) ;
#23608 = CARTESIAN_POINT ( 'NONE',  ( -34.92058450342251064, -116.1632251905417945, 3.191024454178448710 ) ) ;
#23609 = VECTOR ( 'NONE', #1058, 1000.000000000000000 ) ;
#23610 = PLANE ( 'NONE',  #33767 ) ;
#23611 = CARTESIAN_POINT ( 'NONE',  ( -35.50000000000000711, -112.1403507321855528, -1.128496220798856253 ) ) ;
#23612 = ORIENTED_EDGE ( 'NONE', *, *, #18476, .T. ) ;
#23613 = ORIENTED_EDGE ( 'NONE', *, *, #7994, .T. ) ;
#23614 = EDGE_CURVE ( 'NONE', #2022, #423, #2514, .T. ) ;
#23615 = DIRECTION ( 'NONE',  ( 0.000000000000000000, -0.4387576694191721027, 0.8986054237126862576 ) ) ;
#23616 = VECTOR ( 'NONE', #23505, 1000.000000000000000 ) ;
#23617 = COLOUR_RGB ( '', 0.09019608, 0.27058824, 0.51372549) ;
#23618 = ADVANCED_FACE ( 'NONE', ( #5901 ), #25352, .T. ) ;
#23619 = CIRCLE ( 'NONE', #28218, 4.000000000000000000 ) ;
#23620 =( NAMED_UNIT ( * ) PLANE_ANGLE_UNIT ( ) SI_UNIT ( $, .RADIAN. ) );
#23621 = CARTESIAN_POINT ( 'NONE',  ( 50.00000000000000000, 20.00000000000001776, -15.00000000000001421 ) ) ;
#23622 = ORIENTED_EDGE ( 'NONE', *, *, #28647, .T. ) ;
#23623 = ORIENTED_EDGE ( 'NONE', *, *, #22069, .F. ) ;
#23624 = CARTESIAN_POINT ( 'NONE',  ( -34.50000000000000000, -112.0651520602111191, -0.9469505670458575608 ) ) ;
#23625 = PRODUCT_DEFINITION_SHAPE ( 'NONE', 'NONE',  #6847 ) ;
#23626 = DIRECTION ( 'NONE',  ( 1.000000000000000000, 0.000000000000000000, -1.691777834109591064E-31 ) ) ;
#23627 = VERTEX_POINT ( 'NONE', #3566 ) ;
#23628 = EDGE_LOOP ( 'NONE', ( #13709, #5173 ) ) ;
#23629 = DIRECTION ( 'NONE',  ( -1.000000000000000000, 0.000000000000000000, 0.000000000000000000 ) ) ;
#23630 = ADVANCED_FACE ( 'NONE', ( #14698 ), #14513, .T. ) ;
#23631 = CARTESIAN_POINT ( 'NONE',  ( -34.50000000000000000, -113.9929510916433060, 10.50625754673589540 ) ) ;
#23632 = AXIS2_PLACEMENT_3D ( 'NONE', #11655, #26606, #4118 ) ;
#23633 = CARTESIAN_POINT ( 'NONE',  ( 1.479000000000008086, 0.000000000000000000, 0.000000000000000000 ) ) ;
#23634 = CARTESIAN_POINT ( 'NONE',  ( -35.56312645773537895, -113.9929510916434339, 12.87038173996308998 ) ) ;
#23635 = CARTESIAN_POINT ( 'NONE',  ( -37.99994980024369085, -115.9929510916434481, 12.62670525340494621 ) ) ;
#23636 = CYLINDRICAL_SURFACE ( 'NONE', #16416, 47.49900000000001654 ) ;
#23637 = FACE_OUTER_BOUND ( 'NONE', #34008, .T. ) ;
#23638 = ORIENTED_EDGE ( 'NONE', *, *, #23143, .F. ) ;
#23639 = CIRCLE ( 'NONE', #25930, 20.00000000000000711 ) ;
#23640 = CYLINDRICAL_SURFACE ( 'NONE', #16549, 52.00000000000000711 ) ;
#23641 = LINE ( 'NONE', #34628, #19684 ) ;
#23642 = VECTOR ( 'NONE', #23207, 1000.000000000000000 ) ;
#23643 = CARTESIAN_POINT ( 'NONE',  ( 50.00005079999999680, 0.000000000000000000, 0.000000000000000000 ) ) ;
#23644 = EDGE_CURVE ( 'NONE', #17290, #18475, #17045, .T. ) ;
#23645 = AXIS2_PLACEMENT_3D ( 'NONE', #15085, #23386, #6642 ) ;
#23646 = EDGE_LOOP ( 'NONE', ( #32024, #14913, #7908, #301 ) ) ;
#23647 = CARTESIAN_POINT ( 'NONE',  ( 0.000000000000000000, 3.968388925835109049, -21.63912866391136447 ) ) ;
#23648 = EDGE_CURVE ( 'NONE', #4839, #12825, #3216, .T. ) ;
#23649 = CARTESIAN_POINT ( 'NONE',  ( -35.50000000000000711, -112.0140978167138712, 0.0002176474015661141945 ) ) ;
#23650 = CYLINDRICAL_SURFACE ( 'NONE', #21884, 3.799999999999999822 ) ;
#23651 = DIRECTION ( 'NONE',  ( 1.000000000000000000, -0.000000000000000000, 0.000000000000000000 ) ) ;
#23652 = CARTESIAN_POINT ( 'NONE',  ( -35.50000000000000711, -114.1302255537607095, 9.515717283514957714 ) ) ;
#23653 = DIRECTION ( 'NONE',  ( -1.174092375852890260E-15, 4.222049128630259891E-16, 1.000000000000000000 ) ) ;
#23654 = ORIENTED_EDGE ( 'NONE', *, *, #11492, .F. ) ;
#23655 = CARTESIAN_POINT ( 'NONE',  ( 70.00000000000001421, 81.48267994499606459, 37.65054357219658243 ) ) ;
#23656 = CARTESIAN_POINT ( 'NONE',  ( -34.50000000000000000, -113.0765974847181781, -2.624803185604914102 ) ) ;
#23657 = LINE ( 'NONE', #13034, #33544 ) ;
#23658 = ORIENTED_EDGE ( 'NONE', *, *, #27618, .T. ) ;
#23659 = ORIENTED_EDGE ( 'NONE', *, *, #34721, .F. ) ;
#23660 = EDGE_CURVE ( 'NONE', #19486, #26231, #14178, .T. ) ;
#23661 = CARTESIAN_POINT ( 'NONE',  ( -36.02454729103297382, -113.5265240346956261, 8.402725545821549957 ) ) ;
#23662 = VERTEX_POINT ( 'NONE', #17222 ) ;
#23663 = VERTEX_POINT ( 'NONE', #33989 ) ;
#23664 = CARTESIAN_POINT ( 'NONE',  ( -35.50000000000000000, -115.0140978167138712, 0.8752176474015623819 ) ) ;
#23665 = CIRCLE ( 'NONE', #9848, 15.49899999999997391 ) ;
#23666 = STYLED_ITEM ( 'NONE', ( #20218 ), #6921 ) ;
#23667 = AXIS2_PLACEMENT_3D ( 'NONE', #30565, #33097, #22444 ) ;
#23668 = DIRECTION ( 'NONE',  ( 1.000000000000000000, 1.734723475976807094E-16, 0.000000000000000000 ) ) ;
#23669 = DIRECTION ( 'NONE',  ( 1.000000000000000000, 0.000000000000000000, 0.000000000000000000 ) ) ;
#23670 = CARTESIAN_POINT ( 'NONE',  ( -37.99974912065192711, -114.9929510916434339, 12.63488142334838571 ) ) ;
#23671 = LINE ( 'NONE', #34298, #21846 ) ;
#23672 = CARTESIAN_POINT ( 'NONE',  ( -34.54793860109200665, -114.9929510916434339, 13.00730889637958221 ) ) ;
#23673 = DIRECTION ( 'NONE',  ( 0.000000000000000000, 0.000000000000000000, -1.000000000000000000 ) ) ;
#23674 = DIRECTION ( 'NONE',  ( 0.000000000000000000, 0.000000000000000000, 1.000000000000000000 ) ) ;
#23675 = ORIENTED_EDGE ( 'NONE', *, *, #13057, .T. ) ;
#23676 = CARTESIAN_POINT ( 'NONE',  ( -36.07812499999994316, -115.9929510916434481, 13.11852480586264846 ) ) ;
#23677 = CARTESIAN_POINT ( 'NONE',  ( -35.50000000000000711, -116.0140978167138712, -0.1247823525984439463 ) ) ;
#23678 = CARTESIAN_POINT ( 'NONE',  ( 0.000000000000000000, 0.000000000000000000, 120.0000000000000000 ) ) ;
#23679 = DIRECTION ( 'NONE',  ( 0.000000000000000000, 0.000000000000000000, -1.000000000000000000 ) ) ;
#23680 = VERTEX_POINT ( 'NONE', #19731 ) ;
#23681 = DIRECTION ( 'NONE',  ( 0.000000000000000000, -0.4817536741017223179, 0.8763066800438598092 ) ) ;
#23682 = DIRECTION ( 'NONE',  ( -1.000000000000000000, 0.000000000000000000, 0.000000000000000000 ) ) ;
#23683 = ADVANCED_FACE ( 'NONE', ( #30743 ), #3400, .T. ) ;
#23684 = CARTESIAN_POINT ( 'NONE',  ( -50.00000000000000000, 10.00000000000000888, -25.00000000000000000 ) ) ;
#23685 = DIRECTION ( 'NONE',  ( -1.000000000000000000, 0.000000000000000000, 0.000000000000000000 ) ) ;
#23686 = ORIENTED_EDGE ( 'NONE', *, *, #32768, .F. ) ;
#23687 = AXIS2_PLACEMENT_3D ( 'NONE', #7756, #7413, #18739 ) ;
#23688 = MECHANICAL_DESIGN_GEOMETRIC_PRESENTATION_REPRESENTATION (  '', ( #32872 ), #98 ) ;
#23689 = CARTESIAN_POINT ( 'NONE',  ( -36.25098837183129774, -113.3347980657956242, 2.816024454178448710 ) ) ;
#23690 = CIRCLE ( 'NONE', #27707, 52.00000000000000711 ) ;
#23691 = DIRECTION ( 'NONE',  ( 1.000000000000000000, 0.000000000000000000, 0.000000000000000000 ) ) ;
#23692 = DIRECTION ( 'NONE',  ( -1.000000000000000000, 0.000000000000000000, 0.000000000000000000 ) ) ;
#23693 = EDGE_LOOP ( 'NONE', ( #24509, #28305, #34972, #13087 ) ) ;
#23694 = EDGE_LOOP ( 'NONE', ( #35052, #2026, #26043, #20069 ) ) ;
#23695 = DIRECTION ( 'NONE',  ( -1.000000000000000000, -0.000000000000000000, -0.000000000000000000 ) ) ;
#23696 = ORIENTED_EDGE ( 'NONE', *, *, #12766, .T. ) ;
#23697 = CARTESIAN_POINT ( 'NONE',  ( -38.18337828418796676, -117.0245472910329738, 8.965225545821551734 ) ) ;
#23698 = VERTEX_POINT ( 'NONE', #30923 ) ;
#23699 = PRESENTATION_STYLE_ASSIGNMENT (( #12184 ) ) ;
#23701 = ORIENTED_EDGE ( 'NONE', *, *, #15612, .F. ) ;
#23700 =( GEOMETRIC_REPRESENTATION_CONTEXT ( 3 ) GLOBAL_UNCERTAINTY_ASSIGNED_CONTEXT ( ( #1353 ) ) GLOBAL_UNIT_ASSIGNED_CONTEXT ( ( #3538, #31070, #9104 ) ) REPRESENTATION_CONTEXT ( 'NONE', 'WORKASPACE' ) );
#23702 = ORIENTED_EDGE ( 'NONE', *, *, #25118, .F. ) ;
#23703 = CARTESIAN_POINT ( 'NONE',  ( -34.49999999999998579, -21.98076211353320630, 84.99999999999994316 ) ) ;
#23704 = DIRECTION ( 'NONE',  ( 0.000000000000000000, 0.000000000000000000, 1.000000000000000000 ) ) ;
#23705 = FACE_OUTER_BOUND ( 'NONE', #10532, .T. ) ;
#23706 = VERTEX_POINT ( 'NONE', #502 ) ;
#23707 = ORIENTED_EDGE ( 'NONE', *, *, #8348, .T. ) ;
#23708 = CARTESIAN_POINT ( 'NONE',  ( -1.600000000000004086, -12.74999999999999822, -1.200000000000006617 ) ) ;
#23709 = AXIS2_PLACEMENT_3D ( 'NONE', #21085, #29750, #32090 ) ;
#23710 = CARTESIAN_POINT ( 'NONE',  ( -50.00000000000000000, 19.99999999999998934, -15.00000000000001421 ) ) ;
#23711 = AXIS2_PLACEMENT_3D ( 'NONE', #18836, #5176, #15948 ) ;
#23712 = ORIENTED_EDGE ( 'NONE', *, *, #18957, .T. ) ;
#23713 = CARTESIAN_POINT ( 'NONE',  ( 0.000000000000000000, 0.000000000000000000, 0.000000000000000000 ) ) ;
#23714 = DIRECTION ( 'NONE',  ( 0.000000000000000000, 0.000000000000000000, 1.000000000000000000 ) ) ;
#23715 = DIRECTION ( 'NONE',  ( -1.000000000000000000, -0.000000000000000000, -0.000000000000000000 ) ) ;
#23716 = CARTESIAN_POINT ( 'NONE',  ( -34.49999793727135966, -115.9929510916434481, 12.61164896875036767 ) ) ;
#23717 = CARTESIAN_POINT ( 'NONE',  ( 50.00005079999999680, 0.000000000000000000, 0.000000000000000000 ) ) ;
#23718 = CARTESIAN_POINT ( 'NONE',  ( -37.05926240293131713, -115.9999999999999858, 3.378524454178448710 ) ) ;
#23719 = CARTESIAN_POINT ( 'NONE',  ( -34.50000000000000000, -115.7766462221073454, 9.569741527169023598 ) ) ;
#23720 = FACE_OUTER_BOUND ( 'NONE', #14386, .T. ) ;
#23721 = CARTESIAN_POINT ( 'NONE',  ( 0.000000000000000000, 6.085920226791021292, 15.78165944574522861 ) ) ;
#23722 =( GEOMETRIC_REPRESENTATION_CONTEXT ( 3 ) GLOBAL_UNCERTAINTY_ASSIGNED_CONTEXT ( ( #17901 ) ) GLOBAL_UNIT_ASSIGNED_CONTEXT ( ( #5668, #18624, #29622 ) ) REPRESENTATION_CONTEXT ( 'NONE', 'WORKASPACE' ) );
#23723 = CIRCLE ( 'NONE', #30638, 7.199999999999993960 ) ;
#23724 = DIRECTION ( 'NONE',  ( -1.000000000000000000, 0.000000000000000000, 0.000000000000000000 ) ) ;
#23725 = DIRECTION ( 'NONE',  ( -1.000000000000000000, 0.000000000000000000, -0.000000000000000000 ) ) ;
#23726 = EDGE_CURVE ( 'NONE', #19400, #22699, #31277, .T. ) ;
#23727 = ADVANCED_FACE ( 'NONE', ( #6079, #11646 ), #665, .T. ) ;
#23728 = CARTESIAN_POINT ( 'NONE',  ( 3.799999999999999822, 0.000000000000000000, -44.50000000000000000 ) ) ;
#23729 = DIRECTION ( 'NONE',  ( -1.000000000000000000, 0.000000000000000000, -0.000000000000000000 ) ) ;
#23730 = ORIENTED_EDGE ( 'NONE', *, *, #22912, .F. ) ;
#23731 = CARTESIAN_POINT ( 'NONE',  ( -36.23083527818512550, -111.9754527089670404, 5.215225545821551734 ) ) ;
#23732 = CARTESIAN_POINT ( 'NONE',  ( 50.00005079999998969, 5.400000000000029665, -1.000000000000000888 ) ) ;
#23733 = CARTESIAN_POINT ( 'NONE',  ( -35.50000000000000711, -116.0140978167138712, 0.8752176474015622709 ) ) ;
#23734 = ORIENTED_EDGE ( 'NONE', *, *, #31764, .T. ) ;
#23735 = ORIENTED_EDGE ( 'NONE', *, *, #3783, .T. ) ;
#23736 = CIRCLE ( 'NONE', #23159, 4.000000000000000000 ) ;
#23737 = SURFACE_STYLE_FILL_AREA ( #346 ) ;
#23738 = DIRECTION ( 'NONE',  ( 0.000000000000000000, 0.000000000000000000, -1.000000000000000000 ) ) ;
#23739 = ORIENTED_EDGE ( 'NONE', *, *, #28661, .F. ) ;
#23740 = ADVANCED_FACE ( 'NONE', ( #1042, #9314 ), #27703, .T. ) ;
#23741 = ORIENTED_EDGE ( 'NONE', *, *, #10320, .F. ) ;
#23742 = ORIENTED_EDGE ( 'NONE', *, *, #30871, .F. ) ;
#23743 = DIRECTION ( 'NONE',  ( 0.000000000000000000, 0.000000000000000000, 1.000000000000000000 ) ) ;
#23744 = CARTESIAN_POINT ( 'NONE',  ( -35.00000000000000000, -113.9407375970690310, 9.996475545821589037 ) ) ;
#23745 = DIRECTION ( 'NONE',  ( 1.000000000000000000, 0.000000000000000000, 0.000000000000000000 ) ) ;
#23746 = LINE ( 'NONE', #24290, #25392 ) ;
#23747 = ORIENTED_EDGE ( 'NONE', *, *, #657, .T. ) ;
#23748 = ORIENTED_EDGE ( 'NONE', *, *, #16487, .F. ) ;
#23749 = AXIS2_PLACEMENT_3D ( 'NONE', #27237, #13545, #5276 ) ;
#23750 = CARTESIAN_POINT ( 'NONE',  ( -35.50000000000000711, -113.6318576702834804, 1.956056246348823580 ) ) ;
#23751 = AXIS2_PLACEMENT_3D ( 'NONE', #5868, #1004, #3180 ) ;
#23752 = AXIS2_PLACEMENT_3D ( 'NONE', #2198, #32584, #21245 ) ;
#23753 = DIRECTION ( 'NONE',  ( 0.000000000000000000, 0.000000000000000000, 1.000000000000000000 ) ) ;
#23754 = CARTESIAN_POINT ( 'NONE',  ( 8.000000000000000000, 0.9861715913090087771, -17.47118961583601049 ) ) ;
#23755 = EDGE_LOOP ( 'NONE', ( #24193, #21929 ) ) ;
#23756 = FACE_OUTER_BOUND ( 'NONE', #6731, .T. ) ;
#23757 = EDGE_CURVE ( 'NONE', #28798, #26858, #22019, .T. ) ;
#23758 = CARTESIAN_POINT ( 'NONE',  ( -34.50000000000000000, -112.8655373925166572, 1.864575885149403423 ) ) ;
#23759 = AXIS2_PLACEMENT_3D ( 'NONE', #29936, #29586, #7959 ) ;
#23760 = CARTESIAN_POINT ( 'NONE',  ( -34.50000000000000000, -114.9929510916434339, 10.85830208992344303 ) ) ;
#23761 = AXIS2_PLACEMENT_3D ( 'NONE', #4121, #4295, #6266 ) ;
#23762 = DIRECTION ( 'NONE',  ( -1.000000000000000000, 0.000000000000000000, 0.000000000000000000 ) ) ;
#23763 = CARTESIAN_POINT ( 'NONE',  ( -35.91854304697313438, -114.9929510916434339, 13.11211614918345703 ) ) ;
#23764 = DIRECTION ( 'NONE',  ( -1.000000000000000000, 0.000000000000000000, 0.000000000000000000 ) ) ;
#23765 = CARTESIAN_POINT ( 'NONE',  ( -34.50000000000000000, -114.9929510916434339, 10.52000928670414126 ) ) ;
#23766 = DIRECTION ( 'NONE',  ( 0.000000000000000000, 0.000000000000000000, 1.000000000000000000 ) ) ;
#23767 = CARTESIAN_POINT ( 'NONE',  ( -38.00000000000000711, -114.9929510916434339, 12.59652202191340820 ) ) ;
#23768 = CARTESIAN_POINT ( 'NONE',  ( 7.999999999999992895, 0.000000000000000000, 0.000000000000000000 ) ) ;
#23769 = ORIENTED_EDGE ( 'NONE', *, *, #11845, .T. ) ;
#23770 = DIRECTION ( 'NONE',  ( 0.000000000000000000, -0.7705132427757815927, -0.6374239897486989603 ) ) ;
#23771 = CARTESIAN_POINT ( 'NONE',  ( 0.000000000000000000, -0.5097555531874712331, 19.99350267651955093 ) ) ;
#23772 = EDGE_CURVE ( 'NONE', #18771, #20524, #31224, .T. ) ;
#23773 = ORIENTED_EDGE ( 'NONE', *, *, #26373, .T. ) ;
#23774 = EDGE_CURVE ( 'NONE', #1635, #32416, #175, .T. ) ;
#23775 = CARTESIAN_POINT ( 'NONE',  ( -36.00585935943767169, -114.9929510916434339, 13.11852578240983291 ) ) ;
#23776 = ORIENTED_EDGE ( 'NONE', *, *, #28388, .T. ) ;
#23777 = ADVANCED_FACE ( 'NONE', ( #22459, #33451 ), #8954, .T. ) ;
#23778 = CARTESIAN_POINT ( 'NONE',  ( -35.00000000000000000, -114.0592624029313242, 4.503524454178448266 ) ) ;
#23779 = DIRECTION ( 'NONE',  ( -1.000000000000000000, 0.000000000000000000, 0.000000000000000000 ) ) ;
#23780 = EDGE_LOOP ( 'NONE', ( #5058, #21772, #13510, #25833 ) ) ;
#23781 = AXIS2_PLACEMENT_3D ( 'NONE', #27870, #28226, #12017 ) ;
#23782 = VERTEX_POINT ( 'NONE', #19919 ) ;
#23783 = AXIS2_PLACEMENT_3D ( 'NONE', #23491, #31591, #34842 ) ;
#23784 = CARTESIAN_POINT ( 'NONE',  ( -34.50000000000000000, -113.0140978167134449, 0.8752176474011410523 ) ) ;
#23785 = CARTESIAN_POINT ( 'NONE',  ( 7.999999999999992895, 19.44205635905542451, 43.33776004284616334 ) ) ;
#23786 = CYLINDRICAL_SURFACE ( 'NONE', #22061, 9.999999999999994671 ) ;
#23787 = ADVANCED_FACE ( 'NONE', ( #25189 ), #1053, .T. ) ;
#23788 = VERTEX_POINT ( 'NONE', #3752 ) ;
#23789 = CARTESIAN_POINT ( 'NONE',  ( -39.16322519054179452, -116.0794154965774823, 2.066024454178448710 ) ) ;
#23790 = EDGE_CURVE ( 'NONE', #32535, #8148, #26094, .T. ) ;
#23791 = DIRECTION ( 'NONE',  ( -1.174092375852890260E-15, 4.222049128630259891E-16, 1.000000000000000000 ) ) ;
#23792 = AXIS2_PLACEMENT_3D ( 'NONE', #26675, #16365, #27380 ) ;
#23793 = LINE ( 'NONE', #10825, #26318 ) ;
#23794 = VECTOR ( 'NONE', #14660, 1000.000000000000000 ) ;
#23795 = ORIENTED_EDGE ( 'NONE', *, *, #26936, .T. ) ;
#23796 = ORIENTED_EDGE ( 'NONE', *, *, #11639, .F. ) ;
#23797 = CARTESIAN_POINT ( 'NONE',  ( 70.00001200000001234, -22.08487140685993921, 83.95300846256282057 ) ) ;
#23798 = AXIS2_PLACEMENT_3D ( 'NONE', #18240, #4764, #29245 ) ;
#23799 = DIRECTION ( 'NONE',  ( 0.000000000000000000, -2.423959199780483078E-15, 1.000000000000000000 ) ) ;
#23800 = ORIENTED_EDGE ( 'NONE', *, *, #1491, .T. ) ;
#23801 = ORIENTED_EDGE ( 'NONE', *, *, #11674, .F. ) ;
#23802 = CARTESIAN_POINT ( 'NONE',  ( -34.50000000000000000, -111.0140821919592327, -0.5779076015960634694 ) ) ;
#23803 = CARTESIAN_POINT ( 'NONE',  ( 7.999999999999992895, 0.000000000000000000, 0.000000000000000000 ) ) ;
#23804 = ORIENTED_EDGE ( 'NONE', *, *, #33030, .T. ) ;
#23805 = ORIENTED_EDGE ( 'NONE', *, *, #28806, .T. ) ;
#23806 = DIRECTION ( 'NONE',  ( 0.000000000000000000, 0.000000000000000000, 1.000000000000000000 ) ) ;
#23807 = ADVANCED_FACE ( 'NONE', ( #3408, #14356, #25541 ), #30577, .F. ) ;
#23808 = CIRCLE ( 'NONE', #3099, 4.000000000000003553 ) ;
#23809 = CIRCLE ( 'NONE', #27821, 20.00000000000000711 ) ;
#23810 = CARTESIAN_POINT ( 'NONE',  ( -34.50000000000000000, -113.9929510916434339, 10.50625754673586876 ) ) ;
#23811 = PRODUCT_DEFINITION ( 'UNKNOWN', '', #2336, #24450 ) ;
#23812 = CARTESIAN_POINT ( 'NONE',  ( 8.000000000000007105, -9.604183132802312173, -5.908880290975638161 ) ) ;
#23813 = CARTESIAN_POINT ( 'NONE',  ( -38.00000000000000711, -113.9929510916434339, 10.50625754673587053 ) ) ;
#23814 = CARTESIAN_POINT ( 'NONE',  ( -37.34375000000001421, -115.9929510916434481, 13.11852480586264846 ) ) ;
#23815 = CYLINDRICAL_SURFACE ( 'NONE', #16445, 4.000000000000000000 ) ;
#23816 = DIRECTION ( 'NONE',  ( 0.000000000000000000, 0.000000000000000000, -1.000000000000000000 ) ) ;
#23817 = VECTOR ( 'NONE', #19148, 1000.000000000000000 ) ;
#23818 = ADVANCED_FACE ( 'NONE', ( #16875 ), #25721, .T. ) ;
#23819 = VERTEX_POINT ( 'NONE', #11659 ) ;
#23820 = ADVANCED_FACE ( 'NONE', ( #22629 ), #30933, .T. ) ;
#23821 = CARTESIAN_POINT ( 'NONE',  ( 65.00000000000001421, -32.20716221109618260, 78.48218274074299927 ) ) ;
#23822 = CARTESIAN_POINT ( 'NONE',  ( 0.000000000000000000, 0.000000000000000000, 0.000000000000000000 ) ) ;
#23823 = FACE_OUTER_BOUND ( 'NONE', #34061, .T. ) ;
#23824 = EDGE_LOOP ( 'NONE', ( #21707, #8091, #28315, #4882 ) ) ;
#23825 = CARTESIAN_POINT ( 'NONE',  ( 0.000000000000000000, 0.000000000000000000, -33.50000000000000711 ) ) ;
#23826 = CARTESIAN_POINT ( 'NONE',  ( -35.50000000000000711, -112.0269151300720409, -0.7876962586524208776 ) ) ;
#23827 = DIRECTION ( 'NONE',  ( 1.000000000000000000, 0.000000000000000000, 0.000000000000000000 ) ) ;
#23828 = CARTESIAN_POINT ( 'NONE',  ( -35.50000000000000711, -114.2598117360253696, 9.542047897280109936 ) ) ;
#23829 = CARTESIAN_POINT ( 'NONE',  ( 8.000000000000000000, -13.55483219355736679, 11.06713717293235888 ) ) ;
#23830 = EDGE_CURVE ( 'NONE', #751, #8797, #9141, .T. ) ;
#23831 = EDGE_LOOP ( 'NONE', ( #30853, #4516, #23515, #29063 ) ) ;
#23832 = DIRECTION ( 'NONE',  ( 0.000000000000000000, 0.000000000000000000, 1.000000000000000000 ) ) ;
#23833 = CARTESIAN_POINT ( 'NONE',  ( -34.50000000000000000, -112.0066700803175763, -2.372276521656937920 ) ) ;
#23834 = DIRECTION ( 'NONE',  ( 0.000000000000000000, -0.3420201433256756518, 0.9396926207859058744 ) ) ;
#23835 = EDGE_LOOP ( 'NONE', ( #31783, #31302, #30153, #33701 ) ) ;
#23836 = ORIENTED_EDGE ( 'NONE', *, *, #16068, .F. ) ;
#23837 = CARTESIAN_POINT ( 'NONE',  ( -39.02454729103295961, -114.7691647218148745, 3.659774454178448710 ) ) ;
#23838 = CYLINDRICAL_SURFACE ( 'NONE', #19251, 10.00000000000000000 ) ;
#23839 = ORIENTED_EDGE ( 'NONE', *, *, #16095, .T. ) ;
#23840 = EDGE_LOOP ( 'NONE', ( #24772, #30083 ) ) ;
#23841 = CARTESIAN_POINT ( 'NONE',  ( -35.50000000000000000, -115.0140978167139707, -0.6247823525984387283 ) ) ;
#23842 = AXIS2_PLACEMENT_3D ( 'NONE', #30391, #30209, #8406 ) ;
#23843 = AXIS2_PLACEMENT_3D ( 'NONE', #24311, #7910, #29891 ) ;
#23844 = DIRECTION ( 'NONE',  ( -1.000000000000000000, -0.000000000000000000, 0.000000000000000000 ) ) ;
#23845 = EDGE_CURVE ( 'NONE', #30950, #21764, #6518, .T. ) ;
#23846 = CIRCLE ( 'NONE', #3165, 4.800000000000001599 ) ;
#23847 = DIRECTION ( 'NONE',  ( -1.000000000000000000, 0.000000000000000000, 0.000000000000000000 ) ) ;
#23848 = ADVANCED_FACE ( 'NONE', ( #28236 ), #3576, .T. ) ;
#23849 = CARTESIAN_POINT ( 'NONE',  ( -37.43749999999998579, -114.9929510916434339, 13.11852480586264669 ) ) ;
#23850 = ADVANCED_FACE ( 'NONE', ( #25900 ), #3943, .T. ) ;
#23851 = DIRECTION ( 'NONE',  ( -1.000000000000000000, -1.734723475976807094E-16, -0.000000000000000000 ) ) ;
#23852 = CARTESIAN_POINT ( 'NONE',  ( -34.50000000000000000, -113.8474311500459777, -1.624782352598427959 ) ) ;
#23853 = CARTESIAN_POINT ( 'NONE',  ( -34.50000000000000000, -114.9929510916434339, 12.50851088611648088 ) ) ;
#23854 = CARTESIAN_POINT ( 'NONE',  ( 0.000000000000000000, -9.471478019455027209, -14.71414642875966017 ) ) ;
#23855 = EDGE_CURVE ( 'NONE', #12176, #272, #20301, .T. ) ;
#23856 = DIRECTION ( 'NONE',  ( 0.000000000000000000, 1.000000000000000000, -1.067522139062650474E-15 ) ) ;
#23857 = ORIENTED_EDGE ( 'NONE', *, *, #24467, .F. ) ;
#23858 = CARTESIAN_POINT ( 'NONE',  ( -35.93473953453761993, -115.9929510916434481, 13.11451721564123396 ) ) ;
#23859 = CARTESIAN_POINT ( 'NONE',  ( 7.999999999999992895, 0.000000000000000000, 0.000000000000000000 ) ) ;
#23860 = DIRECTION ( 'NONE',  ( -1.000000000000000000, -1.387778780781445922E-16, 0.000000000000000000 ) ) ;
#23861 = EDGE_CURVE ( 'NONE', #15465, #34789, #33996, .T. ) ;
#23862 = PLANE ( 'NONE',  #12470 ) ;
#23863 = LINE ( 'NONE', #32314, #34336 ) ;
#23864 = ORIENTED_EDGE ( 'NONE', *, *, #2000, .T. ) ;
#23865 = CARTESIAN_POINT ( 'NONE',  ( 7.999999999999992895, -46.90537658765327933, -2.727856614654800005 ) ) ;
#23866 = DIRECTION ( 'NONE',  ( -1.000000000000000000, 0.000000000000000000, 0.000000000000000000 ) ) ;
#23867 = CIRCLE ( 'NONE', #20984, 13.00000000000000000 ) ;
#23868 = AXIS2_PLACEMENT_3D ( 'NONE', #8441, #685, #6271 ) ;
#23869 = DIRECTION ( 'NONE',  ( 0.000000000000000000, 0.4817536741017101609, 0.8763066800438663595 ) ) ;
#23870 = DIRECTION ( 'NONE',  ( -0.000000000000000000, -0.000000000000000000, -1.000000000000000000 ) ) ;
#23871 = ORIENTED_EDGE ( 'NONE', *, *, #26164, .F. ) ;
#23872 =( BOUNDED_SURFACE ( )  B_SPLINE_SURFACE ( 3, 3, ( 
 ( #6364, #1321, #12125, #17328, #14822, #16976, #23094, #9417, #17698, #28696, #4043, #14991, #25993, #12669, #9780, #1685, #2241, #21101, #21283, #31570, #9956, #15874, #26714, #15517, #26897, #1872, #20917, #4755, #4928, #1499, #32282, #29237, #31740, #12846, #35002, #23649, #20570, #34633, #4581, #15160, #15698, #18230, #2052, #28868, #26537, #23271, #23826, #34270, #34812, #18591, #7073, #7601, #10133, #32104, #10321, #31914, #7249, #20743, #7432, #29591, #9603, #18047, #6896, #18410, #17871, #4220, #23467, #26165, #12485, #13026, #34460, #29044, #24014, #29411, #4392, #15339, #26353, #22169, #16593, #5803, #16047, #10494, #8499, #27066, #16762, #24888, #24182, #18764, #30296, #35530, #32637, #27604, #2940, #7963, #2586, #27244, #18942, #5283, #19474, #24360, #35348, #30114 ),
 ( #29941, #32814, #10857, #16221, #8135, #42, #19115, #13550, #10674, #24538, #27773, #11032, #11197, #21458, #21817, #13206, #13900, #5452, #35177, #27423, #16404, #5634, #30472, #2409, #33168, #2772, #21633, #13735, #213, #24714, #32453, #21994, #32991, #5111, #7779, #8306, #29768, #13377, #19286, #3113, #9021, #20337, #17291, #34053, #11551, #1110, #6322, #14589, #14775, #3463, #14414, #563, #922, #25785, #12079, #22519, #17653, #28120, #14063, #8663, #3286, #9379, #25059, #28470, #31347, #19632, #3816, #25423, #30989, #385, #6674, #23053, #6497, #11384, #5974, #22345, #33339, #16931, #30639, #27936, #14244, #25243, #20161, #738, #33509, #17472, #8837, #19799, #11719, #17114, #30811, #6149, #22691, #33684, #19984, #28296, #3640, #25602, #11903, #22880, #33873, #31168 ),
 ( #9199, #5202, #4177, #31531, #9560, #9912, #9737, #29859, #28657, #4003, #26495, #20528, #14947, #1828, #34231, #12805, #31696, #25953, #23784, #20698, #34421, #1278, #7030, #6855, #12264, #7207, #23238, #29003, #17827, #34770, #10092, #28827, #18189, #29200, #15299, #18861, #15117, #26129, #23601, #1460, #4548, #23424, #18005, #26312, #12441, #1648, #4353, #12626, #15479, #34593, #20875, #31876, #7872, #21059, #32065, #28587, #17762, #28063, #22455, #20451, #3404, #28763, #1222, #507, #30748, #6607, #11831, #8948, #3937, #14884, #19914, #14518, #3571, #30929, #17225, #31464, #672, #11653, #6433, #28231, #17050, #12201, #9137, #25184, #17581, #23174, #25533, #34168, #20274, #848, #4116, #22623, #14351, #25358, #1048, #22810, #11484, #33447, #8768, #25895, #6084, #19735 ),
 ( #33617, #9491, #6261, #33812, #20099, #31106, #14703, #17401, #28404, #3747, #25716, #12020, #22989, #33992, #9318, #31280, #6790, #1394, #32127, #13575, #10698, #26066, #10348, #24209, #7455, #16249, #4779, #12371, #18436, #26739, #15724, #16075, #35561, #13234, #5310, #10519, #10164, #13058, #32305, #18794, #35373, #4951, #21664, #24045, #35030, #29799, #2080, #32474, #18617, #29435, #27268, #35200, #15057, #32669, #2610, #15904, #24566, #7991, #26927, #30140, #21309, #7628, #29615, #27095, #2268, #19143, #23852, #8162, #18973, #21135, #34840, #29971, #21482, #10883, #7807, #5138, #21848, #2433, #13402, #24386, #32844, #11057, #27801, #33194, #25087, #27966, #415, #30498, #27630, #19495, #20013, #3316, #3490, #13759, #3138, #33717, #8867, #33366, #9055, #19657, #14092, #22547 ),
 ( #6003, #25451, #11407, #30842, #22370, #70, #2968, #22193, #8692, #25269, #5830, #592, #13927, #24917, #30669, #8522, #14270, #16788, #11226, #11579, #16962, #240, #33538, #19831, #22025, #6180, #16431, #14442, #17143, #30323, #5660, #28148, #769, #33020, #16618, #11747, #22724, #5478, #27452, #8333, #2800, #24742, #19312, #26175, #1878, #18239, #12680, #12855, #12132, #6543, #4589, #23102, #23833, #20924, #20207, #14830, #26360, #31577, #28706, #23656, #34642, #4054, #34280, #23281, #14997, #1329, #15525, #20382, #9611, #20578, #26000, #12309, #26545, #31394, #6728, #1510, #6908, #1158, #31923, #28875, #9254, #1694, #7259, #17879, #29244, #4403, #4228, #31218, #17704, #34102, #9425, #20750, #15167, #17518, #28521, #3871, #9965, #25836, #12492, #23474, #34469, #9787 ),
 ( #31748, #7080, #18055, #29054, #15348, #26905, #18773, #21643, #29777, #24191, #21291, #13215, #13742, #32646, #32823, #7441, #21465, #27432, #2592, #27074, #2781, #13384, #32461, #16230, #16412, #13033, #8142, #5117, #7607, #24366, #10866, #35184, #32111, #10500, #16056, #26722, #27251, #2416, #13557, #4763, #35354, #34820, #10683, #10142, #7970, #30122, #18599, #19122, #18950, #29950, #21827, #7787, #5290, #32288, #24547, #5460, #21111, #29597, #18418, #35539, #29417, #15705, #35009, #2059, #24023, #10330, #4937, #15884, #2248, #25250, #3647, #5983, #17300, #33694, #28127, #28303, #27612, #22002, #19991, #2950, #24723, #748, #51, #30303, #6157, #11392, #8506, #3471, #14424, #19480, #14071, #30648, #16601, #17122, #19640, #25431, #5641, #16939, #11038, #27945, #6330, #3295 ),
 ( #30482, #5812, #11727, #19293, #14252, #32999, #9031, #16770, #13909, #24895, #25066, #27781, #221, #11204, #11560, #572, #22529, #33518, #22175, #33177, #22701, #8312, #8847, #3118, #19809, #30996, #30819, #394, #22351, #33347, #8674, #17478, #20707, #12634, #9568, #28835, #20537, #23244, #31540, #31707, #6683, #31882, #22887, #34238, #7215, #931, #17664, #9208, #23063, #23611, #1655, #6864, #15125, #9386, #17836, #14785, #25962, #9921, #1467, #1286, #28478, #4185, #18197, #26135, #25794, #3824, #4011, #14954, #14597, #18013, #12447, #20344, #20881, #12271, #20169, #34430, #1116, #34603, #12089, #34060, #25609, #28666, #23433, #31354, #9745, #33880, #7037, #29010, #4359, #15306, #26321, #6503, #11913, #31175, #29208, #2554, #35319, #15485, #34970, #13177, #21067, #5250 ) ),
 .UNSPECIFIED., .T., .F., .F. ) 
 B_SPLINE_SURFACE_WITH_KNOTS ( ( 4, 3, 4 ),
 ( 4, 2, 2, 2, 2, 2, 2, 2, 2, 2, 2, 2, 2, 2, 2, 2, 2, 2, 2, 2, 2, 2, 2, 2, 2, 2, 2, 2, 2, 2, 2, 2, 2, 2, 2, 2, 2, 2, 2, 2, 2, 2, 2, 2, 2, 2, 2, 2, 2, 2, 4 ),
 ( 0.000000000000000000, 0.5000000000000000000, 1.000000000000000000 ),
 ( 0.000000000000000000, 0.05194669433742771930, 0.07792004150614158242, 0.09090671509049851051, 0.09740005188267697456, 0.1038933886748554386, 0.1123700156520060500, 0.1208466426291566476, 0.1377998965834578704, 0.1717064044920602883, 0.2056129124006627062, 0.2225661663549639291, 0.2310427933321145266, 0.2395194203092651519, 0.2482763131408625423, 0.2570332059724599327, 0.2745469916356546580, 0.3095745629620442196, 0.3446021342884337813, 0.3621159199516285621, 0.3708728127832259247, 0.3796297056148233429, 0.3887999023441631730, 0.3979700990735030031, 0.4163104925321826633, 0.4529912794495420392, 0.4896720663669014151, 0.5080124598255810753, 0.5171826565549209054, 0.5263528532842607355, 0.5380287103930572190, 0.5497045675018538136, 0.5730562817194468916, 0.6197597101546329368, 0.6664631385898189819, 0.6898148528074120600, 0.7014907099162086546, 0.7131665670250051381, 0.7223367637543449682, 0.7315069604836847983, 0.7498473539423643475, 0.7865281408597235568, 0.8232089277770826552, 0.8415493212357623154, 0.8507195179651021455, 0.8598897146944418646, 0.8686466075260392827, 0.8774035003576365899, 0.8949172860208314262, 0.9299448573472208768, 1.000000000000000000 ),
 .UNSPECIFIED. ) 
 GEOMETRIC_REPRESENTATION_ITEM ( )  RATIONAL_B_SPLINE_SURFACE ( (
 ( 1.000000000000000000, 1.000000000000000000, 1.000000000000000000, 1.000000000000000000, 1.000000000000000000, 1.000000000000000000, 1.000000000000000000, 1.000000000000000000, 1.000000000000000000, 1.000000000000000000, 1.000000000000000000, 1.000000000000000000, 1.000000000000000000, 1.000000000000000000, 1.000000000000000000, 1.000000000000000000, 1.000000000000000000, 1.000000000000000000, 1.000000000000000000, 1.000000000000000000, 1.000000000000000000, 1.000000000000000000, 1.000000000000000000, 1.000000000000000000, 1.000000000000000000, 1.000000000000000000, 1.000000000000000000, 1.000000000000000000, 1.000000000000000000, 1.000000000000000000, 1.000000000000000000, 1.000000000000000000, 1.000000000000000000, 1.000000000000000000, 1.000000000000000000, 1.000000000000000000, 1.000000000000000000, 1.000000000000000000, 1.000000000000000000, 1.000000000000000000, 1.000000000000000000, 1.000000000000000000, 1.000000000000000000, 1.000000000000000000, 1.000000000000000000, 1.000000000000000000, 1.000000000000000000, 1.000000000000000000, 1.000000000000000000, 1.000000000000000000, 1.000000000000000000, 1.000000000000000000, 1.000000000000000000, 1.000000000000000000, 1.000000000000000000, 1.000000000000000000, 1.000000000000000000, 1.000000000000000000, 1.000000000000000000, 1.000000000000000000, 1.000000000000000000, 1.000000000000000000, 1.000000000000000000, 1.000000000000000000, 1.000000000000000000, 1.000000000000000000, 1.000000000000000000, 1.000000000000000000, 1.000000000000000000, 1.000000000000000000, 1.000000000000000000, 1.000000000000000000, 1.000000000000000000, 1.000000000000000000, 1.000000000000000000, 1.000000000000000000, 1.000000000000000000, 1.000000000000000000, 1.000000000000000000, 1.000000000000000000, 1.000000000000000000, 1.000000000000000000, 1.000000000000000000, 1.000000000000000000, 1.000000000000000000, 1.000000000000000000, 1.000000000000000000, 1.000000000000000000, 1.000000000000000000, 1.000000000000000000, 1.000000000000000000, 1.000000000000000000, 1.000000000000000000, 1.000000000000000000, 1.000000000000000000, 1.000000000000000000, 1.000000000000000000, 1.000000000000000000, 1.000000000000000000, 1.000000000000000000, 1.000000000000000000, 1.000000000000000000),
 ( 0.3333333333333333703, 0.3333333333333333703, 0.3333333333333333703, 0.3333333333333333703, 0.3333333333333333703, 0.3333333333333333703, 0.3333333333333333703, 0.3333333333333333703, 0.3333333333333333703, 0.3333333333333333703, 0.3333333333333333703, 0.3333333333333333703, 0.3333333333333333703, 0.3333333333333333703, 0.3333333333333333703, 0.3333333333333333703, 0.3333333333333333703, 0.3333333333333333703, 0.3333333333333333703, 0.3333333333333333703, 0.3333333333333333703, 0.3333333333333333703, 0.3333333333333333703, 0.3333333333333333703, 0.3333333333333333703, 0.3333333333333333703, 0.3333333333333333703, 0.3333333333333333703, 0.3333333333333333703, 0.3333333333333333703, 0.3333333333333333703, 0.3333333333333333703, 0.3333333333333333703, 0.3333333333333333703, 0.3333333333333333703, 0.3333333333333333703, 0.3333333333333333703, 0.3333333333333333703, 0.3333333333333333703, 0.3333333333333333703, 0.3333333333333333703, 0.3333333333333333703, 0.3333333333333333703, 0.3333333333333333703, 0.3333333333333333703, 0.3333333333333333703, 0.3333333333333333703, 0.3333333333333333703, 0.3333333333333333703, 0.3333333333333333703, 0.3333333333333333703, 0.3333333333333333703, 0.3333333333333333703, 0.3333333333333333703, 0.3333333333333333703, 0.3333333333333333703, 0.3333333333333333703, 0.3333333333333333703, 0.3333333333333333703, 0.3333333333333333703, 0.3333333333333333703, 0.3333333333333333703, 0.3333333333333333703, 0.3333333333333333703, 0.3333333333333333703, 0.3333333333333333703, 0.3333333333333333703, 0.3333333333333333703, 0.3333333333333333703, 0.3333333333333333703, 0.3333333333333333703, 0.3333333333333333703, 0.3333333333333333703, 0.3333333333333333703, 0.3333333333333333703, 0.3333333333333333703, 0.3333333333333333703, 0.3333333333333333703, 0.3333333333333333703, 0.3333333333333333703, 0.3333333333333333703, 0.3333333333333333703, 0.3333333333333333703, 0.3333333333333333703, 0.3333333333333333703, 0.3333333333333333703, 0.3333333333333333703, 0.3333333333333333703, 0.3333333333333333703, 0.3333333333333333703, 0.3333333333333333703, 0.3333333333333333703, 0.3333333333333333703, 0.3333333333333333703, 0.3333333333333333703, 0.3333333333333333703, 0.3333333333333333703, 0.3333333333333333703, 0.3333333333333333703, 0.3333333333333333703, 0.3333333333333333703, 0.3333333333333333703),
 ( 0.3333333333333333703, 0.3333333333333333703, 0.3333333333333333703, 0.3333333333333333703, 0.3333333333333333703, 0.3333333333333333703, 0.3333333333333333703, 0.3333333333333333703, 0.3333333333333333703, 0.3333333333333333703, 0.3333333333333333703, 0.3333333333333333703, 0.3333333333333333703, 0.3333333333333333703, 0.3333333333333333703, 0.3333333333333333703, 0.3333333333333333703, 0.3333333333333333703, 0.3333333333333333703, 0.3333333333333333703, 0.3333333333333333703, 0.3333333333333333703, 0.3333333333333333703, 0.3333333333333333703, 0.3333333333333333703, 0.3333333333333333703, 0.3333333333333333703, 0.3333333333333333703, 0.3333333333333333703, 0.3333333333333333703, 0.3333333333333333703, 0.3333333333333333703, 0.3333333333333333703, 0.3333333333333333703, 0.3333333333333333703, 0.3333333333333333703, 0.3333333333333333703, 0.3333333333333333703, 0.3333333333333333703, 0.3333333333333333703, 0.3333333333333333703, 0.3333333333333333703, 0.3333333333333333703, 0.3333333333333333703, 0.3333333333333333703, 0.3333333333333333703, 0.3333333333333333703, 0.3333333333333333703, 0.3333333333333333703, 0.3333333333333333703, 0.3333333333333333703, 0.3333333333333333703, 0.3333333333333333703, 0.3333333333333333703, 0.3333333333333333703, 0.3333333333333333703, 0.3333333333333333703, 0.3333333333333333703, 0.3333333333333333703, 0.3333333333333333703, 0.3333333333333333703, 0.3333333333333333703, 0.3333333333333333703, 0.3333333333333333703, 0.3333333333333333703, 0.3333333333333333703, 0.3333333333333333703, 0.3333333333333333703, 0.3333333333333333703, 0.3333333333333333703, 0.3333333333333333703, 0.3333333333333333703, 0.3333333333333333703, 0.3333333333333333703, 0.3333333333333333703, 0.3333333333333333703, 0.3333333333333333703, 0.3333333333333333703, 0.3333333333333333703, 0.3333333333333333703, 0.3333333333333333703, 0.3333333333333333703, 0.3333333333333333703, 0.3333333333333333703, 0.3333333333333333703, 0.3333333333333333703, 0.3333333333333333703, 0.3333333333333333703, 0.3333333333333333703, 0.3333333333333333703, 0.3333333333333333703, 0.3333333333333333703, 0.3333333333333333703, 0.3333333333333333703, 0.3333333333333333703, 0.3333333333333333703, 0.3333333333333333703, 0.3333333333333333703, 0.3333333333333333703, 0.3333333333333333703, 0.3333333333333333703, 0.3333333333333333703),
 ( 1.000000000000000000, 1.000000000000000000, 1.000000000000000000, 1.000000000000000000, 1.000000000000000000, 1.000000000000000000, 1.000000000000000000, 1.000000000000000000, 1.000000000000000000, 1.000000000000000000, 1.000000000000000000, 1.000000000000000000, 1.000000000000000000, 1.000000000000000000, 1.000000000000000000, 1.000000000000000000, 1.000000000000000000, 1.000000000000000000, 1.000000000000000000, 1.000000000000000000, 1.000000000000000000, 1.000000000000000000, 1.000000000000000000, 1.000000000000000000, 1.000000000000000000, 1.000000000000000000, 1.000000000000000000, 1.000000000000000000, 1.000000000000000000, 1.000000000000000000, 1.000000000000000000, 1.000000000000000000, 1.000000000000000000, 1.000000000000000000, 1.000000000000000000, 1.000000000000000000, 1.000000000000000000, 1.000000000000000000, 1.000000000000000000, 1.000000000000000000, 1.000000000000000000, 1.000000000000000000, 1.000000000000000000, 1.000000000000000000, 1.000000000000000000, 1.000000000000000000, 1.000000000000000000, 1.000000000000000000, 1.000000000000000000, 1.000000000000000000, 1.000000000000000000, 1.000000000000000000, 1.000000000000000000, 1.000000000000000000, 1.000000000000000000, 1.000000000000000000, 1.000000000000000000, 1.000000000000000000, 1.000000000000000000, 1.000000000000000000, 1.000000000000000000, 1.000000000000000000, 1.000000000000000000, 1.000000000000000000, 1.000000000000000000, 1.000000000000000000, 1.000000000000000000, 1.000000000000000000, 1.000000000000000000, 1.000000000000000000, 1.000000000000000000, 1.000000000000000000, 1.000000000000000000, 1.000000000000000000, 1.000000000000000000, 1.000000000000000000, 1.000000000000000000, 1.000000000000000000, 1.000000000000000000, 1.000000000000000000, 1.000000000000000000, 1.000000000000000000, 1.000000000000000000, 1.000000000000000000, 1.000000000000000000, 1.000000000000000000, 1.000000000000000000, 1.000000000000000000, 1.000000000000000000, 1.000000000000000000, 1.000000000000000000, 1.000000000000000000, 1.000000000000000000, 1.000000000000000000, 1.000000000000000000, 1.000000000000000000, 1.000000000000000000, 1.000000000000000000, 1.000000000000000000, 1.000000000000000000, 1.000000000000000000, 1.000000000000000000),
 ( 0.3333333333333333703, 0.3333333333333333703, 0.3333333333333333703, 0.3333333333333333703, 0.3333333333333333703, 0.3333333333333333703, 0.3333333333333333703, 0.3333333333333333703, 0.3333333333333333703, 0.3333333333333333703, 0.3333333333333333703, 0.3333333333333333703, 0.3333333333333333703, 0.3333333333333333703, 0.3333333333333333703, 0.3333333333333333703, 0.3333333333333333703, 0.3333333333333333703, 0.3333333333333333703, 0.3333333333333333703, 0.3333333333333333703, 0.3333333333333333703, 0.3333333333333333703, 0.3333333333333333703, 0.3333333333333333703, 0.3333333333333333703, 0.3333333333333333703, 0.3333333333333333703, 0.3333333333333333703, 0.3333333333333333703, 0.3333333333333333703, 0.3333333333333333703, 0.3333333333333333703, 0.3333333333333333703, 0.3333333333333333703, 0.3333333333333333703, 0.3333333333333333703, 0.3333333333333333703, 0.3333333333333333703, 0.3333333333333333703, 0.3333333333333333703, 0.3333333333333333703, 0.3333333333333333703, 0.3333333333333333703, 0.3333333333333333703, 0.3333333333333333703, 0.3333333333333333703, 0.3333333333333333703, 0.3333333333333333703, 0.3333333333333333703, 0.3333333333333333703, 0.3333333333333333703, 0.3333333333333333703, 0.3333333333333333703, 0.3333333333333333703, 0.3333333333333333703, 0.3333333333333333703, 0.3333333333333333703, 0.3333333333333333703, 0.3333333333333333703, 0.3333333333333333703, 0.3333333333333333703, 0.3333333333333333703, 0.3333333333333333703, 0.3333333333333333703, 0.3333333333333333703, 0.3333333333333333703, 0.3333333333333333703, 0.3333333333333333703, 0.3333333333333333703, 0.3333333333333333703, 0.3333333333333333703, 0.3333333333333333703, 0.3333333333333333703, 0.3333333333333333703, 0.3333333333333333703, 0.3333333333333333703, 0.3333333333333333703, 0.3333333333333333703, 0.3333333333333333703, 0.3333333333333333703, 0.3333333333333333703, 0.3333333333333333703, 0.3333333333333333703, 0.3333333333333333703, 0.3333333333333333703, 0.3333333333333333703, 0.3333333333333333703, 0.3333333333333333703, 0.3333333333333333703, 0.3333333333333333703, 0.3333333333333333703, 0.3333333333333333703, 0.3333333333333333703, 0.3333333333333333703, 0.3333333333333333703, 0.3333333333333333703, 0.3333333333333333703, 0.3333333333333333703, 0.3333333333333333703, 0.3333333333333333703, 0.3333333333333333703),
 ( 0.3333333333333333703, 0.3333333333333333703, 0.3333333333333333703, 0.3333333333333333703, 0.3333333333333333703, 0.3333333333333333703, 0.3333333333333333703, 0.3333333333333333703, 0.3333333333333333703, 0.3333333333333333703, 0.3333333333333333703, 0.3333333333333333703, 0.3333333333333333703, 0.3333333333333333703, 0.3333333333333333703, 0.3333333333333333703, 0.3333333333333333703, 0.3333333333333333703, 0.3333333333333333703, 0.3333333333333333703, 0.3333333333333333703, 0.3333333333333333703, 0.3333333333333333703, 0.3333333333333333703, 0.3333333333333333703, 0.3333333333333333703, 0.3333333333333333703, 0.3333333333333333703, 0.3333333333333333703, 0.3333333333333333703, 0.3333333333333333703, 0.3333333333333333703, 0.3333333333333333703, 0.3333333333333333703, 0.3333333333333333703, 0.3333333333333333703, 0.3333333333333333703, 0.3333333333333333703, 0.3333333333333333703, 0.3333333333333333703, 0.3333333333333333703, 0.3333333333333333703, 0.3333333333333333703, 0.3333333333333333703, 0.3333333333333333703, 0.3333333333333333703, 0.3333333333333333703, 0.3333333333333333703, 0.3333333333333333703, 0.3333333333333333703, 0.3333333333333333703, 0.3333333333333333703, 0.3333333333333333703, 0.3333333333333333703, 0.3333333333333333703, 0.3333333333333333703, 0.3333333333333333703, 0.3333333333333333703, 0.3333333333333333703, 0.3333333333333333703, 0.3333333333333333703, 0.3333333333333333703, 0.3333333333333333703, 0.3333333333333333703, 0.3333333333333333703, 0.3333333333333333703, 0.3333333333333333703, 0.3333333333333333703, 0.3333333333333333703, 0.3333333333333333703, 0.3333333333333333703, 0.3333333333333333703, 0.3333333333333333703, 0.3333333333333333703, 0.3333333333333333703, 0.3333333333333333703, 0.3333333333333333703, 0.3333333333333333703, 0.3333333333333333703, 0.3333333333333333703, 0.3333333333333333703, 0.3333333333333333703, 0.3333333333333333703, 0.3333333333333333703, 0.3333333333333333703, 0.3333333333333333703, 0.3333333333333333703, 0.3333333333333333703, 0.3333333333333333703, 0.3333333333333333703, 0.3333333333333333703, 0.3333333333333333703, 0.3333333333333333703, 0.3333333333333333703, 0.3333333333333333703, 0.3333333333333333703, 0.3333333333333333703, 0.3333333333333333703, 0.3333333333333333703, 0.3333333333333333703, 0.3333333333333333703, 0.3333333333333333703),
 ( 1.000000000000000000, 1.000000000000000000, 1.000000000000000000, 1.000000000000000000, 1.000000000000000000, 1.000000000000000000, 1.000000000000000000, 1.000000000000000000, 1.000000000000000000, 1.000000000000000000, 1.000000000000000000, 1.000000000000000000, 1.000000000000000000, 1.000000000000000000, 1.000000000000000000, 1.000000000000000000, 1.000000000000000000, 1.000000000000000000, 1.000000000000000000, 1.000000000000000000, 1.000000000000000000, 1.000000000000000000, 1.000000000000000000, 1.000000000000000000, 1.000000000000000000, 1.000000000000000000, 1.000000000000000000, 1.000000000000000000, 1.000000000000000000, 1.000000000000000000, 1.000000000000000000, 1.000000000000000000, 1.000000000000000000, 1.000000000000000000, 1.000000000000000000, 1.000000000000000000, 1.000000000000000000, 1.000000000000000000, 1.000000000000000000, 1.000000000000000000, 1.000000000000000000, 1.000000000000000000, 1.000000000000000000, 1.000000000000000000, 1.000000000000000000, 1.000000000000000000, 1.000000000000000000, 1.000000000000000000, 1.000000000000000000, 1.000000000000000000, 1.000000000000000000, 1.000000000000000000, 1.000000000000000000, 1.000000000000000000, 1.000000000000000000, 1.000000000000000000, 1.000000000000000000, 1.000000000000000000, 1.000000000000000000, 1.000000000000000000, 1.000000000000000000, 1.000000000000000000, 1.000000000000000000, 1.000000000000000000, 1.000000000000000000, 1.000000000000000000, 1.000000000000000000, 1.000000000000000000, 1.000000000000000000, 1.000000000000000000, 1.000000000000000000, 1.000000000000000000, 1.000000000000000000, 1.000000000000000000, 1.000000000000000000, 1.000000000000000000, 1.000000000000000000, 1.000000000000000000, 1.000000000000000000, 1.000000000000000000, 1.000000000000000000, 1.000000000000000000, 1.000000000000000000, 1.000000000000000000, 1.000000000000000000, 1.000000000000000000, 1.000000000000000000, 1.000000000000000000, 1.000000000000000000, 1.000000000000000000, 1.000000000000000000, 1.000000000000000000, 1.000000000000000000, 1.000000000000000000, 1.000000000000000000, 1.000000000000000000, 1.000000000000000000, 1.000000000000000000, 1.000000000000000000, 1.000000000000000000, 1.000000000000000000, 1.000000000000000000) ) ) 
 REPRESENTATION_ITEM ( '' )  SURFACE ( )  );
#23873 = CARTESIAN_POINT ( 'NONE',  ( -35.99999999999999289, -114.0592624029313242, 6.003524454178450043 ) ) ;
#23874 = DIRECTION ( 'NONE',  ( 0.000000000000000000, 0.000000000000000000, -1.000000000000000000 ) ) ;
#23875 = DIRECTION ( 'NONE',  ( 0.000000000000000000, 0.9980267284282713369, 0.06279051952931692659 ) ) ;
#23876 = VECTOR ( 'NONE', #32901, 1000.000000000000000 ) ;
#23877 = ORIENTED_EDGE ( 'NONE', *, *, #31134, .F. ) ;
#23878 = EDGE_LOOP ( 'NONE', ( #696, #33179, #3120, #28523 ) ) ;
#23879 = VECTOR ( 'NONE', #24196, 1000.000000000000000 ) ;
#23880 = DIRECTION ( 'NONE',  ( 1.000000000000000000, 1.734723475976807094E-16, 0.000000000000000000 ) ) ;
#23881 = CARTESIAN_POINT ( 'NONE',  ( 8.000000000000000000, -0.3212489022566501484, 16.91141623315869680 ) ) ;
#23882 = ORIENTED_EDGE ( 'NONE', *, *, #19760, .T. ) ;
#23883 = CARTESIAN_POINT ( 'NONE',  ( -38.45611840935523418, -112.6276912846090568, 3.433975545821551290 ) ) ;
#23884 = VERTEX_POINT ( 'NONE', #31288 ) ;
#23885 = CONTEXT_DEPENDENT_SHAPE_REPRESENTATION ( #14265, #32538 ) ;
#23886 = AXIS2_PLACEMENT_3D ( 'NONE', #17502, #9407, #11752 ) ;
#23887 = EDGE_LOOP ( 'NONE', ( #16022, #16281, #23254, #1271 ) ) ;
#23888 = EDGE_LOOP ( 'NONE', ( #14950, #3807, #20716, #21165 ) ) ;
#23889 = CARTESIAN_POINT ( 'NONE',  ( 0.000000000000000000, 0.000000000000000000, -1.200000000000006617 ) ) ;
#23890 = EDGE_CURVE ( 'NONE', #17346, #18651, #202, .T. ) ;
#23891 = CYLINDRICAL_SURFACE ( 'NONE', #20784, 4.800000000000000711 ) ;
#23892 = ORIENTED_EDGE ( 'NONE', *, *, #22303, .T. ) ;
#23893 = ORIENTED_EDGE ( 'NONE', *, *, #25118, .T. ) ;
#23894 = EDGE_CURVE ( 'NONE', #19390, #31137, #29550, .T. ) ;
#23895 = AXIS2_PLACEMENT_3D ( 'NONE', #17016, #28025, #35606 ) ;
#23896 = DIRECTION ( 'NONE',  ( 1.000000000000000000, 0.000000000000000000, -1.691777834109591064E-31 ) ) ;
#23897 = DIRECTION ( 'NONE',  ( -1.000000000000000000, 0.000000000000000000, 0.000000000000000000 ) ) ;
#23898 = VERTEX_POINT ( 'NONE', #17944 ) ;
#23899 = DIRECTION ( 'NONE',  ( -1.000000000000000000, 0.000000000000000000, 0.000000000000000000 ) ) ;
#23900 = VECTOR ( 'NONE', #1371, 1000.000000000000000 ) ;
#23901 = DIRECTION ( 'NONE',  ( -1.000000000000000000, -0.000000000000000000, 0.000000000000000000 ) ) ;
#23902 = CARTESIAN_POINT ( 'NONE',  ( 50.00005079999998969, 10.58300524425836109, 3.000000000000002665 ) ) ;
#23903 = CARTESIAN_POINT ( 'NONE',  ( -34.68937937320795584, -115.9929510916434481, 13.37409560816408671 ) ) ;
#23904 = DIRECTION ( 'NONE',  ( -1.000000000000000000, 0.000000000000000000, 0.000000000000000000 ) ) ;
#23905 = CARTESIAN_POINT ( 'NONE',  ( -38.97545270896704039, -113.1123104723225055, 8.347274454178448266 ) ) ;
#23906 = CARTESIAN_POINT ( 'NONE',  ( -34.50000000000000000, -115.9929081983957104, 10.49113315946066294 ) ) ;
#23907 = FACE_OUTER_BOUND ( 'NONE', #11284, .T. ) ;
#23908 = LINE ( 'NONE', #7155, #1765 ) ;
#23909 = VECTOR ( 'NONE', #24310, 1000.000000000000000 ) ;
#23910 = CYLINDRICAL_SURFACE ( 'NONE', #33711, 20.00000000000000355 ) ;
#23911 = CARTESIAN_POINT ( 'NONE',  ( 0.000000000000000000, 0.000000000000000000, 35.10000000000000142 ) ) ;
#23912 = DIRECTION ( 'NONE',  ( 0.000000000000000000, -0.6845471059286792892, -0.7289686274214203232 ) ) ;
#23913 = DIRECTION ( 'NONE',  ( 1.000000000000000000, -0.000000000000000000, 0.000000000000000000 ) ) ;
#23914 = ORIENTED_EDGE ( 'NONE', *, *, #24071, .F. ) ;
#23915 = CARTESIAN_POINT ( 'NONE',  ( -34.97545270896703329, -114.7691647218148745, 5.590225545821552622 ) ) ;
#23916 = DIRECTION ( 'NONE',  ( -0.000000000000000000, 0.000000000000000000, 1.000000000000000000 ) ) ;
#23917 = DIRECTION ( 'NONE',  ( 0.000000000000000000, 0.000000000000000000, 1.000000000000000000 ) ) ;
#23918 = ORIENTED_EDGE ( 'NONE', *, *, #7503, .T. ) ;
#23919 = EDGE_LOOP ( 'NONE', ( #2550, #34285, #7656, #29424 ) ) ;
#23921 = SURFACE_SIDE_STYLE ('',( #23737 ) ) ;
#23920 = PRODUCT_DEFINITION_SHAPE ( 'NONE', 'NONE',  #35632 ) ;
#23922 = CIRCLE ( 'NONE', #8371, 17.49900000000000233 ) ;
#23923 = CYLINDRICAL_SURFACE ( 'NONE', #1398, 11.00000000000000000 ) ;
#23924 = EDGE_LOOP ( 'NONE', ( #7565, #14236, #20787, #32293 ) ) ;
#23925 = ORIENTED_EDGE ( 'NONE', *, *, #25683, .F. ) ;
#23926 = ORIENTED_EDGE ( 'NONE', *, *, #18229, .F. ) ;
#23927 = CIRCLE ( 'NONE', #23337, 52.00000000000000711 ) ;
#23928 = CIRCLE ( 'NONE', #8377, 15.49899999999998457 ) ;
#23929 = CIRCLE ( 'NONE', #22108, 11.00000000000000000 ) ;
#23930 = CARTESIAN_POINT ( 'NONE',  ( 8.000000000000000000, 0.000000000000000000, 0.000000000000000000 ) ) ;
#23931 = LINE ( 'NONE', #21214, #7929 ) ;
#23932 = CARTESIAN_POINT ( 'NONE',  ( 1.387778780781445676E-14, -1.387778780781445676E-14, 110.0000000000000000 ) ) ;
#23933 = CARTESIAN_POINT ( 'NONE',  ( -26.99999999999998934, -19.99999999999999289, 0.000000000000000000 ) ) ;
#23935 = ORIENTED_EDGE ( 'NONE', *, *, #5165, .T. ) ;
#23934 = AXIS2_PLACEMENT_3D ( 'NONE', #17062, #1059, #517 ) ;
#23936 = ORIENTED_EDGE ( 'NONE', *, *, #21841, .F. ) ;
#23937 = CARTESIAN_POINT ( 'NONE',  ( -35.50000000000000711, -112.9876085932806262, 1.879154677457530065 ) ) ;
#23938 = EDGE_CURVE ( 'NONE', #31629, #24733, #3684, .T. ) ;
#23939 = FACE_OUTER_BOUND ( 'NONE', #16255, .T. ) ;
#23940 = CARTESIAN_POINT ( 'NONE',  ( -21.15833593587365513, -8.980762113533204527, 86.49999999999994316 ) ) ;
#23941 = ORIENTED_EDGE ( 'NONE', *, *, #33710, .F. ) ;
#23942 = FACE_OUTER_BOUND ( 'NONE', #25056, .T. ) ;
#23943 = CARTESIAN_POINT ( 'NONE',  ( -34.49999999999998579, -25.98076211353322051, 84.99999999999992895 ) ) ;
#23944 = CARTESIAN_POINT ( 'NONE',  ( -34.50000000000000000, -114.9929510916434339, 12.17846912687782712 ) ) ;
#23945 = CIRCLE ( 'NONE', #34879, 3.799999999999999822 ) ;
#23946 = CARTESIAN_POINT ( 'NONE',  ( 4.000000000000003553, -2.912696353505664248, -21.80633394113455736 ) ) ;
#23947 = CARTESIAN_POINT ( 'NONE',  ( -37.75185693410092824, -114.9929510916434339, 13.05539834812634581 ) ) ;
#23948 = CARTESIAN_POINT ( 'NONE',  ( -90.00000000000002842, -4.871103520542888323E-16, -7.020000000000039542 ) ) ;
#23949 = EDGE_CURVE ( 'NONE', #17877, #23592, #7110, .T. ) ;
#23950 = CARTESIAN_POINT ( 'NONE',  ( -34.50000000000000000, -114.9819937217110635, 10.35556074009299188 ) ) ;
#23951 = DIRECTION ( 'NONE',  ( 0.000000000000000000, 0.000000000000000000, 1.000000000000000000 ) ) ;
#23952 = CIRCLE ( 'NONE', #2683, 7.199999999999993072 ) ;
#23953 = AXIS2_PLACEMENT_3D ( 'NONE', #26253, #14717, #1594 ) ;
#23954 = CARTESIAN_POINT ( 'NONE',  ( -37.52044295795950291, -114.9929510916434339, 13.11812344617477244 ) ) ;
#23955 = CYLINDRICAL_SURFACE ( 'NONE', #389, 47.49900000000001654 ) ;
#23956 = ORIENTED_EDGE ( 'NONE', *, *, #7750, .F. ) ;
#23957 = CARTESIAN_POINT ( 'NONE',  ( 0.000000000000000000, 30.93515269692163372, -36.04401931830219752 ) ) ;
#23958 = CARTESIAN_POINT ( 'NONE',  ( 7.999999999999992895, 44.61570720899074161, 14.73072383765644489 ) ) ;
#23959 = ORIENTED_EDGE ( 'NONE', *, *, #7323, .T. ) ;
#23960 = CARTESIAN_POINT ( 'NONE',  ( -37.99974912065192711, -114.9929510916434339, 12.63488142334838571 ) ) ;
#23961 = ORIENTED_EDGE ( 'NONE', *, *, #26503, .F. ) ;
#23962 = CARTESIAN_POINT ( 'NONE',  ( -35.02454729103298803, -114.8876895276775087, 7.597274454178450931 ) ) ;
#23963 = VECTOR ( 'NONE', #32822, 1000.000000000000000 ) ;
#23964 = CARTESIAN_POINT ( 'NONE',  ( 55.00000000000000711, -25.01350700525240356, 84.74619386235809770 ) ) ;
#23965 = VECTOR ( 'NONE', #1015, 1000.000000000000000 ) ;
#23966 = ORIENTED_EDGE ( 'NONE', *, *, #2072, .F. ) ;
#23967 = ORIENTED_EDGE ( 'NONE', *, *, #12611, .T. ) ;
#23968 = DIRECTION ( 'NONE',  ( -1.000000000000000000, 0.000000000000000000, 0.000000000000000000 ) ) ;
#23969 = EDGE_LOOP ( 'NONE', ( #23735, #25577, #21491, #1082 ) ) ;
#23970 = CARTESIAN_POINT ( 'NONE',  ( -37.05926240293131713, -115.9999999999999858, 7.878524454178450043 ) ) ;
#23971 = VECTOR ( 'NONE', #17947, 1000.000000000000000 ) ;
#23972 = LINE ( 'NONE', #18195, #4464 ) ;
#23973 = AXIS2_PLACEMENT_3D ( 'NONE', #20158, #17112, #19982 ) ;
#23974 = CARTESIAN_POINT ( 'NONE',  ( 7.999999999999992895, 44.47301969247445896, 16.68249143361927267 ) ) ;
#23975 = ORIENTED_EDGE ( 'NONE', *, *, #4454, .T. ) ;
#23976 = ORIENTED_EDGE ( 'NONE', *, *, #4443, .F. ) ;
#23977 = CYLINDRICAL_SURFACE ( 'NONE', #28599, 52.00000000000000711 ) ;
#23978 = AXIS2_PLACEMENT_3D ( 'NONE', #294, #11282, #22254 ) ;
#23979 = CARTESIAN_POINT ( 'NONE',  ( 0.000000000000000000, 18.48663108841359559, -3.384281271887881637 ) ) ;
#23980 = ORIENTED_EDGE ( 'NONE', *, *, #17281, .F. ) ;
#23981 = ORIENTED_EDGE ( 'NONE', *, *, #7748, .F. ) ;
#23982 = CARTESIAN_POINT ( 'NONE',  ( -34.50000000000000000, -111.3577635893106361, 2.022004269840791402 ) ) ;
#23983 = CIRCLE ( 'NONE', #11911, 20.00000000000000000 ) ;
#23984 = ADVANCED_FACE ( 'NONE', ( #23536 ), #26244, .F. ) ;
#23985 = EDGE_CURVE ( 'NONE', #3344, #13171, #27819, .T. ) ;
#23986 = CIRCLE ( 'NONE', #32023, 4.800000000000006040 ) ;
#23987 = DIRECTION ( 'NONE',  ( 1.000000000000000000, -0.000000000000000000, 0.000000000000000000 ) ) ;
#23988 = ORIENTED_EDGE ( 'NONE', *, *, #3122, .F. ) ;
#23989 = VERTEX_POINT ( 'NONE', #26429 ) ;
#23990 = VECTOR ( 'NONE', #30994, 1000.000000000000000 ) ;
#23991 = CARTESIAN_POINT ( 'NONE',  ( -35.50000000000000711, -114.1189822439768449, 9.514224058074130852 ) ) ;
#23992 = VECTOR ( 'NONE', #10362, 1000.000000000000000 ) ;
#23993 = CARTESIAN_POINT ( 'NONE',  ( -34.50000000000000000, -113.9929510916438460, 10.50625754673626133 ) ) ;
#23994 = FACE_OUTER_BOUND ( 'NONE', #27729, .T. ) ;
#23995 = CARTESIAN_POINT ( 'NONE',  ( 7.999999999999992895, 32.32520163883631170, -34.09746168776000985 ) ) ;
#23996 = EDGE_CURVE ( 'NONE', #21999, #211, #9498, .T. ) ;
#23997 = CARTESIAN_POINT ( 'NONE',  ( -34.50000000000000000, -113.9836614335179377, 10.50514867547815534 ) ) ;
#23998 = EDGE_CURVE ( 'NONE', #21509, #15577, #6540, .T. ) ;
#23999 = CARTESIAN_POINT ( 'NONE',  ( -36.15625000000007816, -115.9929510916434481, 13.11852480586264846 ) ) ;
#24000 = CIRCLE ( 'NONE', #14209, 15.49899999999998279 ) ;
#24001 = CARTESIAN_POINT ( 'NONE',  ( -49.99999999999999289, -27.99999999999999289, 113.9999999999999858 ) ) ;
#24002 = EDGE_CURVE ( 'NONE', #1954, #4878, #10033, .T. ) ;
#24003 = FACE_OUTER_BOUND ( 'NONE', #13522, .T. ) ;
#24004 = CIRCLE ( 'NONE', #13084, 7.199999999999994849 ) ;
#24005 = ORIENTED_EDGE ( 'NONE', *, *, #28040, .T. ) ;
#24006 = FACE_OUTER_BOUND ( 'NONE', #14584, .T. ) ;
#24007 = CARTESIAN_POINT ( 'NONE',  ( 8.000000000000000000, -13.60411018104308667, -12.96676809804163000 ) ) ;
#24008 = DIRECTION ( 'NONE',  ( 1.110223024625156540E-16, 1.000000000000000000, 0.000000000000000000 ) ) ;
#24009 = CIRCLE ( 'NONE', #17660, 1.000000000000000444 ) ;
#24010 = AXIS2_PLACEMENT_3D ( 'NONE', #11074, #7824, #22042 ) ;
#24011 = ORIENTED_EDGE ( 'NONE', *, *, #14084, .T. ) ;
#24012 = VECTOR ( 'NONE', #33136, 1000.000000000000000 ) ;
#24013 = FACE_BOUND ( 'NONE', #31751, .T. ) ;
#24014 = CARTESIAN_POINT ( 'NONE',  ( -35.50000000000000711, -114.8474311500471572, -1.624782352598427959 ) ) ;
#24015 = CARTESIAN_POINT ( 'NONE',  ( 8.000000000000000000, -21.80633394113452184, 2.912696353505742852 ) ) ;
#24016 = AXIS2_PLACEMENT_3D ( 'NONE', #4790, #15732, #26750 ) ;
#24017 = AXIS2_PLACEMENT_3D ( 'NONE', #14114, #25650, #8711 ) ;
#24018 = CARTESIAN_POINT ( 'NONE',  ( -35.50000000000000711, -114.9656200615856818, 10.26631071845107179 ) ) ;
#24019 = CARTESIAN_POINT ( 'NONE',  ( -39.49999999999999289, -5.633167542791597704, 121.0048025873810218 ) ) ;
#24020 = EDGE_CURVE ( 'NONE', #14643, #12235, #15234, .T. ) ;
#24021 = ORIENTED_EDGE ( 'NONE', *, *, #17854, .F. ) ;
#24022 = PLANE ( 'NONE',  #370 ) ;
#24023 = CARTESIAN_POINT ( 'NONE',  ( -35.50000000000000000, -113.4307644833805142, -2.624782352598442614 ) ) ;
#24024 = VERTEX_POINT ( 'NONE', #9846 ) ;
#24025 = ORIENTED_EDGE ( 'NONE', *, *, #34831, .T. ) ;
#24026 = CARTESIAN_POINT ( 'NONE',  ( -36.64504884055823908, -115.0245472910329880, 6.284774454178449155 ) ) ;
#24027 = VECTOR ( 'NONE', #2618, 1000.000000000000000 ) ;
#24028 = FACE_OUTER_BOUND ( 'NONE', #25164, .T. ) ;
#24029 = ORIENTED_EDGE ( 'NONE', *, *, #6214, .T. ) ;
#24030 = EDGE_LOOP ( 'NONE', ( #13701, #24839, #23976, #10293 ) ) ;
#24031 = CARTESIAN_POINT ( 'NONE',  ( -34.50000000000000000, -113.0140978167138712, -0.1247823525984260717 ) ) ;
#24032 = AXIS2_PLACEMENT_3D ( 'NONE', #21712, #19188, #13447 ) ;
#24033 = EDGE_CURVE ( 'NONE', #34564, #4231, #2545, .T. ) ;
#24034 = EDGE_CURVE ( 'NONE', #25299, #32530, #1944, .T. ) ;
#24035 = ADVANCED_FACE ( 'NONE', ( #15587 ), #20811, .T. ) ;
#24036 = CYLINDRICAL_SURFACE ( 'NONE', #3990, 4.000000000000014211 ) ;
#24037 = AXIS2_PLACEMENT_3D ( 'NONE', #1077, #34020, #19945 ) ;
#24038 = CARTESIAN_POINT ( 'NONE',  ( -37.49999999999999289, -12.47865190846804495, 110.2774766518096925 ) ) ;
#24039 = CIRCLE ( 'NONE', #10823, 19.99999999999998579 ) ;
#24040 = CARTESIAN_POINT ( 'NONE',  ( -37.34375000000001421, -114.9929510916434339, 13.11852480586264669 ) ) ;
#24041 = CYLINDRICAL_SURFACE ( 'NONE', #17259, 20.00000000000000355 ) ;
#24042 = DIRECTION ( 'NONE',  ( 0.000000000000000000, 0.000000000000000000, 1.000000000000000000 ) ) ;
#24043 = ADVANCED_FACE ( 'NONE', ( #31999 ), #6795, .F. ) ;
#24044 = VECTOR ( 'NONE', #21204, 1000.000000000000000 ) ;
#24045 = CARTESIAN_POINT ( 'NONE',  ( -34.50000000000000000, -112.0141059978162019, -0.6575071456984691309 ) ) ;
#24046 = EDGE_CURVE ( 'NONE', #19124, #26081, #23808, .T. ) ;
#24047 = DIRECTION ( 'NONE',  ( -1.047965281155519667E-16, -6.938893903907192632E-17, -1.000000000000000000 ) ) ;
#24048 = DIRECTION ( 'NONE',  ( 0.000000000000000000, 0.000000000000000000, -1.000000000000000000 ) ) ;
#24049 = DIRECTION ( 'NONE',  ( -1.000000000000000000, 0.000000000000000000, 0.000000000000000000 ) ) ;
#24050 = VERTEX_POINT ( 'NONE', #1401 ) ;
#24051 = CARTESIAN_POINT ( 'NONE',  ( -37.37500000000009237, -115.9929510916434481, 13.11852480586264846 ) ) ;
#24052 = CARTESIAN_POINT ( 'NONE',  ( -35.50000000000000711, -112.9486715495423681, -1.623175561345890472 ) ) ;
#24053 = CYLINDRICAL_SURFACE ( 'NONE', #26627, 8.000000000000001776 ) ;
#24054 = CYLINDRICAL_SURFACE ( 'NONE', #27985, 13.99999999999999822 ) ;
#24055 = AXIS2_PLACEMENT_3D ( 'NONE', #15689, #12477, #13019 ) ;
#24056 = ORIENTED_EDGE ( 'NONE', *, *, #31132, .F. ) ;
#24057 = DIRECTION ( 'NONE',  ( -1.000000000000000000, 0.000000000000000000, 0.000000000000000000 ) ) ;
#24058 = CARTESIAN_POINT ( 'NONE',  ( 0.000000000000000000, 47.49120266317496686, 0.8606222198176832761 ) ) ;
#24059 = DIRECTION ( 'NONE',  ( -1.000000000000000000, -0.000000000000000000, 0.000000000000000000 ) ) ;
#24060 = CARTESIAN_POINT ( 'NONE',  ( 0.000000000000000000, -11.19999565274257414, 10.71350075272070512 ) ) ;
#24061 = AXIS2_PLACEMENT_3D ( 'NONE', #15099, #1626, #31514 ) ;
#24062 = CARTESIAN_POINT ( 'NONE',  ( -37.47347596530441649, -114.9754527089670262, 7.972274454178450043 ) ) ;
#24063 = DIRECTION ( 'NONE',  ( -1.000000000000000000, 0.000000000000000000, 0.000000000000000000 ) ) ;
#24064 = CARTESIAN_POINT ( 'NONE',  ( 2.321707774797385326, -4.824281976788927118, 0.000000000000000000 ) ) ;
#24065 = ADVANCED_FACE ( 'NONE', ( #1584 ), #26071, .T. ) ;
#24066 = ORIENTED_EDGE ( 'NONE', *, *, #8362, .F. ) ;
#24067 = ORIENTED_EDGE ( 'NONE', *, *, #5044, .T. ) ;
#24068 = CIRCLE ( 'NONE', #14838, 5.000000000000004441 ) ;
#24069 = DIRECTION ( 'NONE',  ( 0.000000000000000000, 0.000000000000000000, 1.000000000000000000 ) ) ;
#24070 = DIRECTION ( 'NONE',  ( 0.000000000000000000, 0.000000000000000000, 1.000000000000000000 ) ) ;
#24071 = EDGE_CURVE ( 'NONE', #32406, #17996, #32178, .T. ) ;
#24072 = CYLINDRICAL_SURFACE ( 'NONE', #7612, 3.999999999999993339 ) ;
#24073 = ORIENTED_EDGE ( 'NONE', *, *, #33806, .T. ) ;
#24074 = CARTESIAN_POINT ( 'NONE',  ( -38.99999999999999289, -114.0592624029313242, 7.746475545821551734 ) ) ;
#24075 = VERTEX_POINT ( 'NONE', #26785 ) ;
#24076 = EDGE_CURVE ( 'NONE', #18374, #984, #15143, .T. ) ;
#24077 = CIRCLE ( 'NONE', #13148, 8.000000000000008882 ) ;
#24078 = ORIENTED_EDGE ( 'NONE', *, *, #12388, .F. ) ;
#24079 = VERTEX_POINT ( 'NONE', #19315 ) ;
#24080 = DIRECTION ( 'NONE',  ( -1.000000000000000000, 0.000000000000000000, 0.000000000000000000 ) ) ;
#24081 = EDGE_CURVE ( 'NONE', #5415, #9277, #5960, .T. ) ;
#24082 = EDGE_CURVE ( 'NONE', #14603, #7064, #8337, .T. ) ;
#24083 = CARTESIAN_POINT ( 'NONE',  ( 8.000000000000007105, 0.000000000000000000, 0.000000000000000000 ) ) ;
#24084 = ORIENTED_EDGE ( 'NONE', *, *, #2972, .T. ) ;
#24085 = ORIENTED_EDGE ( 'NONE', *, *, #25939, .F. ) ;
#24086 = LINE ( 'NONE', #32169, #8730 ) ;
#24087 = PLANE ( 'NONE',  #6275 ) ;
#24088 = DIRECTION ( 'NONE',  ( 3.469446951953614682E-16, -1.000000000000000000, 0.000000000000000000 ) ) ;
#24089 = VECTOR ( 'NONE', #12326, 1000.000000000000000 ) ;
#24090 = CARTESIAN_POINT ( 'NONE',  ( 1.799999999999996048, 0.000000000000000000, 0.000000000000000000 ) ) ;
#24091 = FACE_OUTER_BOUND ( 'NONE', #17523, .T. ) ;
#24092 = VECTOR ( 'NONE', #9797, 1000.000000000000000 ) ;
#24093 = DIRECTION ( 'NONE',  ( -1.000000000000000000, 0.000000000000000000, 0.000000000000000000 ) ) ;
#24094 = CARTESIAN_POINT ( 'NONE',  ( -36.94073759706868287, -112.0000000000000142, 7.128524454178449155 ) ) ;
#24095 = CARTESIAN_POINT ( 'NONE',  ( -34.50481333282507279, -115.9929510916434481, 12.74107470552716315 ) ) ;
#24096 = DIRECTION ( 'NONE',  ( -1.000000000000000000, 0.000000000000000000, 0.000000000000000000 ) ) ;
#24097 = DIRECTION ( 'NONE',  ( 1.000000000000000000, 0.000000000000000000, 0.000000000000000000 ) ) ;
#24098 = DIRECTION ( 'NONE',  ( -9.178431089824344374E-17, 6.938893903907203726E-17, 1.000000000000000000 ) ) ;
#24099 = DIRECTION ( 'NONE',  ( -1.000000000000000000, 1.110223024625156540E-16, 0.000000000000000000 ) ) ;
#24100 = CARTESIAN_POINT ( 'NONE',  ( -10.00000000000000000, 0.000000000000000000, 0.000000000000000000 ) ) ;
#24101 =( NAMED_UNIT ( * ) PLANE_ANGLE_UNIT ( ) SI_UNIT ( $, .RADIAN. ) );
#24102 = ORIENTED_EDGE ( 'NONE', *, *, #12850, .T. ) ;
#24103 = CARTESIAN_POINT ( 'NONE',  ( -39.97545270896702618, -115.3019030900506152, 9.152725545821551734 ) ) ;
#24104 = CARTESIAN_POINT ( 'NONE',  ( 7.999999999999992895, -3.840921266750157326, 47.34345070675169609 ) ) ;
#24105 = CARTESIAN_POINT ( 'NONE',  ( 0.000000000000000000, 0.000000000000000000, 0.000000000000000000 ) ) ;
#24106 = ADVANCED_FACE ( 'NONE', ( #25272 ), #73, .T. ) ;
#24107 = EDGE_LOOP ( 'NONE', ( #26093, #7564, #1479, #2594, #31223, #20661, #13479, #19807, #20791, #10452, #19998, #18714, #13179, #32161, #9337, #14599, #12720, #985, #12033, #16283, #11250, #17310, #18717, #30067, #7223, #25017, #28956, #20932, #20333, #10460, #17085, #268, #6290, #23427, #19184, #21971, #23570, #23032, #6639, #29803, #16740, #25338, #4230, #16261, #24271, #29423, #33111, #2849, #5993, #25943, #30205, #22432, #12043, #7488, #32654, #18696, #27392, #11853, #12219, #18860, #19953, #8611, #12989, #15375, #1215, #26775, #17980, #21545, #7691, #27014, #4130, #7299, #20949, #17325, #24859, #32544, #32536 ) ) ;
#24108 = VERTEX_POINT ( 'NONE', #4998 ) ;
#24109 = EDGE_CURVE ( 'NONE', #4840, #25508, #8267, .T. ) ;
#24110 = CARTESIAN_POINT ( 'NONE',  ( 0.000000000000000000, 42.03146605346819342, -22.12489237027273603 ) ) ;
#24111 = VERTEX_POINT ( 'NONE', #22029 ) ;
#24112 = ORIENTED_EDGE ( 'NONE', *, *, #16719, .T. ) ;
#24113 = CIRCLE ( 'NONE', #14311, 8.000000000000001776 ) ;
#24114 = DIRECTION ( 'NONE',  ( 1.000000000000000000, -0.000000000000000000, -0.000000000000000000 ) ) ;
#24115 = DIRECTION ( 'NONE',  ( 0.000000000000000000, 1.000000000000000000, 0.000000000000000000 ) ) ;
#24116 = DIRECTION ( 'NONE',  ( -1.000000000000000000, 0.000000000000000000, 0.000000000000000000 ) ) ;
#24117 = CARTESIAN_POINT ( 'NONE',  ( 0.000000000000000000, 0.000000000000000000, 0.000000000000000000 ) ) ;
#24118 = ORIENTED_EDGE ( 'NONE', *, *, #12102, .F. ) ;
#24119 = ORIENTED_EDGE ( 'NONE', *, *, #4084, .F. ) ;
#24120 = CARTESIAN_POINT ( 'NONE',  ( -35.50000000000000711, -113.0796441757086939, 1.890140615870383956 ) ) ;
#24121 = DIRECTION ( 'NONE',  ( 1.000000000000000000, 1.734723475976807094E-16, 0.000000000000000000 ) ) ;
#24122 = CYLINDRICAL_SURFACE ( 'NONE', #578, 47.49900000000001654 ) ;
#24123 = ORIENTED_EDGE ( 'NONE', *, *, #4870, .T. ) ;
#24124 = CARTESIAN_POINT ( 'NONE',  ( 7.999999999999992895, 46.77034588191337861, -22.72740077717178053 ) ) ;
#24125 = CARTESIAN_POINT ( 'NONE',  ( -34.50000000000000000, -112.9876085932806262, 1.879154677457530065 ) ) ;
#24126 = CARTESIAN_POINT ( 'NONE',  ( -34.50000000000000000, -114.5636144531578680, 9.676196722963288366 ) ) ;
#24127 = CARTESIAN_POINT ( 'NONE',  ( 7.999999999999992895, 0.000000000000000000, 0.000000000000000000 ) ) ;
#24128 = CARTESIAN_POINT ( 'NONE',  ( -35.99386409314529800, -114.9929510916434339, 13.11852378322482515 ) ) ;
#24129 = CARTESIAN_POINT ( 'NONE',  ( 0.000000000000000000, 0.000000000000000000, 0.000000000000000000 ) ) ;
#24130 = CARTESIAN_POINT ( 'NONE',  ( -34.50000000000000000, -114.9929517792218689, 10.50900788599415314 ) ) ;
#24131 = DIRECTION ( 'NONE',  ( -1.000000000000000000, 0.000000000000000000, 0.000000000000000000 ) ) ;
#24132 = LINE ( 'NONE', #10447, #16675 ) ;
#24133 = DIRECTION ( 'NONE',  ( -1.000000000000000000, 0.000000000000000000, -0.000000000000000000 ) ) ;
#24134 = ORIENTED_EDGE ( 'NONE', *, *, #11488, .T. ) ;
#24135 = DIRECTION ( 'NONE',  ( 0.000000000000000000, 0.000000000000000000, 1.000000000000000000 ) ) ;
#24136 = DIRECTION ( 'NONE',  ( 0.000000000000000000, 0.000000000000000000, 1.000000000000000000 ) ) ;
#24137 = ORIENTED_EDGE ( 'NONE', *, *, #9480, .T. ) ;
#24138 = CARTESIAN_POINT ( 'NONE',  ( -37.56526046546250086, -114.9929510916434339, 13.11451721564129258 ) ) ;
#24139 = VERTEX_POINT ( 'NONE', #25090 ) ;
#24140 = AXIS2_PLACEMENT_3D ( 'NONE', #29495, #34540, #34907 ) ;
#24141 = CARTESIAN_POINT ( 'NONE',  ( -39.07941549657748936, -111.8367748094582055, 2.441024454178448710 ) ) ;
#24142 = CARTESIAN_POINT ( 'NONE',  ( -42.49999999999999289, -26.94801722181404102, 85.25380613764170334 ) ) ;
#24143 = ORIENTED_EDGE ( 'NONE', *, *, #20937, .F. ) ;
#24144 = EDGE_LOOP ( 'NONE', ( #2470, #27330 ) ) ;
#24145 = EDGE_CURVE ( 'NONE', #28086, #26963, #30846, .T. ) ;
#24146 = CYLINDRICAL_SURFACE ( 'NONE', #34716, 17.49900000000000233 ) ;
#24147 = VERTEX_POINT ( 'NONE', #16435 ) ;
#24148 = CARTESIAN_POINT ( 'NONE',  ( -37.05926240293133134, -116.9999999999999858, 4.878524454178448266 ) ) ;
#24149 = FACE_BOUND ( 'NONE', #1355, .T. ) ;
#24150 = DIRECTION ( 'NONE',  ( 0.000000000000000000, 0.000000000000000000, 1.000000000000000000 ) ) ;
#24151 = ORIENTED_EDGE ( 'NONE', *, *, #26055, .F. ) ;
#24152 = ORIENTED_EDGE ( 'NONE', *, *, #16144, .T. ) ;
#24153 = CARTESIAN_POINT ( 'NONE',  ( 70.00001200000001234, -23.52257523363354608, 88.19866736959268394 ) ) ;
#24154 = EDGE_CURVE ( 'NONE', #11680, #9813, #5833, .T. ) ;
#24155 = CARTESIAN_POINT ( 'NONE',  ( 50.00005079999999680, 6.071532165918824830E-15, 1.000000000000000000 ) ) ;
#24156 = EDGE_LOOP ( 'NONE', ( #19, #9297, #6662, #1713 ) ) ;
#24157 = ORIENTED_EDGE ( 'NONE', *, *, #34559, .F. ) ;
#24158 = CIRCLE ( 'NONE', #29349, 10.00000000000000000 ) ;
#24159 = CARTESIAN_POINT ( 'NONE',  ( -34.50000000000000000, -111.0140978167138570, 0.7502176474015694874 ) ) ;
#24160 = CARTESIAN_POINT ( 'NONE',  ( 44.00000000000000000, 1.616533774874506480E-14, 0.000000000000000000 ) ) ;
#24161 = CIRCLE ( 'NONE', #4594, 4.000000000000000000 ) ;
#24162 = VERTEX_POINT ( 'NONE', #13932 ) ;
#24163 = CIRCLE ( 'NONE', #30488, 52.00000000000000711 ) ;
#24164 = CARTESIAN_POINT ( 'NONE',  ( -35.50000000000000711, -114.1414532730574507, 9.517316564499758158 ) ) ;
#24165 = CARTESIAN_POINT ( 'NONE',  ( -34.50000000000000000, -113.9465028010160381, 10.50071319044726081 ) ) ;
#24166 = FACE_OUTER_BOUND ( 'NONE', #22621, .T. ) ;
#24167 = FACE_OUTER_BOUND ( 'NONE', #28610, .T. ) ;
#24168 = CARTESIAN_POINT ( 'NONE',  ( -37.98402046630260287, -113.9929510916434339, 12.74811950270164296 ) ) ;
#24169 = CARTESIAN_POINT ( 'NONE',  ( -37.49414064056232831, -115.9929510916434481, 13.11852578240983291 ) ) ;
#24170 = CARTESIAN_POINT ( 'NONE',  ( 7.999999999999992895, -42.41764978026620270, 20.20639853260275487 ) ) ;
#24171 =( REPRESENTATION_RELATIONSHIP ('NONE','NONE', #26607, #2005 ) REPRESENTATION_RELATIONSHIP_WITH_TRANSFORMATION ( #18049 )SHAPE_REPRESENTATION_RELATIONSHIP( ) );
#24172 = DIRECTION ( 'NONE',  ( 0.000000000000000000, 0.2538061376417690140, 0.9672551082808337197 ) ) ;
#24173 = ORIENTED_EDGE ( 'NONE', *, *, #9885, .T. ) ;
#24174 = CIRCLE ( 'NONE', #8632, 47.49900000000002365 ) ;
#24175 = DIRECTION ( 'NONE',  ( 1.000000000000000000, -5.339440136655842133E-16, -1.047965281155519420E-16 ) ) ;
#24176 = CARTESIAN_POINT ( 'NONE',  ( 8.000000000000000000, 0.000000000000000000, 0.000000000000000000 ) ) ;
#24177 = LINE ( 'NONE', #2581, #22030 ) ;
#24178 = ORIENTED_EDGE ( 'NONE', *, *, #17150, .T. ) ;
#24179 = CIRCLE ( 'NONE', #1741, 7.199999999999993072 ) ;
#24180 = CARTESIAN_POINT ( 'NONE',  ( 5.400000000000003020, 1.000000000000000888, 38.00000000000000000 ) ) ;
#24181 = EDGE_CURVE ( 'NONE', #7811, #23706, #14574, .T. ) ;
#24182 = CARTESIAN_POINT ( 'NONE',  ( -35.50000000000000711, -115.9821387493194891, -0.8839717462762166633 ) ) ;
#24183 = FACE_OUTER_BOUND ( 'NONE', #25029, .T. ) ;
#24184 = EDGE_CURVE ( 'NONE', #8054, #33836, #16295, .T. ) ;
#24185 = CIRCLE ( 'NONE', #8642, 9.499000000000009436 ) ;
#24186 = AXIS2_PLACEMENT_3D ( 'NONE', #26326, #20545, #10102 ) ;
#24187 = CARTESIAN_POINT ( 'NONE',  ( -35.50000000000000711, -114.9929510916434339, 10.72628538622835670 ) ) ;
#24188 = FACE_OUTER_BOUND ( 'NONE', #12069, .T. ) ;
#24189 = ORIENTED_EDGE ( 'NONE', *, *, #19318, .T. ) ;
#24190 = DIRECTION ( 'NONE',  ( 0.000000000000000000, 1.000000000000000000, 0.000000000000000000 ) ) ;
#24191 = CARTESIAN_POINT ( 'NONE',  ( -35.50000000000000000, -112.8230659962028994, 2.866612799894348029 ) ) ;
#24192 = VERTEX_POINT ( 'NONE', #17146 ) ;
#24193 = ORIENTED_EDGE ( 'NONE', *, *, #18304, .T. ) ;
#24194 = CARTESIAN_POINT ( 'NONE',  ( -36.25098837183129774, -113.3347980657956242, 7.316024454178450043 ) ) ;
#24195 = EDGE_CURVE ( 'NONE', #20493, #4537, #9994, .T. ) ;
#24196 = DIRECTION ( 'NONE',  ( 1.000000000000000000, -0.000000000000000000, -0.000000000000000000 ) ) ;
#24197 = ORIENTED_EDGE ( 'NONE', *, *, #15650, .T. ) ;
#24198 = ORIENTED_EDGE ( 'NONE', *, *, #14848, .F. ) ;
#24199 = EDGE_CURVE ( 'NONE', #11194, #9658, #33005, .T. ) ;
#24200 = CARTESIAN_POINT ( 'NONE',  ( -34.50000000000000000, -113.0140978167138712, -0.5622823525984297355 ) ) ;
#24201 = AXIS2_PLACEMENT_3D ( 'NONE', #3406, #14886, #19916 ) ;
#24202 = DIRECTION ( 'NONE',  ( 1.000000000000000000, 0.000000000000000000, -1.691777834109591064E-31 ) ) ;
#24203 = DIRECTION ( 'NONE',  ( 0.000000000000000000, 0.000000000000000000, -1.000000000000000000 ) ) ;
#24204 = CARTESIAN_POINT ( 'NONE',  ( -38.00000000000000711, -114.9929510916434339, 11.91443571948719615 ) ) ;
#24205 = DIRECTION ( 'NONE',  ( 0.000000000000000000, -1.000000000000000000, -1.048062100069320848E-14 ) ) ;
#24206 = LINE ( 'NONE', #8332, #32035 ) ;
#24207 =( GEOMETRIC_REPRESENTATION_CONTEXT ( 3 ) GLOBAL_UNCERTAINTY_ASSIGNED_CONTEXT ( ( #33720 ) ) GLOBAL_UNIT_ASSIGNED_CONTEXT ( ( #21507, #18645, #2641 ) ) REPRESENTATION_CONTEXT ( 'NONE', 'WORKASPACE' ) );
#24208 = VECTOR ( 'NONE', #12095, 1000.000000000000000 ) ;
#24209 = CARTESIAN_POINT ( 'NONE',  ( -34.50000000000000000, -112.0250551866464548, 1.025914454044489332 ) ) ;
#24210 = ADVANCED_FACE ( 'NONE', ( #13762 ), #21356, .T. ) ;
#24211 =( GEOMETRIC_REPRESENTATION_CONTEXT ( 3 ) GLOBAL_UNCERTAINTY_ASSIGNED_CONTEXT ( ( #5907 ) ) GLOBAL_UNIT_ASSIGNED_CONTEXT ( ( #19257, #34198, #17793 ) ) REPRESENTATION_CONTEXT ( 'NONE', 'WORKASPACE' ) );
#24212 = CARTESIAN_POINT ( 'NONE',  ( 2.141980652367342586, -6.189445006155629869, -0.7999999999999951594 ) ) ;
#24213 = PRODUCT_DEFINITION_SHAPE ( 'NONE', 'NONE',  #35648 ) ;
#24214 = CARTESIAN_POINT ( 'NONE',  ( -34.49999999999998579, -20.32009476567218798, 72.19543654875879213 ) ) ;
#24215 = ORIENTED_EDGE ( 'NONE', *, *, #31764, .F. ) ;
#24216 = CARTESIAN_POINT ( 'NONE',  ( -35.50000000000000711, -114.1068310684433129, 9.512752019463897923 ) ) ;
#24217 = CARTESIAN_POINT ( 'NONE',  ( 8.000000000000000000, -14.87816164169118416, 4.342730381189816136 ) ) ;
#24218 = FACE_OUTER_BOUND ( 'NONE', #12863, .T. ) ;
#24219 = DIRECTION ( 'NONE',  ( 1.000000000000000000, -5.339440136655842133E-16, -1.047965281155519420E-16 ) ) ;
#24220 = CARTESIAN_POINT ( 'NONE',  ( 0.000000000000000000, 0.000000000000000000, 0.000000000000000000 ) ) ;
#24221 = ORIENTED_EDGE ( 'NONE', *, *, #19490, .F. ) ;
#24222 = FACE_OUTER_BOUND ( 'NONE', #26907, .T. ) ;
#24223 = DIRECTION ( 'NONE',  ( -1.000000000000000000, 0.000000000000000000, 0.000000000000000000 ) ) ;
#24224 = EDGE_CURVE ( 'NONE', #8679, #9355, #12306, .T. ) ;
#24225 = DIRECTION ( 'NONE',  ( -1.000000000000000000, 0.000000000000000000, 0.000000000000000000 ) ) ;
#24226 = LINE ( 'NONE', #29276, #8078 ) ;
#24227 = ADVANCED_FACE ( 'NONE', ( #19661 ), #6006, .T. ) ;
#24228 = CIRCLE ( 'NONE', #635, 20.00000000000000000 ) ;
#24229 = ADVANCED_FACE ( 'NONE', ( #6187, #28151 ), #11230, .F. ) ;
#24230 = FACE_BOUND ( 'NONE', #19820, .T. ) ;
#24231 = CARTESIAN_POINT ( 'NONE',  ( 5.400000000000085620, -1.000000000000049516, -44.50000000000000000 ) ) ;
#24232 = ORIENTED_EDGE ( 'NONE', *, *, #15449, .T. ) ;
#24233 = EDGE_LOOP ( 'NONE', ( #17933, #8191, #9084, #10979 ) ) ;
#24234 = CARTESIAN_POINT ( 'NONE',  ( 46.00000000000000000, 0.000000000000000000, 70.00000000000000000 ) ) ;
#24235 = DIRECTION ( 'NONE',  ( 0.000000000000000000, 0.000000000000000000, 1.000000000000000000 ) ) ;
#24236 = FACE_OUTER_BOUND ( 'NONE', #28228, .T. ) ;
#24237 = EDGE_LOOP ( 'NONE', ( #10079, #30207, #317, #12362 ) ) ;
#24238 = CARTESIAN_POINT ( 'NONE',  ( -37.88768952767750875, -112.0245472910329880, 8.027725545821549957 ) ) ;
#24239 = EDGE_CURVE ( 'NONE', #12895, #574, #24397, .T. ) ;
#24240 = ORIENTED_EDGE ( 'NONE', *, *, #27776, .T. ) ;
#24241 = CIRCLE ( 'NONE', #14440, 20.00000000000000711 ) ;
#24242 = AXIS2_PLACEMENT_3D ( 'NONE', #24117, #10058, #18515 ) ;
#24243 = EDGE_CURVE ( 'NONE', #34165, #20385, #7696, .T. ) ;
#24244 =( NAMED_UNIT ( * ) PLANE_ANGLE_UNIT ( ) SI_UNIT ( $, .RADIAN. ) );
#24245 = ORIENTED_EDGE ( 'NONE', *, *, #3, .T. ) ;
#24246 = ORIENTED_EDGE ( 'NONE', *, *, #16951, .T. ) ;
#24247 = ADVANCED_FACE ( 'NONE', ( #6708 ), #9770, .T. ) ;
#24248 = FACE_OUTER_BOUND ( 'NONE', #18449, .T. ) ;
#24249 = CARTESIAN_POINT ( 'NONE',  ( -46.00000000000000000, -25.98076211353320275, 76.99999999999992895 ) ) ;
#24250 = VERTEX_POINT ( 'NONE', #14813 ) ;
#24251 = ORIENTED_EDGE ( 'NONE', *, *, #522, .F. ) ;
#24252 = CARTESIAN_POINT ( 'NONE',  ( 0.000000000000000000, -2.710505431213761085E-17, -46.00000000000000000 ) ) ;
#24253 = CARTESIAN_POINT ( 'NONE',  ( 7.999999999999992895, 0.000000000000000000, 0.000000000000000000 ) ) ;
#24254 = DIRECTION ( 'NONE',  ( 0.000000000000000000, 0.000000000000000000, -1.000000000000000000 ) ) ;
#24255 = ADVANCED_FACE ( 'NONE', ( #1311 ), #14979, .F. ) ;
#24256 = FACE_OUTER_BOUND ( 'NONE', #29932, .T. ) ;
#24257 = DIRECTION ( 'NONE',  ( -1.000000000000000000, 0.000000000000000000, -0.000000000000000000 ) ) ;
#24258 = PRODUCT_DEFINITION ( 'UNKNOWN', '', #15498, #17678 ) ;
#24259 = CARTESIAN_POINT ( 'NONE',  ( -36.23083527818513261, -116.0245472910329880, 6.284774454178449155 ) ) ;
#24261 = EDGE_CURVE ( 'NONE', #30356, #19767, #10022, .T. ) ;
#24260 = TOROIDAL_SURFACE ( 'NONE', #11022, 5.015999999999992909, 0.04099999999999925926 ) ;
#24262 =( GEOMETRIC_REPRESENTATION_CONTEXT ( 3 ) GLOBAL_UNCERTAINTY_ASSIGNED_CONTEXT ( ( #16852 ) ) GLOBAL_UNIT_ASSIGNED_CONTEXT ( ( #1291, #23620, #23248 ) ) REPRESENTATION_CONTEXT ( 'NONE', 'WORKASPACE' ) );
#24263 = CARTESIAN_POINT ( 'NONE',  ( -34.50000000000000000, -115.9792481177720731, 10.26484292309424795 ) ) ;
#24265 = CARTESIAN_POINT ( 'NONE',  ( 0.000000000000000000, -46.87740477351715640, -3.172455868805712509 ) ) ;
#24264 = CIRCLE ( 'NONE', #28265, 4.000000000000000000 ) ;
#24266 = DIRECTION ( 'NONE',  ( 0.000000000000000000, 0.3090169943749477288, -0.9510565162951534202 ) ) ;
#24267 = LINE ( 'NONE', #35254, #14734 ) ;
#24268 = DIRECTION ( 'NONE',  ( 1.000000000000000000, -0.000000000000000000, 0.000000000000000000 ) ) ;
#24269 = DIRECTION ( 'NONE',  ( 1.084202172485500613E-16, -6.938893903907203726E-17, -1.000000000000000000 ) ) ;
#24270 = SURFACE_STYLE_USAGE ( .BOTH. , #29666 ) ;
#24271 = ORIENTED_EDGE ( 'NONE', *, *, #31688, .F. ) ;
#24272 = EDGE_CURVE ( 'NONE', #32986, #34870, #31562, .T. ) ;
#24273 = EDGE_CURVE ( 'NONE', #24979, #32647, #2021, .T. ) ;
#24274 = CARTESIAN_POINT ( 'NONE',  ( -35.69809690994941320, -116.9754527089670546, 8.777725545821549957 ) ) ;
#24275 = CARTESIAN_POINT ( 'NONE',  ( -39.49999999999999289, -3.734562119078923992, 144.3977620171895637 ) ) ;
#24276 = FACE_OUTER_BOUND ( 'NONE', #20552, .T. ) ;
#24277 = CARTESIAN_POINT ( 'NONE',  ( 7.999999999999992895, -42.60732521687585006, 19.80331771201643321 ) ) ;
#24278 = VERTEX_POINT ( 'NONE', #1490 ) ;
#24279 = ORIENTED_EDGE ( 'NONE', *, *, #3862, .T. ) ;
#24280 = CARTESIAN_POINT ( 'NONE',  ( 46.00000000000000000, 0.000000000000000000, 70.00000000000000000 ) ) ;
#24281 = CARTESIAN_POINT ( 'NONE',  ( -21.15833593587365513, -42.98076211353323828, 83.49999999999991473 ) ) ;
#24282 = VERTEX_POINT ( 'NONE', #9594 ) ;
#24283 = ORIENTED_EDGE ( 'NONE', *, *, #27645, .F. ) ;
#24284 = ADVANCED_FACE ( 'NONE', ( #9235 ), #22911, .T. ) ;
#24285 = DIRECTION ( 'NONE',  ( 0.000000000000000000, 0.8660254037844398178, -0.4999999999999981681 ) ) ;
#24286 = CARTESIAN_POINT ( 'NONE',  ( -38.45611840935523418, -112.6276912846090568, 9.433975545821551734 ) ) ;
#24287 = CIRCLE ( 'NONE', #29451, 1.000000000000000444 ) ;
#24288 = VECTOR ( 'NONE', #13961, 1000.000000000000000 ) ;
#24289 = DIRECTION ( 'NONE',  ( 0.000000000000000000, 0.000000000000000000, 1.000000000000000000 ) ) ;
#24290 = CARTESIAN_POINT ( 'NONE',  ( -3.799999999999999822, 0.000000000000000000, -33.50000000000000711 ) ) ;
#24291 = VERTEX_POINT ( 'NONE', #20563 ) ;
#24292 = ORIENTED_EDGE ( 'NONE', *, *, #14477, .F. ) ;
#24293 = CARTESIAN_POINT ( 'NONE',  ( -35.50000000000000711, -112.3995503592287690, -1.424448457485529618 ) ) ;
#24294 = CARTESIAN_POINT ( 'NONE',  ( 7.999999999999992895, 1.347111479062088405E-15, -11.00000000000000000 ) ) ;
#24295 = CYLINDRICAL_SURFACE ( 'NONE', #29333, 3.999999999999996447 ) ;
#24296 = EDGE_LOOP ( 'NONE', ( #4679, #34548, #10946, #4504 ) ) ;
#24297 = DIRECTION ( 'NONE',  ( 0.000000000000000000, 0.000000000000000000, 1.000000000000000000 ) ) ;
#24298 = EDGE_CURVE ( 'NONE', #4943, #14725, #960, .T. ) ;
#24299 = CARTESIAN_POINT ( 'NONE',  ( -34.50000000000000000, -112.0140978167138712, -0.4997823525984337878 ) ) ;
#24300 = ADVANCED_FACE ( 'NONE', ( #22730 ), #15150, .T. ) ;
#24301 = CARTESIAN_POINT ( 'NONE',  ( -35.98977351030467986, -114.9929510916434339, 14.11852173794918386 ) ) ;
#24302 = ADVANCED_FACE ( 'NONE', ( #28325 ), #12474, .T. ) ;
#24303 = DIRECTION ( 'NONE',  ( 1.174092375852890260E-15, -4.222049128630259891E-16, -1.000000000000000000 ) ) ;
#24304 = CARTESIAN_POINT ( 'NONE',  ( -35.50000000000000000, -113.9813390189866027, 10.50487145766371100 ) ) ;
#24305 = DIRECTION ( 'NONE',  ( -1.000000000000000000, -0.000000000000000000, -0.000000000000000000 ) ) ;
#24306 = CARTESIAN_POINT ( 'NONE',  ( -34.50000000000000000, -114.0998638248492085, 9.511920366020609308 ) ) ;
#24307 = FACE_OUTER_BOUND ( 'NONE', #10599, .T. ) ;
#24308 = CARTESIAN_POINT ( 'NONE',  ( -38.00000000000000711, -114.9929510916434339, 12.53051367006571937 ) ) ;
#24309 = ORIENTED_EDGE ( 'NONE', *, *, #24239, .T. ) ;
#24310 = DIRECTION ( 'NONE',  ( 0.000000000000000000, -1.000000000000000000, 0.000000000000000000 ) ) ;
#24311 = CARTESIAN_POINT ( 'NONE',  ( 8.000000000000000000, -18.48663108841356717, -3.384281271888017084 ) ) ;
#24312 = ORIENTED_EDGE ( 'NONE', *, *, #30173, .T. ) ;
#24313 = CARTESIAN_POINT ( 'NONE',  ( -37.37500000000009237, -114.9929510916434339, 13.11852480586264669 ) ) ;
#24314 = VERTEX_POINT ( 'NONE', #772 ) ;
#24315 = ADVANCED_FACE ( 'NONE', ( #31378 ), #17862, .T. ) ;
#24316 = VECTOR ( 'NONE', #24737, 1000.000000000000000 ) ;
#24317 = CARTESIAN_POINT ( 'NONE',  ( -35.62769128460905677, -115.4561184093552413, 6.191024454178448266 ) ) ;
#24318 = EDGE_CURVE ( 'NONE', #16181, #26147, #31911, .T. ) ;
#24319 = DIRECTION ( 'NONE',  ( -1.000000000000000000, -1.836970198721029934E-16, -0.000000000000000000 ) ) ;
#24320 = ORIENTED_EDGE ( 'NONE', *, *, #5249, .T. ) ;
#24321 = ORIENTED_EDGE ( 'NONE', *, *, #15804, .F. ) ;
#24322 = DIRECTION ( 'NONE',  ( -1.000000000000000000, -0.000000000000000000, -0.000000000000000000 ) ) ;
#24323 = CYLINDRICAL_SURFACE ( 'NONE', #24380, 8.000000000000001776 ) ;
#24324 = VERTEX_POINT ( 'NONE', #34085 ) ;
#24325 = CARTESIAN_POINT ( 'NONE',  ( -34.97545270896703329, -113.2308352781851539, 8.909774454178450043 ) ) ;
#24326 = AXIS2_PLACEMENT_3D ( 'NONE', #7067, #15155, #12296 ) ;
#24327 = CIRCLE ( 'NONE', #19688, 8.000000000000005329 ) ;
#24328 = DIRECTION ( 'NONE',  ( -1.000000000000000000, 0.000000000000000000, -0.000000000000000000 ) ) ;
#24329 = LINE ( 'NONE', #13520, #10790 ) ;
#24331 = ORIENTED_EDGE ( 'NONE', *, *, #7688, .F. ) ;
#24330 = CIRCLE ( 'NONE', #3048, 3.799999999999999822 ) ;
#24332 = ORIENTED_EDGE ( 'NONE', *, *, #2752, .F. ) ;
#24333 = CARTESIAN_POINT ( 'NONE',  ( 70.00001200000001234, -22.78209474394047973, 82.54181312010027227 ) ) ;
#24334 = DIRECTION ( 'NONE',  ( -1.000000000000000000, 0.000000000000000000, 0.000000000000000000 ) ) ;
#24335 = EDGE_LOOP ( 'NONE', ( #18341, #31188, #8548, #16711 ) ) ;
#24336 = ORIENTED_EDGE ( 'NONE', *, *, #25832, .T. ) ;
#24337 = CARTESIAN_POINT ( 'NONE',  ( -34.50000000000000000, -111.0140821919084715, 0.8283428459075261596 ) ) ;
#24338 = FACE_OUTER_BOUND ( 'NONE', #10459, .T. ) ;
#24339 = VECTOR ( 'NONE', #30697, 1000.000000000000000 ) ;
#24340 = ORIENTED_EDGE ( 'NONE', *, *, #11216, .F. ) ;
#24341 = CARTESIAN_POINT ( 'NONE',  ( -35.50000000000000711, -114.1712995509219724, 9.522174004479579068 ) ) ;
#24342 = EDGE_CURVE ( 'NONE', #7666, #22879, #2049, .T. ) ;
#24343 = CARTESIAN_POINT ( 'NONE',  ( -34.50000000000000000, -113.9929510916434339, 10.50625754673609258 ) ) ;
#24344 = CARTESIAN_POINT ( 'NONE',  ( 70.00000000000001421, 58.35354061212520804, 76.25822877525452270 ) ) ;
#24345 = FACE_BOUND ( 'NONE', #6510, .T. ) ;
#24346 = CARTESIAN_POINT ( 'NONE',  ( -37.80727372874345349, -113.9929510916434339, 13.01835785830664705 ) ) ;
#24347 = CARTESIAN_POINT ( 'NONE',  ( -38.00000000000000711, -115.9929510916434481, 12.60752341388803721 ) ) ;
#24348 = FACE_OUTER_BOUND ( 'NONE', #17043, .T. ) ;
#24349 = CIRCLE ( 'NONE', #7648, 52.00000000000000711 ) ;
#24350 = AXIS2_PLACEMENT_3D ( 'NONE', #29617, #11059, #15726 ) ;
#24351 = DIRECTION ( 'NONE',  ( -1.000000000000000000, 0.000000000000000000, 0.000000000000000000 ) ) ;
#24352 = ORIENTED_EDGE ( 'NONE', *, *, #22127, .T. ) ;
#24353 = CARTESIAN_POINT ( 'NONE',  ( -3.799999999999999822, 4.382607293638566128E-16, -20.99999999999999645 ) ) ;
#24354 = CARTESIAN_POINT ( 'NONE',  ( 0.9999999999999453770, -6.008326913195871199, 0.000000000000000000 ) ) ;
#24355 = CARTESIAN_POINT ( 'NONE',  ( -44.00000000000000000, 0.000000000000000000, 0.000000000000000000 ) ) ;
#24356 = ORIENTED_EDGE ( 'NONE', *, *, #27764, .T. ) ;
#24357 = DIRECTION ( 'NONE',  ( -1.000000000000000000, 0.000000000000000000, 0.000000000000000000 ) ) ;
#24358 = CIRCLE ( 'NONE', #9385, 9.499000000000004107 ) ;
#24359 = AXIS2_PLACEMENT_3D ( 'NONE', #22073, #24963, #22245 ) ;
#24360 = CARTESIAN_POINT ( 'NONE',  ( -35.50000000000000711, -116.0140978167138712, 0.3752176474015736507 ) ) ;
#24361 = CARTESIAN_POINT ( 'NONE',  ( 0.000000000000000000, -2.710505431213761085E-17, 45.00000000000000000 ) ) ;
#24362 = CARTESIAN_POINT ( 'NONE',  ( -35.50000000000000711, -114.9929510916434339, 10.68227981832981044 ) ) ;
#24363 = DIRECTION ( 'NONE',  ( 1.000000000000000000, 0.000000000000000000, 0.000000000000000000 ) ) ;
#24364 = ORIENTED_EDGE ( 'NONE', *, *, #11859, .T. ) ;
#24365 = PLANE ( 'NONE',  #25106 ) ;
#24366 = CARTESIAN_POINT ( 'NONE',  ( -35.50000000000000000, -111.0140978167138570, 0.7502176474015694874 ) ) ;
#24367 = ORIENTED_EDGE ( 'NONE', *, *, #25127, .T. ) ;
#24368 = EDGE_LOOP ( 'NONE', ( #28081, #28269, #3518, #16851 ) ) ;
#24369 = CARTESIAN_POINT ( 'NONE',  ( -34.97545270896703329, -113.2308352781851539, 2.909774454178448710 ) ) ;
#24370 = PRESENTATION_STYLE_ASSIGNMENT (( #21118 ) ) ;
#24371 = CYLINDRICAL_SURFACE ( 'NONE', #22135, 1.000000000000000888 ) ;
#24373 = ORIENTED_EDGE ( 'NONE', *, *, #12808, .T. ) ;
#24372 = AXIS2_PLACEMENT_3D ( 'NONE', #22816, #28410, #6612 ) ;
#24374 = ORIENTED_EDGE ( 'NONE', *, *, #13656, .T. ) ;
#24375 = CARTESIAN_POINT ( 'NONE',  ( -34.50000000000000000, -113.0140978167138712, -0.3122823525984338988 ) ) ;
#24376 = LINE ( 'NONE', #21656, #34418 ) ;
#24377 = FACE_BOUND ( 'NONE', #28473, .T. ) ;
#24378 = DIRECTION ( 'NONE',  ( -1.000000000000000000, 0.000000000000000000, 0.000000000000000000 ) ) ;
#24379 = APPLICATION_CONTEXT ( 'automotive_design' ) ;
#24380 = AXIS2_PLACEMENT_3D ( 'NONE', #24496, #35314, #21591 ) ;
#24381 = EDGE_CURVE ( 'NONE', #19752, #9468, #6037, .T. ) ;
#24382 = CARTESIAN_POINT ( 'NONE',  ( -37.54084996655477369, -114.9929510916434339, 13.11692036158760466 ) ) ;
#24383 = CIRCLE ( 'NONE', #3112, 4.980000000000017302 ) ;
#24384 = CARTESIAN_POINT ( 'NONE',  ( 3.872983346207429900, -1.000000000000003553, 30.00000000000000000 ) ) ;
#24385 = CARTESIAN_POINT ( 'NONE',  ( 7.999999999999992895, 0.000000000000000000, 0.000000000000000000 ) ) ;
#24386 = CARTESIAN_POINT ( 'NONE',  ( -34.50000000000000000, -115.2732872103912030, -1.592823285204062911 ) ) ;
#24387 = DIRECTION ( 'NONE',  ( -1.000000000000000000, 0.000000000000000000, -0.000000000000000000 ) ) ;
#24388 = CIRCLE ( 'NONE', #8845, 13.99999999999999645 ) ;
#24389 = DIRECTION ( 'NONE',  ( -1.000000000000000000, -1.836970198721030181E-16, 0.000000000000000000 ) ) ;
#24390 = ORIENTED_EDGE ( 'NONE', *, *, #11699, .F. ) ;
#24391 = ADVANCED_FACE ( 'NONE', ( #9060 ), #4212, .F. ) ;
#24392 = CARTESIAN_POINT ( 'NONE',  ( -37.51635661748575501, -115.9929510916434481, 13.11827392651459512 ) ) ;
#24393 = CYLINDRICAL_SURFACE ( 'NONE', #1014, 20.00000000000000355 ) ;
#24394 = DIRECTION ( 'NONE',  ( 1.000000000000000000, 1.836970198721029934E-16, 0.000000000000000000 ) ) ;
#24395 = FACE_OUTER_BOUND ( 'NONE', #28029, .T. ) ;
#24396 = LINE ( 'NONE', #26935, #5610 ) ;
#24397 = CIRCLE ( 'NONE', #8854, 11.00000000000000000 ) ;
#24398 = ORIENTED_EDGE ( 'NONE', *, *, #16902, .F. ) ;
#24399 = DIRECTION ( 'NONE',  ( 1.000000000000000000, -5.339440136655838189E-16, 0.000000000000000000 ) ) ;
#24400 = DIRECTION ( 'NONE',  ( 1.000000000000000000, -0.000000000000000000, -0.000000000000000000 ) ) ;
#24401 = DIRECTION ( 'NONE',  ( 0.000000000000000000, 0.4999999999999948375, 0.8660254037844415942 ) ) ;
#24402 = CARTESIAN_POINT ( 'NONE',  ( 30.00000000000000000, 14.30000000000001315, 3.000000000000002665 ) ) ;
#24403 = CARTESIAN_POINT ( 'NONE',  ( 46.00000000000000000, 0.000000000000000000, 70.00000000000000000 ) ) ;
#24404 = DIRECTION ( 'NONE',  ( 1.000000000000000000, -0.000000000000000000, 0.000000000000000000 ) ) ;
#24405 = ORIENTED_EDGE ( 'NONE', *, *, #3921, .T. ) ;
#24406 = ORIENTED_EDGE ( 'NONE', *, *, #21561, .F. ) ;
#24407 = AXIS2_PLACEMENT_3D ( 'NONE', #28428, #3773, #14729 ) ;
#24408 = LINE ( 'NONE', #10192, #4409 ) ;
#24409 = CIRCLE ( 'NONE', #13483, 20.00000000000000711 ) ;
#24410 = CARTESIAN_POINT ( 'NONE',  ( 7.999999999999992895, 0.000000000000000000, 0.000000000000000000 ) ) ;
#24411 = FACE_OUTER_BOUND ( 'NONE', #5449, .T. ) ;
#24412 = ORIENTED_EDGE ( 'NONE', *, *, #4914, .F. ) ;
#24413 = CARTESIAN_POINT ( 'NONE',  ( -35.54388159064475872, -115.3723087153909432, 5.683975545821551734 ) ) ;
#24414 = ORIENTED_EDGE ( 'NONE', *, *, #32019, .T. ) ;
#24415 = EDGE_CURVE ( 'NONE', #14060, #15919, #20732, .T. ) ;
#24416 = ORIENTED_EDGE ( 'NONE', *, *, #702, .T. ) ;
#24417 = EDGE_LOOP ( 'NONE', ( #30820, #14492, #4987, #4412 ) ) ;
#24418 = DIRECTION ( 'NONE',  ( -1.734723475976807094E-16, 0.8660254037844444808, -0.4999999999999898415 ) ) ;
#24419 = CARTESIAN_POINT ( 'NONE',  ( 0.000000000000000000, 44.75336757549778355, 14.30704879393622520 ) ) ;
#24420 = ORIENTED_EDGE ( 'NONE', *, *, #29552, .F. ) ;
#24421 = ORIENTED_EDGE ( 'NONE', *, *, #16294, .F. ) ;
#24422 = EDGE_CURVE ( 'NONE', #15120, #29062, #7752, .T. ) ;
#24423 = DIRECTION ( 'NONE',  ( -1.000000000000000000, 0.000000000000000000, 0.000000000000000000 ) ) ;
#24424 = DIRECTION ( 'NONE',  ( -0.000000000000000000, 0.000000000000000000, -1.000000000000000000 ) ) ;
#24425 = ADVANCED_FACE ( 'NONE', ( #23637 ), #2232, .F. ) ;
#24426 = LINE ( 'NONE', #18838, #3910 ) ;
#24427 = DIRECTION ( 'NONE',  ( -1.000000000000000000, 0.000000000000000000, 0.000000000000000000 ) ) ;
#24428 = DIRECTION ( 'NONE',  ( 0.000000000000000000, -0.2486898871648415554, -0.9685831611286345177 ) ) ;
#24429 = VECTOR ( 'NONE', #24981, 1000.000000000000000 ) ;
#24430 = AXIS2_PLACEMENT_3D ( 'NONE', #33458, #2886, #6094 ) ;
#24431 = CARTESIAN_POINT ( 'NONE',  ( -39.02454729103295961, -114.7691647218148745, 6.659774454178449155 ) ) ;
#24432 = ADVANCED_FACE ( 'NONE', ( #34802 ), #10665, .F. ) ;
#24433 = CARTESIAN_POINT ( 'NONE',  ( -37.54906985245723661, -115.9929510916434481, 14.11777216781844757 ) ) ;
#24434 = DIRECTION ( 'NONE',  ( -1.000000000000000000, 0.000000000000000000, 0.000000000000000000 ) ) ;
#24435 = EDGE_CURVE ( 'NONE', #31659, #3685, #15863, .T. ) ;
#24436 = AXIS2_PLACEMENT_3D ( 'NONE', #33964, #8925, #30902 ) ;
#24437 = DIRECTION ( 'NONE',  ( -0.000000000000000000, 0.000000000000000000, -1.000000000000000000 ) ) ;
#24438 = DIRECTION ( 'NONE',  ( 0.000000000000000000, 0.000000000000000000, 1.000000000000000000 ) ) ;
#24439 = CARTESIAN_POINT ( 'NONE',  ( 7.999999999999992895, 0.000000000000000000, 0.000000000000000000 ) ) ;
#24440 = DIRECTION ( 'NONE',  ( 0.000000000000000000, -1.000000000000000000, 0.000000000000000000 ) ) ;
#24441 =( LENGTH_UNIT ( ) NAMED_UNIT ( * ) SI_UNIT ( .MILLI., .METRE. ) );
#24442 = ORIENTED_EDGE ( 'NONE', *, *, #32103, .F. ) ;
#24443 = CARTESIAN_POINT ( 'NONE',  ( -39.02454729103295961, -113.2308352781851539, 3.340225545821550845 ) ) ;
#24444 = CARTESIAN_POINT ( 'NONE',  ( -39.49999999999999289, -14.67619866229204284, 104.0227405789415371 ) ) ;
#24445 = CARTESIAN_POINT ( 'NONE',  ( 0.000000000000000000, -2.710505431213761085E-17, 45.10000000000000142 ) ) ;
#24446 = DIRECTION ( 'NONE',  ( 0.000000000000000000, 0.000000000000000000, 1.000000000000000000 ) ) ;
#24447 = ORIENTED_EDGE ( 'NONE', *, *, #19277, .T. ) ;
#24448 = AXIS2_PLACEMENT_3D ( 'NONE', #5272, #33331, #24528 ) ;
#24449 = ORIENTED_EDGE ( 'NONE', *, *, #22694, .F. ) ;
#24450 = PRODUCT_DEFINITION_CONTEXT ( 'detailed design', #10554, 'design' ) ;
#24451 = CARTESIAN_POINT ( 'NONE',  ( -39.49999999999999289, -3.784235812937200460, 96.08311962715481513 ) ) ;
#24452 = ORIENTED_EDGE ( 'NONE', *, *, #31327, .F. ) ;
#24453 = EDGE_LOOP ( 'NONE', ( #30105, #1117, #17742, #18330 ) ) ;
#24454 = EDGE_CURVE ( 'NONE', #17379, #31396, #29931, .T. ) ;
#24455 = DIRECTION ( 'NONE',  ( 1.000000000000000000, -4.336808689941997226E-15, -1.084202172485499306E-15 ) ) ;
#24456 = AXIS2_PLACEMENT_3D ( 'NONE', #32360, #5362, #26437 ) ;
#24457 = LINE ( 'NONE', #11129, #14811 ) ;
#24458 = DIRECTION ( 'NONE',  ( -1.095604667390109757E-17, 0.9878381089542525029, -0.1554859173613037659 ) ) ;
#24459 = CIRCLE ( 'NONE', #30797, 8.000000000000000000 ) ;
#24460 = CYLINDRICAL_SURFACE ( 'NONE', #12724, 6.000000000000005329 ) ;
#24461 = ORIENTED_EDGE ( 'NONE', *, *, #19956, .F. ) ;
#24462 = ORIENTED_EDGE ( 'NONE', *, *, #31271, .F. ) ;
#24463 = CARTESIAN_POINT ( 'NONE',  ( -35.50000000000000711, -112.9486715495423681, -1.623175561345890472 ) ) ;
#24464 = CIRCLE ( 'NONE', #29065, 7.199999999999994849 ) ;
#24465 = ADVANCED_FACE ( 'NONE', ( #10125 ), #29403, .T. ) ;
#24466 = CYLINDRICAL_SURFACE ( 'NONE', #29520, 13.99999999999999822 ) ;
#24467 = EDGE_CURVE ( 'NONE', #26822, #18180, #4748, .T. ) ;
#24468 = EDGE_CURVE ( 'NONE', #18507, #20326, #31906, .T. ) ;
#24469 = DIRECTION ( 'NONE',  ( -1.000000000000000000, -0.000000000000000000, 0.000000000000000000 ) ) ;
#24470 = ORIENTED_EDGE ( 'NONE', *, *, #24273, .F. ) ;
#24471 = CARTESIAN_POINT ( 'NONE',  ( 8.000000000000007105, 3.975523202428013381, 13.42368113696675103 ) ) ;
#24472 = AXIS2_PLACEMENT_3D ( 'NONE', #25411, #28816, #26117 ) ;
#24473 = CARTESIAN_POINT ( 'NONE',  ( -34.50000000000000000, -115.2732872103912030, -1.592823285204062911 ) ) ;
#24474 = CARTESIAN_POINT ( 'NONE',  ( -38.95206139890800046, -114.9929510916434339, 13.00730889637963728 ) ) ;
#24475 = CARTESIAN_POINT ( 'NONE',  ( 7.999999999999992895, 11.90021268425617329, -45.45261810511203038 ) ) ;
#24476 = CARTESIAN_POINT ( 'NONE',  ( -35.50000000000000000, -113.9557924591415627, 10.50182206170499555 ) ) ;
#24477 = DIRECTION ( 'NONE',  ( -1.000000000000000000, -0.000000000000000000, -0.000000000000000000 ) ) ;
#24478 = CARTESIAN_POINT ( 'NONE',  ( -35.97545865737298953, -114.9929510916434339, 14.11837420659365705 ) ) ;
#24479 = DIRECTION ( 'NONE',  ( -1.000000000000000000, 0.000000000000000000, 0.000000000000000000 ) ) ;
#24480 = ADVANCED_FACE ( 'NONE', ( #2399 ), #2041, .T. ) ;
#24481 = DIRECTION ( 'NONE',  ( 1.000000000000000000, -0.000000000000000000, -0.000000000000000000 ) ) ;
#24482 = VERTEX_POINT ( 'NONE', #13016 ) ;
#24483 = FACE_OUTER_BOUND ( 'NONE', #11729, .T. ) ;
#24484 = DIRECTION ( 'NONE',  ( 0.000000000000000000, -0.2486898871648622888, 0.9685831611286290777 ) ) ;
#24485 = AXIS2_PLACEMENT_3D ( 'NONE', #8347, #5841, #30685 ) ;
#24486 = ORIENTED_EDGE ( 'NONE', *, *, #26796, .F. ) ;
#24487 = CARTESIAN_POINT ( 'NONE',  ( -37.52044295795950291, -114.9929510916434339, 13.11812344617477244 ) ) ;
#24488 = EDGE_LOOP ( 'NONE', ( #11968, #35011, #28426, #16329 ) ) ;
#24489 = CARTESIAN_POINT ( 'NONE',  ( -36.11231047232249125, -112.0245472910329880, 8.722274454178448266 ) ) ;
#24490 = EDGE_CURVE ( 'NONE', #9715, #6623, #20975, .T. ) ;
#24491 = DIRECTION ( 'NONE',  ( 1.000000000000000000, -5.339440136655842133E-16, -1.047965281155519420E-16 ) ) ;
#24492 = AXIS2_PLACEMENT_3D ( 'NONE', #25643, #25830, #437 ) ;
#24493 = ORIENTED_EDGE ( 'NONE', *, *, #16267, .F. ) ;
#24494 = ORIENTED_EDGE ( 'NONE', *, *, #24490, .T. ) ;
#24495 = DIRECTION ( 'NONE',  ( 0.000000000000000000, -0.5000000000000032196, 0.8660254037844368202 ) ) ;
#24496 = CARTESIAN_POINT ( 'NONE',  ( 8.000000000000000000, 8.931325931664870765, -16.53603053422199665 ) ) ;
#24497 = ORIENTED_EDGE ( 'NONE', *, *, #11974, .T. ) ;
#24498 = CARTESIAN_POINT ( 'NONE',  ( -38.30190309005061522, -111.0245472910330022, 3.527725545821551734 ) ) ;
#24499 = EDGE_CURVE ( 'NONE', #18878, #29834, #1678, .T. ) ;
#24500 = AXIS2_PLACEMENT_3D ( 'NONE', #8959, #11497, #3583 ) ;
#24501 = FACE_OUTER_BOUND ( 'NONE', #15041, .T. ) ;
#24502 = DIRECTION ( 'NONE',  ( 1.000000000000000000, -0.000000000000000000, 0.000000000000000000 ) ) ;
#24503 = ORIENTED_EDGE ( 'NONE', *, *, #14560, .T. ) ;
#24505 = VERTEX_POINT ( 'NONE', #21273 ) ;
#24504 = EDGE_CURVE ( 'NONE', #23442, #11697, #32444, .T. ) ;
#24506 = CARTESIAN_POINT ( 'NONE',  ( 70.00001200000001234, -22.48561656011616705, 82.98552407851633461 ) ) ;
#24507 = FACE_OUTER_BOUND ( 'NONE', #7753, .T. ) ;
#24508 = VERTEX_POINT ( 'NONE', #15508 ) ;
#24509 = ORIENTED_EDGE ( 'NONE', *, *, #12300, .F. ) ;
#24510 = CARTESIAN_POINT ( 'NONE',  ( -34.50000000000000000, -111.7850029017436810, -2.224114562373086912 ) ) ;
#24511 = PRODUCT_DEFINITION_SHAPE ( 'NONE', 'NONE',  #35644 ) ;
#24512 = AXIS2_PLACEMENT_3D ( 'NONE', #29236, #32281, #4580 ) ;
#24513 = ADVANCED_FACE ( 'NONE', ( #24003 ), #7424, .F. ) ;
#24514 = DIRECTION ( 'NONE',  ( -1.000000000000000000, -0.000000000000000000, -0.000000000000000000 ) ) ;
#24515 = VERTEX_POINT ( 'NONE', #18581 ) ;
#24516 = EDGE_CURVE ( 'NONE', #17129, #1113, #21539, .T. ) ;
#24517 = CARTESIAN_POINT ( 'NONE',  ( -35.50000000000000711, -114.8211182053456838, 9.932864235516914775 ) ) ;
#24518 = PRESENTATION_LAYER_ASSIGNMENT (  '', '', ( #15878 ) ) ;
#24519 = CIRCLE ( 'NONE', #4962, 0.04100000000000673939 ) ;
#24520 = AXIS2_PLACEMENT_3D ( 'NONE', #22429, #3383, #11117 ) ;
#24521 = CARTESIAN_POINT ( 'NONE',  ( -34.50300906734826611, -113.9929510916434339, 12.71660600561482468 ) ) ;
#24522 = CARTESIAN_POINT ( 'NONE',  ( 7.999999999999992895, 0.000000000000000000, 0.000000000000000000 ) ) ;
#24523 = DIRECTION ( 'NONE',  ( 0.000000000000000000, 0.000000000000000000, -1.000000000000000000 ) ) ;
#24524 = CARTESIAN_POINT ( 'NONE',  ( -37.99359134332094357, -113.9929510916434339, 12.69998175888958514 ) ) ;
#24525 = CIRCLE ( 'NONE', #25080, 8.000000000000008882 ) ;
#24526 = CARTESIAN_POINT ( 'NONE',  ( -35.50000000000000711, -114.1489256397697289, 9.518467544735724317 ) ) ;
#24527 = FACE_BOUND ( 'NONE', #10689, .T. ) ;
#24528 = DIRECTION ( 'NONE',  ( 0.000000000000000000, 0.000000000000000000, 1.000000000000000000 ) ) ;
#24529 = ORIENTED_EDGE ( 'NONE', *, *, #13286, .T. ) ;
#24530 = DIRECTION ( 'NONE',  ( -1.000000000000000000, -0.000000000000000000, -0.000000000000000000 ) ) ;
#24531 = FACE_BOUND ( 'NONE', #6282, .T. ) ;
#24532 = DIRECTION ( 'NONE',  ( -1.000000000000000000, -0.000000000000000000, 0.000000000000000000 ) ) ;
#24533 = AXIS2_PLACEMENT_3D ( 'NONE', #24831, #27882, #515 ) ;
#24534 = ORIENTED_EDGE ( 'NONE', *, *, #22447, .F. ) ;
#24535 = CARTESIAN_POINT ( 'NONE',  ( 7.999999999999992895, -46.21320724403641833, -10.97699764142004497 ) ) ;
#24536 = ORIENTED_EDGE ( 'NONE', *, *, #11054, .T. ) ;
#24537 = CIRCLE ( 'NONE', #13052, 0.04099999999999958539 ) ;
#24538 = CARTESIAN_POINT ( 'NONE',  ( -35.50000000000000000, -113.0601156079281253, 0.8807106166081309917 ) ) ;
#24539 = DIRECTION ( 'NONE',  ( -1.000000000000000000, 0.000000000000000000, 0.000000000000000000 ) ) ;
#24540 = CARTESIAN_POINT ( 'NONE',  ( -35.50000000000000711, -114.9929510916434339, 12.50851088611648088 ) ) ;
#24541 = DIRECTION ( 'NONE',  ( -1.000000000000000000, 0.000000000000000000, 0.000000000000000000 ) ) ;
#24542 = AXIS2_PLACEMENT_3D ( 'NONE', #30941, #6273, #25733 ) ;
#24543 = ADVANCED_FACE ( 'NONE', ( #16039 ), #32623, .T. ) ;
#24544 = ORIENTED_EDGE ( 'NONE', *, *, #30713, .T. ) ;
#24545 = ADVANCED_FACE ( 'NONE', ( #1862 ), #5793, .F. ) ;
#24546 = DIRECTION ( 'NONE',  ( 0.000000000000000000, -0.8660254037844392627, 0.4999999999999989453 ) ) ;
#24547 = CARTESIAN_POINT ( 'NONE',  ( -35.50000000000000000, -112.4957190293567066, -2.560864217808777266 ) ) ;
#24548 = EDGE_LOOP ( 'NONE', ( #12625, #35137 ) ) ;
#24549 = ORIENTED_EDGE ( 'NONE', *, *, #31642, .F. ) ;
#24550 = VECTOR ( 'NONE', #19701, 1000.000000000000000 ) ;
#24551 = CARTESIAN_POINT ( 'NONE',  ( -37.05926240293133134, -115.0000000000000000, 6.378524454178448266 ) ) ;
#24552 = VECTOR ( 'NONE', #23432, 1000.000000000000000 ) ;
#24553 = AXIS2_PLACEMENT_3D ( 'NONE', #7295, #35044, #18084 ) ;
#24554 = CARTESIAN_POINT ( 'NONE',  ( -44.00000000000000000, 0.000000000000000000, 0.000000000000000000 ) ) ;
#24555 = EDGE_LOOP ( 'NONE', ( #11914, #31367 ) ) ;
#24556 = VERTEX_POINT ( 'NONE', #8124 ) ;
#24557 = CARTESIAN_POINT ( 'NONE',  ( -34.50000000000000000, -115.0304602784513293, -0.6247823525985405357 ) ) ;
#24558 = CARTESIAN_POINT ( 'NONE',  ( -34.49999999999998579, -31.64142946139395107, 72.19543654875866423 ) ) ;
#24559 = DIRECTION ( 'NONE',  ( -1.000000000000000000, 0.000000000000000000, 0.000000000000000000 ) ) ;
#24560 = DIRECTION ( 'NONE',  ( 0.000000000000000000, 0.000000000000000000, 1.000000000000000000 ) ) ;
#24561 = CIRCLE ( 'NONE', #15327, 20.00000000000000355 ) ;
#24562 = AXIS2_PLACEMENT_3D ( 'NONE', #24385, #29967, #22023 ) ;
#24563 = CARTESIAN_POINT ( 'NONE',  ( -35.50000000000000000, -113.9929510916434339, 12.59102132592610346 ) ) ;
#24564 = DIRECTION ( 'NONE',  ( -1.000000000000000000, 0.000000000000000000, 0.000000000000000000 ) ) ;
#24565 = CARTESIAN_POINT ( 'NONE',  ( -42.49999999999999289, -29.27980021920983944, 82.28589838486210795 ) ) ;
#24566 = CARTESIAN_POINT ( 'NONE',  ( -34.50000000000000000, -112.8835768857893527, -1.616767172155725740 ) ) ;
#24567 = CIRCLE ( 'NONE', #25129, 4.000000000000000000 ) ;
#24568 = CARTESIAN_POINT ( 'NONE',  ( -37.34375000000001421, -115.9929510916434481, 14.11852480586265024 ) ) ;
#24569 = CYLINDRICAL_SURFACE ( 'NONE', #26069, 8.000000000000001776 ) ;
#24570 = VECTOR ( 'NONE', #35181, 1000.000000000000000 ) ;
#24571 = VECTOR ( 'NONE', #12704, 1000.000000000000227 ) ;
#24572 = LINE ( 'NONE', #29976, #23817 ) ;
#24574 = ORIENTED_EDGE ( 'NONE', *, *, #10563, .F. ) ;
#24573 = AXIS2_PLACEMENT_3D ( 'NONE', #18819, #4803, #5331 ) ;
#24575 = CARTESIAN_POINT ( 'NONE',  ( -35.50000000000000711, -114.1302255537607095, 9.515717283514957714 ) ) ;
#24576 = CARTESIAN_POINT ( 'NONE',  ( 8.000000000000007105, -11.27190672109268377, 0.3151488735047419665 ) ) ;
#24577 = DIRECTION ( 'NONE',  ( -1.000000000000000000, 0.000000000000000000, 0.000000000000000000 ) ) ;
#24578 = VECTOR ( 'NONE', #2552, 1000.000000000000000 ) ;
#24579 = DIRECTION ( 'NONE',  ( -1.000000000000000000, 0.000000000000000000, 0.000000000000000000 ) ) ;
#24580 = CARTESIAN_POINT ( 'NONE',  ( 8.000000000000000000, 11.19999565274250308, 10.71350075272077973 ) ) ;
#24581 = VERTEX_POINT ( 'NONE', #16395 ) ;
#24582 = CYLINDRICAL_SURFACE ( 'NONE', #6724, 4.000000000000000000 ) ;
#24583 = CARTESIAN_POINT ( 'NONE',  ( -9.999999999999994671, 0.000000000000000000, 0.000000000000000000 ) ) ;
#24584 = PLANE ( 'NONE',  #8464 ) ;
#24585 = CARTESIAN_POINT ( 'NONE',  ( 0.000000000000000000, -42.41764978026620270, 20.20639853260275487 ) ) ;
#24586 = CARTESIAN_POINT ( 'NONE',  ( -4.747884751462066788, -5.143694235356003119, -0.7999999999999951594 ) ) ;
#24587 = DIRECTION ( 'NONE',  ( -1.000000000000000000, 0.000000000000000000, 0.000000000000000000 ) ) ;
#24588 = EDGE_LOOP ( 'NONE', ( #20384, #6645, #20652, #26004, #2936, #16598 ) ) ;
#24589 = VECTOR ( 'NONE', #32714, 1000.000000000000000 ) ;
#24590 = VERTEX_POINT ( 'NONE', #2575 ) ;
#24591 = EDGE_CURVE ( 'NONE', #22745, #12825, #18104, .T. ) ;
#24592 = DIRECTION ( 'NONE',  ( -1.000000000000000000, -0.000000000000000000, -0.000000000000000000 ) ) ;
#24593 = CIRCLE ( 'NONE', #26915, 7.199999999999993072 ) ;
#24594 = DIRECTION ( 'NONE',  ( 0.000000000000000000, 0.000000000000000000, 1.000000000000000000 ) ) ;
#24595 = CARTESIAN_POINT ( 'NONE',  ( 112.0000000000000000, 81.48267994499606459, 34.65054357219658243 ) ) ;
#24596 = VERTEX_POINT ( 'NONE', #30464 ) ;
#24597 = CARTESIAN_POINT ( 'NONE',  ( -36.11231047232249125, -115.9754527089670262, 8.777725545821555286 ) ) ;
#24598 = VERTEX_POINT ( 'NONE', #10847 ) ;
#24599 = AXIS2_PLACEMENT_3D ( 'NONE', #26857, #32775, #7931 ) ;
#24600 = EDGE_LOOP ( 'NONE', ( #20722, #27828, #9261, #29481 ) ) ;
#24601 = ORIENTED_EDGE ( 'NONE', *, *, #15664, .F. ) ;
#24602 = CIRCLE ( 'NONE', #2769, 20.00000000000000711 ) ;
#24603 = CARTESIAN_POINT ( 'NONE',  ( 46.00000000000000000, -25.98076211353320275, 76.99999999999992895 ) ) ;
#24604 = EDGE_CURVE ( 'NONE', #29018, #24581, #1437, .T. ) ;
#24605 = VECTOR ( 'NONE', #27560, 1000.000000000000227 ) ;
#24606 = DIRECTION ( 'NONE',  ( 0.000000000000000000, 0.000000000000000000, 1.000000000000000000 ) ) ;
#24607 = EDGE_LOOP ( 'NONE', ( #5162, #12853, #8802, #26591 ) ) ;
#24608 = DIRECTION ( 'NONE',  ( -1.000000000000000000, 0.000000000000000000, -0.000000000000000000 ) ) ;
#24609 = DIRECTION ( 'NONE',  ( 0.000000000000000000, 0.6573494133204066392, -0.7535859266250380939 ) ) ;
#24610 = CARTESIAN_POINT ( 'NONE',  ( 8.000000000000000000, 18.62763138773855687, 2.494040418455418351 ) ) ;
#24611 = AXIS2_PLACEMENT_3D ( 'NONE', #18223, #34264, #1313 ) ;
#24612 = DIRECTION ( 'NONE',  ( 1.000000000000000000, -5.339440136655842133E-16, -1.047965281155519420E-16 ) ) ;
#24613 = CARTESIAN_POINT ( 'NONE',  ( -21.15833593587365513, -8.980762113533204527, 86.49999999999994316 ) ) ;
#24614 = DIRECTION ( 'NONE',  ( 1.000000000000000000, -0.000000000000000000, -0.000000000000000000 ) ) ;
#24615 = CARTESIAN_POINT ( 'NONE',  ( -38.99699093265172678, -115.9929510916434481, 12.71660600561481402 ) ) ;
#24616 = DIRECTION ( 'NONE',  ( 1.000000000000000000, 0.000000000000000000, 0.000000000000000000 ) ) ;
#24617 = AXIS2_PLACEMENT_3D ( 'NONE', #30603, #3432, #5938 ) ;
#24618 = DIRECTION ( 'NONE',  ( -1.000000000000000000, -1.836970198721029934E-16, -0.000000000000000000 ) ) ;
#24619 = ADVANCED_FACE ( 'NONE', ( #27759 ), #2762, .F. ) ;
#24620 = DIRECTION ( 'NONE',  ( 1.000000000000000000, -4.336808689941996437E-15, -1.084202172485499109E-15 ) ) ;
#24621 = DIRECTION ( 'NONE',  ( -1.000000000000000000, 0.000000000000000000, 0.000000000000000000 ) ) ;
#24622 = DIRECTION ( 'NONE',  ( -1.000000000000000000, 0.000000000000000000, 0.000000000000000000 ) ) ;
#24623 = VERTEX_POINT ( 'NONE', #24704 ) ;
#24624 = CARTESIAN_POINT ( 'NONE',  ( -37.97545270896702618, -114.4734759653044023, 3.152725545821551734 ) ) ;
#24625 = CIRCLE ( 'NONE', #9088, 20.00000000000000355 ) ;
#24626 = LINE ( 'NONE', #2672, #847 ) ;
#24627 = CARTESIAN_POINT ( 'NONE',  ( 0.000000000000000000, -43.83938735307282997, 18.28286404005782728 ) ) ;
#24628 = LINE ( 'NONE', #32903, #20506 ) ;
#24629 = ORIENTED_EDGE ( 'NONE', *, *, #25863, .F. ) ;
#24630 = ORIENTED_EDGE ( 'NONE', *, *, #17320, .T. ) ;
#24631 = EDGE_CURVE ( 'NONE', #4840, #6112, #5441, .T. ) ;
#24632 = DIRECTION ( 'NONE',  ( 0.000000000000000000, -1.000000000000000000, 0.000000000000000000 ) ) ;
#24633 = CARTESIAN_POINT ( 'NONE',  ( -46.00000000000000000, 0.000000000000000000, 0.000000000000000000 ) ) ;
#24634 = ORIENTED_EDGE ( 'NONE', *, *, #27329, .F. ) ;
#24635 = EDGE_CURVE ( 'NONE', #35307, #29380, #22698, .T. ) ;
#24636 = ORIENTED_EDGE ( 'NONE', *, *, #12876, .F. ) ;
#24637 = FACE_BOUND ( 'NONE', #34889, .T. ) ;
#24638 = DIRECTION ( 'NONE',  ( 0.000000000000000000, 0.000000000000000000, -1.000000000000000000 ) ) ;
#24639 = ADVANCED_FACE ( 'NONE', ( #16211 ), #11018, .T. ) ;
#24640 = VECTOR ( 'NONE', #2755, 1000.000000000000000 ) ;
#24641 = DIRECTION ( 'NONE',  ( -1.000000000000000000, 7.806255641895633157E-17, -2.465190328815661892E-32 ) ) ;
#24642 = DIRECTION ( 'NONE',  ( -1.000000000000000000, 0.000000000000000000, 0.000000000000000000 ) ) ;
#24643 = ORIENTED_EDGE ( 'NONE', *, *, #4651, .F. ) ;
#24644 = ORIENTED_EDGE ( 'NONE', *, *, #9012, .T. ) ;
#24645 = CIRCLE ( 'NONE', #9107, 7.199999999999992184 ) ;
#24646 = DIRECTION ( 'NONE',  ( -1.047965281155519667E-16, -6.938893903907193865E-17, -1.000000000000000000 ) ) ;
#24647 = DIRECTION ( 'NONE',  ( -1.000000000000000000, -1.836970198721029934E-16, -0.000000000000000000 ) ) ;
#24648 = EDGE_LOOP ( 'NONE', ( #19622, #9024, #7960, #12353 ) ) ;
#24649 = CARTESIAN_POINT ( 'NONE',  ( 0.000000000000000000, 10.00000000000000888, -15.00000000000000178 ) ) ;
#24650 = CARTESIAN_POINT ( 'NONE',  ( -34.50000000000000000, -112.9813730236132585, -1.624774171495860786 ) ) ;
#24651 = CARTESIAN_POINT ( 'NONE',  ( -38.99879592093640923, -114.9929510916434339, 12.67985367974111455 ) ) ;
#24652 = CARTESIAN_POINT ( 'NONE',  ( -38.00000000000000711, -114.9929510916434339, 11.21034663311206181 ) ) ;
#24653 = LINE ( 'NONE', #14009, #22607 ) ;
#24654 = CARTESIAN_POINT ( 'NONE',  ( -34.54793860109200665, -114.9929510916434339, 13.00730889637958221 ) ) ;
#24655 = CARTESIAN_POINT ( 'NONE',  ( 8.000000000000007105, 0.000000000000000000, 0.000000000000000000 ) ) ;
#24656 = EDGE_CURVE ( 'NONE', #26147, #4012, #11542, .T. ) ;
#24657 = FACE_OUTER_BOUND ( 'NONE', #7919, .T. ) ;
#24658 = CARTESIAN_POINT ( 'NONE',  ( -1.799999999999996048, 0.000000000000000000, 0.000000000000000000 ) ) ;
#24659 = DIRECTION ( 'NONE',  ( -1.000000000000000000, -0.000000000000000000, 0.000000000000000000 ) ) ;
#24660 = DIRECTION ( 'NONE',  ( 1.000000000000000000, -0.000000000000000000, 0.000000000000000000 ) ) ;
#24661 = DIRECTION ( 'NONE',  ( -1.000000000000000000, 0.000000000000000000, 0.000000000000000000 ) ) ;
#24662 = ORIENTED_EDGE ( 'NONE', *, *, #11126, .F. ) ;
#24663 = DIRECTION ( 'NONE',  ( 0.000000000000000000, 0.1736481776669211718, 0.9848077530122096857 ) ) ;
#24664 = ORIENTED_EDGE ( 'NONE', *, *, #274, .F. ) ;
#24665 = CARTESIAN_POINT ( 'NONE',  ( -39.07941549657748936, -111.8367748094582055, 8.441024454178448266 ) ) ;
#24666 = CYLINDRICAL_SURFACE ( 'NONE', #20362, 47.49900000000001654 ) ;
#24667 = ORIENTED_EDGE ( 'NONE', *, *, #6366, .F. ) ;
#24668 = AXIS2_PLACEMENT_3D ( 'NONE', #21474, #10693, #10341 ) ;
#24669 = EDGE_LOOP ( 'NONE', ( #27204, #17136 ) ) ;
#24670 = EDGE_CURVE ( 'NONE', #19516, #31085, #14068, .T. ) ;
#24671 = CYLINDRICAL_SURFACE ( 'NONE', #8502, 7.199999999999994849 ) ;
#24672 = FACE_OUTER_BOUND ( 'NONE', #25617, .T. ) ;
#24673 = EDGE_CURVE ( 'NONE', #31584, #1546, #13526, .T. ) ;
#24674 = EDGE_CURVE ( 'NONE', #31085, #8987, #16750, .T. ) ;
#24675 = ORIENTED_EDGE ( 'NONE', *, *, #8645, .T. ) ;
#24676 = CARTESIAN_POINT ( 'NONE',  ( -34.02454729103297382, -112.6980969099494132, 3.902725545821552178 ) ) ;
#24677 = CYLINDRICAL_SURFACE ( 'NONE', #29944, 4.000000000000000000 ) ;
#24678 = PLANE ( 'NONE',  #33811 ) ;
#24679 = ORIENTED_EDGE ( 'NONE', *, *, #16239, .F. ) ;
#24680 = ORIENTED_EDGE ( 'NONE', *, *, #32625, .T. ) ;
#24681 = DIRECTION ( 'NONE',  ( -1.000000000000000000, -0.000000000000000000, -0.000000000000000000 ) ) ;
#24682 = EDGE_CURVE ( 'NONE', #17551, #27414, #33626, .T. ) ;
#24683 = SURFACE_STYLE_USAGE ( .BOTH. , #25218 ) ;
#24684 = ADVANCED_FACE ( 'NONE', ( #13542 ), #5961, .T. ) ;
#24685 = CARTESIAN_POINT ( 'NONE',  ( 8.000000000000000000, 18.48663108841359559, -3.384281271887881637 ) ) ;
#24686 = ORIENTED_EDGE ( 'NONE', *, *, #13047, .T. ) ;
#24687 = ORIENTED_EDGE ( 'NONE', *, *, #22491, .F. ) ;
#24688 = CARTESIAN_POINT ( 'NONE',  ( -34.50000000000000000, -117.0108842342086888, -0.7556348869410856040 ) ) ;
#24689 = CIRCLE ( 'NONE', #3441, 5.016000000000010672 ) ;
#24690 = DIRECTION ( 'NONE',  ( 1.000000000000000000, -4.336808689941997226E-15, -1.174092375852883357E-15 ) ) ;
#24691 = ORIENTED_EDGE ( 'NONE', *, *, #18679, .F. ) ;
#24692 = CARTESIAN_POINT ( 'NONE',  ( -35.50000000000000711, -114.9929510916434339, 10.61627146648203812 ) ) ;
#24693 = AXIS2_PLACEMENT_3D ( 'NONE', #4203, #20355, #3841 ) ;
#24694 = CARTESIAN_POINT ( 'NONE',  ( -37.42187499999996447, -113.9929510916434339, 14.11852480586265024 ) ) ;
#24695 = DIRECTION ( 'NONE',  ( 1.000000000000000000, -4.528031003192420052E-15, -1.174092375852883160E-15 ) ) ;
#24696 = CARTESIAN_POINT ( 'NONE',  ( 8.000000000000000000, -16.92083251265328769, 4.460989585140905156 ) ) ;
#24697 = AXIS2_PLACEMENT_3D ( 'NONE', #32276, #5445, #2403 ) ;
#24698 = CARTESIAN_POINT ( 'NONE',  ( -34.50000000000000000, -113.9929510916435049, 10.50625754673586876 ) ) ;
#24700 = DIRECTION ( 'NONE',  ( -1.783119874454246424E-31, -1.187911941725854497E-31, 1.000000000000000000 ) ) ;
#24699 = AXIS2_PLACEMENT_3D ( 'NONE', #6831, #15093, #28446 ) ;
#24701 = EDGE_CURVE ( 'NONE', #1785, #34547, #25234, .T. ) ;
#24702 = CARTESIAN_POINT ( 'NONE',  ( -35.50000000000000711, -114.5636144531578680, 9.676196722963288366 ) ) ;
#24703 = DIRECTION ( 'NONE',  ( -1.000000000000000000, -8.673617379884210501E-17, 1.502314598737149170E-16 ) ) ;
#24704 = CARTESIAN_POINT ( 'NONE',  ( -29.99999999999999645, -10.99999999999999645, 0.000000000000000000 ) ) ;
#24705 = ORIENTED_EDGE ( 'NONE', *, *, #18970, .T. ) ;
#24706 = EDGE_CURVE ( 'NONE', #7199, #7407, #3101, .T. ) ;
#24707 = ORIENTED_EDGE ( 'NONE', *, *, #6555, .T. ) ;
#24708 = EDGE_CURVE ( 'NONE', #30567, #21603, #11370, .T. ) ;
#24709 = DIRECTION ( 'NONE',  ( 1.000000000000000000, -0.000000000000000000, 0.000000000000000000 ) ) ;
#24710 = CARTESIAN_POINT ( 'NONE',  ( -0.1374368770859779598, -4.808326913195978491, -0.7999999999999951594 ) ) ;
#24711 = ORIENTED_EDGE ( 'NONE', *, *, #26844, .T. ) ;
#24712 = DIRECTION ( 'NONE',  ( 0.000000000000000000, 0.000000000000000000, -1.000000000000000000 ) ) ;
#24713 = EDGE_LOOP ( 'NONE', ( #17465, #27041, #5859, #15175 ) ) ;
#24714 = CARTESIAN_POINT ( 'NONE',  ( -35.50000000000000000, -113.0140978167138712, 0.7502176474015694874 ) ) ;
#24715 = CARTESIAN_POINT ( 'NONE',  ( 8.000000000000000000, -11.11653975335798528, 12.74840161668727134 ) ) ;
#24716 = CARTESIAN_POINT ( 'NONE',  ( -36.94073759706866156, -113.0000000000000000, 4.128524454178449155 ) ) ;
#24717 = EDGE_CURVE ( 'NONE', #1934, #6914, #3275, .T. ) ;
#24718 = EDGE_CURVE ( 'NONE', #9669, #15756, #17461, .T. ) ;
#24719 = CARTESIAN_POINT ( 'NONE',  ( 7.999999999999992895, -47.32430374665948136, 21.55018039121511819 ) ) ;
#24720 = ORIENTED_EDGE ( 'NONE', *, *, #7739, .F. ) ;
#24721 = AXIS2_PLACEMENT_3D ( 'NONE', #24649, #22622, #27708 ) ;
#24722 = DIRECTION ( 'NONE',  ( 0.000000000000000000, 0.8660254037844410391, -0.4999999999999958367 ) ) ;
#24723 = CARTESIAN_POINT ( 'NONE',  ( -35.50000000000000000, -115.6584342456100671, -2.522673865603758614 ) ) ;
#24724 = ORIENTED_EDGE ( 'NONE', *, *, #29694, .T. ) ;
#24725 = VERTEX_POINT ( 'NONE', #1099 ) ;
#24726 = CARTESIAN_POINT ( 'NONE',  ( -37.05926240293131713, -115.9999999999999858, 7.878524454178450043 ) ) ;
#24727 = STYLED_ITEM ( 'NONE', ( #35609 ), #10310 ) ;
#24728 = PRODUCT_DEFINITION_FORMATION_WITH_SPECIFIED_SOURCE ( 'ANY', '', #20719, .NOT_KNOWN. ) ;
#24729 = CIRCLE ( 'NONE', #12653, 7.000000000000035527 ) ;
#24730 = EDGE_CURVE ( 'NONE', #18755, #17047, #11228, .T. ) ;
#24731 = CARTESIAN_POINT ( 'NONE',  ( 8.000000000000000000, 3.872983346207429900, 1.000000000000003109 ) ) ;
#24732 = VERTEX_POINT ( 'NONE', #33670 ) ;
#24733 = VERTEX_POINT ( 'NONE', #6844 ) ;
#24734 = CARTESIAN_POINT ( 'NONE',  ( -34.50000000000000000, -113.0140978167138712, 0.6252176474015680441 ) ) ;
#24735 = CYLINDRICAL_SURFACE ( 'NONE', #33837, 8.000000000000000000 ) ;
#24736 = CARTESIAN_POINT ( 'NONE',  ( -34.49999999999998579, -17.72201855431906736, 96.30456345124113682 ) ) ;
#24737 = DIRECTION ( 'NONE',  ( 1.000000000000000000, -0.000000000000000000, 0.000000000000000000 ) ) ;
#24738 = CARTESIAN_POINT ( 'NONE',  ( -35.50100302244945993, -113.9929510916434339, 12.65121853911337446 ) ) ;
#24739 = CARTESIAN_POINT ( 'NONE',  ( 7.999999999999992895, -47.22458491092824318, 5.098390039074071289 ) ) ;
#24740 = AXIS2_PLACEMENT_3D ( 'NONE', #4420, #4604, #9441 ) ;
#24741 = DIRECTION ( 'NONE',  ( 0.000000000000000000, 0.000000000000000000, -1.000000000000000000 ) ) ;
#24742 = CARTESIAN_POINT ( 'NONE',  ( -34.50000000000000000, -111.0140978167138570, -0.5622823525984297355 ) ) ;
#24743 = EDGE_CURVE ( 'NONE', #14025, #15523, #4925, .T. ) ;
#24744 = CARTESIAN_POINT ( 'NONE',  ( -38.99999693208653895, -115.9929510916434481, 12.62875129555797749 ) ) ;
#24745 = DIRECTION ( 'NONE',  ( 0.000000000000000000, 0.000000000000000000, 1.000000000000000000 ) ) ;
#24746 = ADVANCED_FACE ( 'NONE', ( #3805 ), #25770, .T. ) ;
#24747 = CARTESIAN_POINT ( 'NONE',  ( -1.398397006337051440, -6.091550361990532458, -0.7999999999999951594 ) ) ;
#24748 = DIRECTION ( 'NONE',  ( -1.000000000000000000, 0.000000000000000000, 0.000000000000000000 ) ) ;
#24749 = ORIENTED_EDGE ( 'NONE', *, *, #4921, .T. ) ;
#24750 = CIRCLE ( 'NONE', #20711, 0.5000000000000004441 ) ;
#24751 = CARTESIAN_POINT ( 'NONE',  ( -38.00000000000000711, -115.9929510916434481, 11.73841344789285657 ) ) ;
#24752 = DIRECTION ( 'NONE',  ( -1.000000000000000000, -1.734723475976807094E-16, 0.000000000000000000 ) ) ;
#24753 = SURFACE_STYLE_FILL_AREA ( #27463 ) ;
#24754 = DIRECTION ( 'NONE',  ( -1.000000000000000000, 0.000000000000000000, 0.000000000000000000 ) ) ;
#24755 = CONTEXT_DEPENDENT_SHAPE_REPRESENTATION ( #20724, #11292 ) ;
#24756 = DIRECTION ( 'NONE',  ( -1.000000000000000000, 0.000000000000000000, 0.000000000000000000 ) ) ;
#24757 = VERTEX_POINT ( 'NONE', #6486 ) ;
#24758 = FACE_OUTER_BOUND ( 'NONE', #6901, .T. ) ;
#24759 = CARTESIAN_POINT ( 'NONE',  ( -46.00000000000000000, -25.98076211353320275, 95.99999999999991473 ) ) ;
#24760 = DIRECTION ( 'NONE',  ( -1.000000000000000000, 0.000000000000000000, 0.000000000000000000 ) ) ;
#24761 = LINE ( 'NONE', #30343, #6924 ) ;
#24762 = EDGE_CURVE ( 'NONE', #29218, #32215, #2642, .T. ) ;
#24763 = EDGE_CURVE ( 'NONE', #26196, #10004, #20424, .T. ) ;
#24764 = CARTESIAN_POINT ( 'NONE',  ( 0.000000000000000000, 19.77827456857338007, -2.969824084036534639 ) ) ;
#24765 = DIRECTION ( 'NONE',  ( -1.000000000000000000, 0.000000000000000000, 0.000000000000000000 ) ) ;
#24766 = ORIENTED_EDGE ( 'NONE', *, *, #264, .T. ) ;
#24767 = CARTESIAN_POINT ( 'NONE',  ( 0.000000000000000000, 0.000000000000000000, 0.000000000000000000 ) ) ;
#24768 = CARTESIAN_POINT ( 'NONE',  ( -42.49999999999999289, -24.48076211353301801, 67.99999999999991473 ) ) ;
#24769 = DIRECTION ( 'NONE',  ( 0.000000000000000000, -0.7705132427757949154, 0.6374239897486827511 ) ) ;
#24770 = EDGE_LOOP ( 'NONE', ( #13642, #18140, #20093, #6809 ) ) ;
#24771 = CARTESIAN_POINT ( 'NONE',  ( -37.05926240293131713, -112.0000000000000142, 8.121475545821549957 ) ) ;
#24772 = ORIENTED_EDGE ( 'NONE', *, *, #15804, .T. ) ;
#24773 = FILL_AREA_STYLE ('',( #19175 ) ) ;
#24774 = VERTEX_POINT ( 'NONE', #20327 ) ;
#24775 = AXIS2_PLACEMENT_3D ( 'NONE', #29490, #4829, #13117 ) ;
#24776 = EDGE_LOOP ( 'NONE', ( #6818, #18550, #16278, #18952 ) ) ;
#24777 = DIRECTION ( 'NONE',  ( 0.000000000000000000, 0.000000000000000000, 1.000000000000000000 ) ) ;
#24778 = VECTOR ( 'NONE', #32454, 1000.000000000000000 ) ;
#24779 = STYLED_ITEM ( 'NONE', ( #23699 ), #9091 ) ;
#24780 = AXIS2_PLACEMENT_3D ( 'NONE', #21257, #10471, #15842 ) ;
#24781 = DIRECTION ( 'NONE',  ( -1.000000000000000000, 0.000000000000000000, 0.000000000000000000 ) ) ;
#24782 = ORIENTED_EDGE ( 'NONE', *, *, #28700, .T. ) ;
#24783 = DIRECTION ( 'NONE',  ( -1.000000000000000000, 0.000000000000000000, -0.000000000000000000 ) ) ;
#24784 = FACE_OUTER_BOUND ( 'NONE', #18464, .T. ) ;
#24785 = FACE_OUTER_BOUND ( 'NONE', #9552, .T. ) ;
#24786 = LINE ( 'NONE', #2657, #11931 ) ;
#24787 = CARTESIAN_POINT ( 'NONE',  ( 0.000000000000000000, 13.60411018104336023, -12.96676809804134400 ) ) ;
#24788 = EDGE_CURVE ( 'NONE', #3037, #27614, #33652, .T. ) ;
#24789 = AXIS2_PLACEMENT_3D ( 'NONE', #27499, #29843, #10568 ) ;
#24790 = DIRECTION ( 'NONE',  ( 0.000000000000000000, 4.163336342344333082E-15, 1.000000000000000000 ) ) ;
#24791 = CARTESIAN_POINT ( 'NONE',  ( -35.97545865737298953, -115.9929510916434481, 14.11837420659365527 ) ) ;
#24792 = CARTESIAN_POINT ( 'NONE',  ( 0.000000000000000000, -2.710505431213761085E-17, -45.89999999999999858 ) ) ;
#24793 = DIRECTION ( 'NONE',  ( 0.000000000000000000, 0.3420201433256629953, 0.9396926207859105373 ) ) ;
#24794 = FACE_OUTER_BOUND ( 'NONE', #2455, .T. ) ;
#24795 = DIRECTION ( 'NONE',  ( -1.000000000000000000, 0.000000000000000000, 0.000000000000000000 ) ) ;
#24796 = DIRECTION ( 'NONE',  ( 0.000000000000000000, -0.5000000000000092149, 0.8660254037844333785 ) ) ;
#24797 = SURFACE_STYLE_USAGE ( .BOTH. , #29852 ) ;
#24798 = VERTEX_POINT ( 'NONE', #34410 ) ;
#24799 = AXIS2_PLACEMENT_3D ( 'NONE', #9913, #28658, #20876 ) ;
#24800 = CARTESIAN_POINT ( 'NONE',  ( -37.97545270896702618, -114.4734759653044023, 4.652725545821551734 ) ) ;
#24801 = AXIS2_PLACEMENT_3D ( 'NONE', #31316, #889, #28626 ) ;
#24802 = DIRECTION ( 'NONE',  ( 0.000000000000000000, 0.000000000000000000, 1.000000000000000000 ) ) ;
#24803 = DIRECTION ( 'NONE',  ( 1.000000000000000000, 0.000000000000000000, 0.000000000000000000 ) ) ;
#24804 = DIRECTION ( 'NONE',  ( 0.000000000000000000, 0.000000000000000000, -1.000000000000000000 ) ) ;
#24805 = EDGE_LOOP ( 'NONE', ( #4308, #20715, #20429, #28790 ) ) ;
#24806 = ORIENTED_EDGE ( 'NONE', *, *, #1333, .T. ) ;
#24807 = UNCERTAINTY_MEASURE_WITH_UNIT (LENGTH_MEASURE( 1.000000000000000082E-05 ), #15841, 'distance_accuracy_value', 'NONE');
#24808 = FACE_OUTER_BOUND ( 'NONE', #22663, .T. ) ;
#24809 = CARTESIAN_POINT ( 'NONE',  ( 8.000000000000000000, 18.48663108841356717, 3.384281271888136988 ) ) ;
#24810 = ORIENTED_EDGE ( 'NONE', *, *, #12636, .F. ) ;
#24811 = ORIENTED_EDGE ( 'NONE', *, *, #19865, .T. ) ;
#24812 = DIRECTION ( 'NONE',  ( -1.000000000000000000, 0.000000000000000000, 0.000000000000000000 ) ) ;
#24813 = CARTESIAN_POINT ( 'NONE',  ( -9.999999999999994671, 0.000000000000000000, 0.000000000000000000 ) ) ;
#24814 = CARTESIAN_POINT ( 'NONE',  ( 37.99999999999999289, 1.506315562951244531E-14, 0.000000000000000000 ) ) ;
#24815 = DIRECTION ( 'NONE',  ( 0.000000000000000000, 0.000000000000000000, -1.000000000000000000 ) ) ;
#24816 = ORIENTED_EDGE ( 'NONE', *, *, #34394, .T. ) ;
#24817 = ORIENTED_EDGE ( 'NONE', *, *, #10323, .F. ) ;
#24818 = CARTESIAN_POINT ( 'NONE',  ( 0.000000000000000000, 0.000000000000000000, 38.00000000000000000 ) ) ;
#24819 = LINE ( 'NONE', #8245, #6308 ) ;
#24820 = AXIS2_PLACEMENT_3D ( 'NONE', #28588, #16869, #3221 ) ;
#24821 = MECHANICAL_DESIGN_GEOMETRIC_PRESENTATION_REPRESENTATION (  '', ( #28264 ), #35194 ) ;
#24822 = ORIENTED_EDGE ( 'NONE', *, *, #6179, .T. ) ;
#24823 = VECTOR ( 'NONE', #8240, 1000.000000000000000 ) ;
#24824 = DIRECTION ( 'NONE',  ( -1.000000000000000000, -0.000000000000000000, -0.000000000000000000 ) ) ;
#24825 = CARTESIAN_POINT ( 'NONE',  ( -34.50000000000000000, -113.2224311500466030, -1.624782352598427959 ) ) ;
#24826 = EDGE_CURVE ( 'NONE', #2129, #8092, #16964, .T. ) ;
#24827 = CARTESIAN_POINT ( 'NONE',  ( -37.56132887387857267, -114.9929510916434339, 14.11732072679899197 ) ) ;
#24828 = CARTESIAN_POINT ( 'NONE',  ( -35.50000000000000000, -113.9929510916433344, 10.50625754673586876 ) ) ;
#24829 = DIRECTION ( 'NONE',  ( 0.000000000000000000, -0.4817536741017036661, -0.8763066800438699122 ) ) ;
#24830 = CARTESIAN_POINT ( 'NONE',  ( -34.50000000000000000, -114.9929510916434339, 12.17846912687782712 ) ) ;
#24831 = CARTESIAN_POINT ( 'NONE',  ( 65.00000000000001421, 81.48267994499606459, 30.15054357219658954 ) ) ;
#24832 = CARTESIAN_POINT ( 'NONE',  ( 8.000000000000000000, -13.60411018104308667, -12.96676809804163000 ) ) ;
#24833 = CARTESIAN_POINT ( 'NONE',  ( 4.000000000000003553, 0.6505223195690454929, -51.99593080916758936 ) ) ;
#24834 = AXIS2_PLACEMENT_3D ( 'NONE', #13329, #4872, #2190 ) ;
#24835 = DIRECTION ( 'NONE',  ( 0.000000000000000000, -0.6427876096865297040, -0.7660444431189861181 ) ) ;
#24836 = DIRECTION ( 'NONE',  ( 0.000000000000000000, 0.000000000000000000, -1.000000000000000000 ) ) ;
#24837 = ORIENTED_EDGE ( 'NONE', *, *, #23644, .F. ) ;
#24838 = CARTESIAN_POINT ( 'NONE',  ( 0.000000000000000000, -9.471478019455243924, 14.71414642875952161 ) ) ;
#24839 = ORIENTED_EDGE ( 'NONE', *, *, #28647, .F. ) ;
#24840 = EDGE_CURVE ( 'NONE', #9394, #16271, #1465, .T. ) ;
#24841 = CARTESIAN_POINT ( 'NONE',  ( -38.18337828418795965, -110.9754527089670546, 4.034774454178449155 ) ) ;
#24842 = DIRECTION ( 'NONE',  ( 1.734723475976807094E-16, -1.000000000000000000, 0.000000000000000000 ) ) ;
#24843 = ORIENTED_EDGE ( 'NONE', *, *, #24631, .T. ) ;
#24844 = ORIENTED_EDGE ( 'NONE', *, *, #17360, .T. ) ;
#24845 = CARTESIAN_POINT ( 'NONE',  ( 4.000000000000003553, 2.912696353505820124, 21.80633394113451473 ) ) ;
#24846 = CARTESIAN_POINT ( 'NONE',  ( -4.000000000000000000, -2.710505431213761085E-17, -30.90000000000000568 ) ) ;
#24847 = ORIENTED_EDGE ( 'NONE', *, *, #24788, .T. ) ;
#24848 = AXIS2_PLACEMENT_3D ( 'NONE', #10209, #4465, #15944 ) ;
#24849 = CARTESIAN_POINT ( 'NONE',  ( -40.02454729103296671, -112.8166217158120332, 4.840225545821551734 ) ) ;
#24850 = CARTESIAN_POINT ( 'NONE',  ( 8.000000000000000000, 0.000000000000000000, 0.000000000000000000 ) ) ;
#24851 = DIRECTION ( 'NONE',  ( 0.000000000000000000, 0.000000000000000000, -1.000000000000000000 ) ) ;
#24852 = ORIENTED_EDGE ( 'NONE', *, *, #18914, .T. ) ;
#24853 = VERTEX_POINT ( 'NONE', #17279 ) ;
#24854 = CARTESIAN_POINT ( 'NONE',  ( 7.999999999999992895, 27.43636312076375461, -38.14186064215119387 ) ) ;
#24855 = ADVANCED_FACE ( 'NONE', ( #23043 ), #17102, .T. ) ;
#24856 = FILL_AREA_STYLE_COLOUR ( '', #32320 ) ;
#24857 = LINE ( 'NONE', #8281, #34570 ) ;
#24858 = ORIENTED_EDGE ( 'NONE', *, *, #10982, .F. ) ;
#24859 = ORIENTED_EDGE ( 'NONE', *, *, #35459, .F. ) ;
#24860 = CIRCLE ( 'NONE', #29467, 14.00000000000000000 ) ;
#24861 = CARTESIAN_POINT ( 'NONE',  ( -34.50000000000000000, -117.0140978167138854, 0.3752176474015737617 ) ) ;
#24862 = FACE_OUTER_BOUND ( 'NONE', #23147, .T. ) ;
#24863 = EDGE_LOOP ( 'NONE', ( #10503, #15893, #33673, #21240, #17710, #12083 ) ) ;
#24864 = CARTESIAN_POINT ( 'NONE',  ( -35.49999931242378892, -114.9929510916434339, 12.61439929482945566 ) ) ;
#24865 = EDGE_CURVE ( 'NONE', #4346, #11860, #35402, .T. ) ;
#24866 = CARTESIAN_POINT ( 'NONE',  ( -35.95093014754292682, -113.9929510916434339, 14.11777216781842625 ) ) ;
#24867 = CIRCLE ( 'NONE', #29478, 3.800000000000018918 ) ;
#24868 = EDGE_CURVE ( 'NONE', #13276, #33932, #15240, .T. ) ;
#24869 = CARTESIAN_POINT ( 'NONE',  ( 8.000000000000000000, 16.59870953437680896, 10.45300502024390354 ) ) ;
#24870 = LINE ( 'NONE', #14399, #23127 ) ;
#24871 = EDGE_CURVE ( 'NONE', #28086, #7873, #18129, .T. ) ;
#24872 = CIRCLE ( 'NONE', #33493, 4.800000000000005151 ) ;
#24873 = CARTESIAN_POINT ( 'NONE',  ( -34.50000000000000000, -113.9929510916433912, 10.50625754673588474 ) ) ;
#24874 = CARTESIAN_POINT ( 'NONE',  ( -38.99984940073101569, -114.9929510916434339, 12.64306614848957189 ) ) ;
#24875 = CARTESIAN_POINT ( 'NONE',  ( -35.50000000000000711, -114.0928965812550757, 9.511088712577292270 ) ) ;
#24876 = DIRECTION ( 'NONE',  ( 1.541976423090495140E-16, -1.000000000000000000, 0.000000000000000000 ) ) ;
#24877 = DIRECTION ( 'NONE',  ( -1.000000000000000000, 0.000000000000000000, 0.000000000000000000 ) ) ;
#24878 = ORIENTED_EDGE ( 'NONE', *, *, #25380, .F. ) ;
#24879 = VERTEX_POINT ( 'NONE', #3991 ) ;
#24880 = EDGE_CURVE ( 'NONE', #15127, #11959, #9727, .T. ) ;
#24881 = DIRECTION ( 'NONE',  ( -1.000000000000000000, 0.000000000000000000, 0.000000000000000000 ) ) ;
#24882 = CARTESIAN_POINT ( 'NONE',  ( -42.49999999999999289, -25.98076211353320986, 84.99999999999994316 ) ) ;
#24883 = EDGE_CURVE ( 'NONE', #21916, #30516, #28111, .T. ) ;
#24884 = VERTEX_POINT ( 'NONE', #28284 ) ;
#24885 = AXIS2_PLACEMENT_3D ( 'NONE', #12121, #20370, #6891 ) ;
#24886 = DIRECTION ( 'NONE',  ( 1.000000000000000000, -5.339440136655842133E-16, -1.047965281155519420E-16 ) ) ;
#24887 = ORIENTED_EDGE ( 'NONE', *, *, #1789, .F. ) ;
#24888 = CARTESIAN_POINT ( 'NONE',  ( -35.50000000000000711, -115.9630435732166518, -0.9469505670456015434 ) ) ;
#24889 = DIRECTION ( 'NONE',  ( 0.000000000000000000, -0.6427876096865294819, -0.7660444431189861181 ) ) ;
#24890 = CARTESIAN_POINT ( 'NONE',  ( -36.52652403469556930, -113.0245472910329880, 8.722274454178450043 ) ) ;
#24891 = CARTESIAN_POINT ( 'NONE',  ( 4.000000000000003553, -43.55304910509385508, -28.41006711800031326 ) ) ;
#24892 = VERTEX_POINT ( 'NONE', #3453 ) ;
#24893 = DIRECTION ( 'NONE',  ( 0.000000000000000000, -0.9980267284282723361, 0.06279051952930261860 ) ) ;
#24894 = VECTOR ( 'NONE', #31202, 1000.000000000000000 ) ;
#24895 = CARTESIAN_POINT ( 'NONE',  ( -35.50000000000000711, -112.9415908020655195, 1.873661708251232572 ) ) ;
#24896 = CIRCLE ( 'NONE', #20852, 4.000000000000000000 ) ;
#24897 = ORIENTED_EDGE ( 'NONE', *, *, #5148, .F. ) ;
#24898 = ORIENTED_EDGE ( 'NONE', *, *, #28248, .F. ) ;
#24899 = CARTESIAN_POINT ( 'NONE',  ( -38.97545270896704039, -113.1123104723225197, 6.847274454178450931 ) ) ;
#24900 = ADVANCED_FACE ( 'NONE', ( #14404 ), #14577, .T. ) ;
#24901 = DIRECTION ( 'NONE',  ( -1.000000000000000000, 0.000000000000000000, 0.000000000000000000 ) ) ;
#24902 = ORIENTED_EDGE ( 'NONE', *, *, #18519, .T. ) ;
#24903 = VERTEX_POINT ( 'NONE', #27016 ) ;
#24904 = CARTESIAN_POINT ( 'NONE',  ( -34.50000000000000000, -115.0140978167138712, -0.3122823525984416704 ) ) ;
#24905 = DIRECTION ( 'NONE',  ( 1.000000000000000000, 0.000000000000000000, 0.000000000000000000 ) ) ;
#24906 = PRODUCT_RELATED_PRODUCT_CATEGORY ( 'part', '', ( #1781 ) ) ;
#24907 = PRODUCT_DEFINITION_CONTEXT ( 'detailed design', #7123, 'design' ) ;
#24908 = CYLINDRICAL_SURFACE ( 'NONE', #31005, 4.800000000000000711 ) ;
#24909 = TOROIDAL_SURFACE ( 'NONE', #8798, 4.200000000000000178, 0.1999999999999998723 ) ;
#24910 = VECTOR ( 'NONE', #20947, 1000.000000000000000 ) ;
#24911 = ADVANCED_FACE ( 'NONE', ( #4874 ), #7389, .T. ) ;
#24912 = CARTESIAN_POINT ( 'NONE',  ( -35.50000000000000000, -113.9929510916434339, 10.68227981832981044 ) ) ;
#24913 = DIRECTION ( 'NONE',  ( 0.000000000000000000, 0.000000000000000000, -1.000000000000000000 ) ) ;
#24914 = EDGE_CURVE ( 'NONE', #32151, #30389, #15467, .T. ) ;
#24915 = CARTESIAN_POINT ( 'NONE',  ( 5.400000000000071410, 0.9999999999999662492, 55.00000000000000711 ) ) ;
#24916 = EDGE_CURVE ( 'NONE', #22786, #3877, #26485, .T. ) ;
#24917 = CARTESIAN_POINT ( 'NONE',  ( -34.50000000000000000, -112.5389594332240222, 2.818899826424027477 ) ) ;
#24918 = CARTESIAN_POINT ( 'NONE',  ( -35.50000000000000000, -114.2253558743059330, 8.519800927820798009 ) ) ;
#24919 = LINE ( 'NONE', #5832, #13002 ) ;
#24921 = AXIS2_PLACEMENT_3D ( 'NONE', #22686, #8491, #30468 ) ;
#24920 = DIRECTION ( 'NONE',  ( 1.000000000000000000, 0.000000000000000000, 0.000000000000000000 ) ) ;
#24922 = ORIENTED_EDGE ( 'NONE', *, *, #9369, .F. ) ;
#24923 = CIRCLE ( 'NONE', #7099, 20.00000000000000711 ) ;
#24924 = CARTESIAN_POINT ( 'NONE',  ( -37.58145695302688694, -115.9929510916434481, 13.11211614918362756 ) ) ;
#24925 = CARTESIAN_POINT ( 'NONE',  ( 3.999999999999996447, -3.968388925834655190, -21.63912866391144618 ) ) ;
#24926 = DIRECTION ( 'NONE',  ( 0.000000000000000000, 0.000000000000000000, -1.000000000000000000 ) ) ;
#24927 = DIRECTION ( 'NONE',  ( -1.000000000000000000, -0.000000000000000000, 0.000000000000000000 ) ) ;
#24928 = ADVANCED_FACE ( 'NONE', ( #20862, #32407 ), #10080, .T. ) ;
#24929 = EDGE_LOOP ( 'NONE', ( #5900, #25262 ) ) ;
#24930 = CARTESIAN_POINT ( 'NONE',  ( -0.2142857142857362840, -10.49781318335649161, -1.200000000000006617 ) ) ;
#24931 = CARTESIAN_POINT ( 'NONE',  ( 0.2142857142857085284, -10.49781318335649161, 0.000000000000000000 ) ) ;
#24932 = DIRECTION ( 'NONE',  ( 0.000000000000000000, 0.000000000000000000, -1.000000000000000000 ) ) ;
#24933 = DIRECTION ( 'NONE',  ( 0.000000000000000000, 0.000000000000000000, -1.000000000000000000 ) ) ;
#24934 = ITEM_DEFINED_TRANSFORMATION ( 'NONE', 'NONE', #9243,  #21307 ) ;
#24935 = PLANE ( 'NONE',  #27924 ) ;
#24936 = DIRECTION ( 'NONE',  ( -1.000000000000000000, -1.836970198721029934E-16, -0.000000000000000000 ) ) ;
#24937 = VECTOR ( 'NONE', #853, 1000.000000000000000 ) ;
#24938 = ORIENTED_EDGE ( 'NONE', *, *, #2261, .F. ) ;
#24939 = CIRCLE ( 'NONE', #7112, 52.00000000000000711 ) ;
#24940 = DIRECTION ( 'NONE',  ( 1.000000000000000000, -4.607758420995283758E-15, -1.196244974681468005E-15 ) ) ;
#24941 = DIRECTION ( 'NONE',  ( -1.000000000000000000, -1.836970198721029934E-16, -0.000000000000000000 ) ) ;
#24942 = LINE ( 'NONE', #21874, #29508 ) ;
#24943 = ORIENTED_EDGE ( 'NONE', *, *, #32146, .T. ) ;
#24944 = CARTESIAN_POINT ( 'NONE',  ( -35.62769128460905677, -112.5438815906447729, 9.808975545821551734 ) ) ;
#24945 = VERTEX_POINT ( 'NONE', #16001 ) ;
#24946 = ADVANCED_FACE ( 'NONE', ( #34582 ), #12615, .T. ) ;
#24947 =( NAMED_UNIT ( * ) SI_UNIT ( $, .STERADIAN. ) SOLID_ANGLE_UNIT ( ) );
#24948 = VERTEX_POINT ( 'NONE', #12791 ) ;
#24949 = EDGE_LOOP ( 'NONE', ( #21027, #16464, #15751, #31048 ) ) ;
#24950 = DIRECTION ( 'NONE',  ( -1.000000000000000000, 0.000000000000000000, 0.000000000000000000 ) ) ;
#24951 = EDGE_CURVE ( 'NONE', #22316, #30516, #17556, .T. ) ;
#24952 = AXIS2_PLACEMENT_3D ( 'NONE', #7026, #17466, #4347 ) ;
#24953 = CIRCLE ( 'NONE', #20908, 7.199999999999992184 ) ;
#24954 = EDGE_CURVE ( 'NONE', #32016, #12368, #8366, .T. ) ;
#24955 = LINE ( 'NONE', #30361, #11049 ) ;
#24956 = LINE ( 'NONE', #14131, #570 ) ;
#24957 = PLANE ( 'NONE',  #566 ) ;
#24958 = EDGE_CURVE ( 'NONE', #16010, #26553, #7212, .T. ) ;
#24959 = CARTESIAN_POINT ( 'NONE',  ( 0.000000000000000000, 0.000000000000000000, 3.000000000000002665 ) ) ;
#24960 = EDGE_CURVE ( 'NONE', #1374, #21589, #31940, .T. ) ;
#24961 = DIRECTION ( 'NONE',  ( -1.000000000000000000, 0.000000000000000000, 0.000000000000000000 ) ) ;
#24962 = CARTESIAN_POINT ( 'NONE',  ( 7.999999999999992895, 45.78515115856061612, -12.64416602183615623 ) ) ;
#24963 = DIRECTION ( 'NONE',  ( -1.000000000000000000, -0.000000000000000000, 0.000000000000000000 ) ) ;
#24964 = CARTESIAN_POINT ( 'NONE',  ( -37.51022648969539119, -115.9929510916434481, 14.11852173794918563 ) ) ;
#24965 = CARTESIAN_POINT ( 'NONE',  ( 4.121423858225409909, -12.61643262889541894, -1.200000000000006617 ) ) ;
#24966 = FACE_OUTER_BOUND ( 'NONE', #7210, .T. ) ;
#24967 = CYLINDRICAL_SURFACE ( 'NONE', #26239, 19.99999999999998579 ) ;
#24968 = FACE_OUTER_BOUND ( 'NONE', #35167, .T. ) ;
#24969 = AXIS2_PLACEMENT_3D ( 'NONE', #19038, #18677, #13471 ) ;
#24970 = AXIS2_PLACEMENT_3D ( 'NONE', #34411, #17995, #6487 ) ;
#24971 = CARTESIAN_POINT ( 'NONE',  ( -2.000000000000000888, -4.579597227308185762E-14, 6.765000000000020997 ) ) ;
#24972 = PRESENTATION_STYLE_ASSIGNMENT (( #24797 ) ) ;
#24973 = ORIENTED_EDGE ( 'NONE', *, *, #9512, .T. ) ;
#24974 = CARTESIAN_POINT ( 'NONE',  ( -37.76916472181486739, -116.0245472910329880, 8.965225545821551734 ) ) ;
#24975 = CARTESIAN_POINT ( 'NONE',  ( -44.00000000000000000, 0.000000000000000000, 0.000000000000000000 ) ) ;
#24976 = DIRECTION ( 'NONE',  ( 0.000000000000000000, 0.000000000000000000, -1.000000000000000000 ) ) ;
#24977 = CARTESIAN_POINT ( 'NONE',  ( 65.00000000000001421, 49.63000703270403591, 62.56502393413636298 ) ) ;
#24978 = ORIENTED_EDGE ( 'NONE', *, *, #15864, .T. ) ;
#24979 = VERTEX_POINT ( 'NONE', #29187 ) ;
#24980 = DIRECTION ( 'NONE',  ( 0.000000000000000000, 0.3090169943749412895, 0.9510565162951555296 ) ) ;
#24981 = DIRECTION ( 'NONE',  ( -1.000000000000000000, 0.000000000000000000, 0.000000000000000000 ) ) ;
#24982 = VERTEX_POINT ( 'NONE', #29710 ) ;
#24983 = ORIENTED_EDGE ( 'NONE', *, *, #9779, .F. ) ;
#24984 = EDGE_CURVE ( 'NONE', #14069, #27933, #4340, .T. ) ;
#24985 = EDGE_CURVE ( 'NONE', #34324, #10214, #29541, .T. ) ;
#24986 = FACE_OUTER_BOUND ( 'NONE', #30906, .T. ) ;
#24987 = FACE_OUTER_BOUND ( 'NONE', #27063, .T. ) ;
#24988 = DIRECTION ( 'NONE',  ( -6.058232658448418820E-17, -0.9730768813850325660, -0.2304807647374927382 ) ) ;
#24989 = FACE_OUTER_BOUND ( 'NONE', #2670, .T. ) ;
#24990 = ORIENTED_EDGE ( 'NONE', *, *, #448, .T. ) ;
#24991 = ORIENTED_EDGE ( 'NONE', *, *, #23353, .F. ) ;
#24992 = VECTOR ( 'NONE', #13261, 1000.000000000000114 ) ;
#24993 = AXIS2_PLACEMENT_3D ( 'NONE', #1235, #14894, #33823 ) ;
#24994 = DIRECTION ( 'NONE',  ( 1.047965281155515106E-16, -6.938893903907203726E-17, -1.000000000000000000 ) ) ;
#24995 = DIRECTION ( 'NONE',  ( -1.000000000000000000, 0.000000000000000000, -0.000000000000000000 ) ) ;
#24996 = VERTEX_POINT ( 'NONE', #12969 ) ;
#24997 = CYLINDRICAL_SURFACE ( 'NONE', #26445, 3.799999999999999822 ) ;
#24998 = VECTOR ( 'NONE', #690, 1000.000000000000000 ) ;
#24999 = CARTESIAN_POINT ( 'NONE',  ( -34.50000000000000000, -112.5103839485166333, -1.498529437127682495 ) ) ;
#25000 = CARTESIAN_POINT ( 'NONE',  ( -39.00000000000000711, -114.9929510916434339, 12.59102132592608925 ) ) ;
#25001 = CARTESIAN_POINT ( 'NONE',  ( -35.50000000000000000, -113.9929510916434339, 10.50625754673588474 ) ) ;
#25002 = DIRECTION ( 'NONE',  ( 0.000000000000000000, -0.2538061376417689030, -0.9672551082808337197 ) ) ;
#25003 = CARTESIAN_POINT ( 'NONE',  ( -35.61121590948313553, -114.9929510916434339, 14.07058620477040733 ) ) ;
#25004 = DIRECTION ( 'NONE',  ( -1.000000000000000000, 0.000000000000000000, 0.000000000000000000 ) ) ;
#25005 = CARTESIAN_POINT ( 'NONE',  ( -34.49999999999998579, 7.019851009788996343, 105.5074730863398003 ) ) ;
#25006 = AXIS2_PLACEMENT_3D ( 'NONE', #23086, #23264, #29035 ) ;
#25007 = B_SPLINE_CURVE_WITH_KNOTS ( 'NONE', 3,
 ( #12553, #33988, #6962, #23343, #23169, #15225, #31458, #26234, #34343, #31627, #1573, #17758, #3932, #9839, #20802, #25891, #28582, #9670 ),
 .UNSPECIFIED., .F., .F.,
 ( 4, 2, 2, 2, 2, 2, 2, 2, 4 ),
 ( 0.5000000000000000000, 0.5625000000000000000, 0.6250000000000000000, 0.6875000000000000000, 0.7500000000000000000, 0.8125000000000000000, 0.8750000000000000000, 0.9375000000000000000, 1.000000000000000000 ),
 .UNSPECIFIED. ) ;
#25008 = FACE_OUTER_BOUND ( 'NONE', #16907, .T. ) ;
#25009 = DIRECTION ( 'NONE',  ( 0.000000000000000000, 0.000000000000000000, -1.000000000000000000 ) ) ;
#25010 = DIRECTION ( 'NONE',  ( 0.000000000000000000, 0.000000000000000000, 1.000000000000000000 ) ) ;
#25011 = ORIENTED_EDGE ( 'NONE', *, *, #22097, .T. ) ;
#25012 = CARTESIAN_POINT ( 'NONE',  ( 8.000000000000000000, 14.80634052301623171, -8.177498406287266874 ) ) ;
#25013 = ORIENTED_EDGE ( 'NONE', *, *, #745, .T. ) ;
#25014 = CARTESIAN_POINT ( 'NONE',  ( -39.99999999999999289, -113.9407375970686758, 3.753524454178448710 ) ) ;
#25015 = DIRECTION ( 'NONE',  ( -1.000000000000000000, 0.000000000000000000, 0.000000000000000000 ) ) ;
#25016 = CARTESIAN_POINT ( 'NONE',  ( -35.50000000000000711, -113.6807644833805995, -1.624782352598427959 ) ) ;
#25017 = ORIENTED_EDGE ( 'NONE', *, *, #10653, .F. ) ;
#25018 = VERTEX_POINT ( 'NONE', #34758 ) ;
#25019 = AXIS2_PLACEMENT_3D ( 'NONE', #16540, #13679, #14015 ) ;
#25020 = CARTESIAN_POINT ( 'NONE',  ( -46.00000000000000000, 1.347111479062088405E-15, -11.00000000000000000 ) ) ;
#25021 = AXIS2_PLACEMENT_3D ( 'NONE', #31603, #31074, #28909 ) ;
#25022 = DIRECTION ( 'NONE',  ( -1.000000000000000000, 0.000000000000000000, 0.000000000000000000 ) ) ;
#25023 = ORIENTED_EDGE ( 'NONE', *, *, #6869, .F. ) ;
#25024 = CIRCLE ( 'NONE', #14087, 20.00000000000000711 ) ;
#25025 = VECTOR ( 'NONE', #23160, 1000.000000000000000 ) ;
#25026 = DIRECTION ( 'NONE',  ( 0.000000000000000000, 0.000000000000000000, 1.000000000000000000 ) ) ;
#25027 = ADVANCED_FACE ( 'NONE', ( #31684 ), #32053, .T. ) ;
#25028 = CARTESIAN_POINT ( 'NONE',  ( -55.00000000000000000, -2.775557561562891351E-14, 110.0000000000000000 ) ) ;
#25029 = EDGE_LOOP ( 'NONE', ( #28375, #24978, #31625, #21653 ) ) ;
#25030 = VERTEX_POINT ( 'NONE', #23957 ) ;
#25031 = DIRECTION ( 'NONE',  ( 0.000000000000000000, -0.3681245526846654292, -0.9297764858882563432 ) ) ;
#25032 =( NAMED_UNIT ( * ) PLANE_ANGLE_UNIT ( ) SI_UNIT ( $, .RADIAN. ) );
#25033 = DIRECTION ( 'NONE',  ( -1.000000000000000000, -1.734723475976807094E-16, -0.000000000000000000 ) ) ;
#25035 = ORIENTED_EDGE ( 'NONE', *, *, #3495, .F. ) ;
#25034 = AXIS2_PLACEMENT_3D ( 'NONE', #9189, #31335, #9367 ) ;
#25036 = VERTEX_POINT ( 'NONE', #34952 ) ;
#25037 = CARTESIAN_POINT ( 'NONE',  ( -34.50000000000000000, -117.0140978167138854, -0.3747823525984421145 ) ) ;
#25038 = ADVANCED_FACE ( 'NONE', ( #10273 ), #32231, .T. ) ;
#25039 = ORIENTED_EDGE ( 'NONE', *, *, #14732, .T. ) ;
#25040 = CARTESIAN_POINT ( 'NONE',  ( -35.50000000000000711, -114.9929510916434339, 12.56351784598954424 ) ) ;
#25041 = CARTESIAN_POINT ( 'NONE',  ( -36.50000000000010658, -113.9929510916434339, 14.11852480586265024 ) ) ;
#25042 = AXIS2_PLACEMENT_3D ( 'NONE', #35214, #24400, #29089 ) ;
#25043 = DIRECTION ( 'NONE',  ( 0.000000000000000000, 0.000000000000000000, -1.000000000000000000 ) ) ;
#25044 = DIRECTION ( 'NONE',  ( 0.000000000000000000, 0.5877852522924738032, -0.8090169943749468962 ) ) ;
#25045 = CARTESIAN_POINT ( 'NONE',  ( -34.50000000000000000, -113.9929510916434339, 10.55026311463432087 ) ) ;
#25046 = CARTESIAN_POINT ( 'NONE',  ( -39.00000000000000711, -114.9929510916434339, 12.44250253426874941 ) ) ;
#25047 = CIRCLE ( 'NONE', #7794, 8.000000000000007105 ) ;
#25048 = CARTESIAN_POINT ( 'NONE',  ( -35.50000000000000711, -114.9929501463477663, 10.50247632894551231 ) ) ;
#25049 = DIRECTION ( 'NONE',  ( -1.000000000000000000, 0.000000000000000000, 0.000000000000000000 ) ) ;
#25050 = CARTESIAN_POINT ( 'NONE',  ( -34.49999999999998579, -36.56745899286266166, 87.83669687932923864 ) ) ;
#25051 = VERTEX_POINT ( 'NONE', #35128 ) ;
#25052 = ORIENTED_EDGE ( 'NONE', *, *, #34427, .F. ) ;
#25053 = DIRECTION ( 'NONE',  ( -1.000000000000000000, 0.000000000000000000, 0.000000000000000000 ) ) ;
#25054 = CARTESIAN_POINT ( 'NONE',  ( 7.999999999999992895, -27.79676263918213763, 37.88001506494759241 ) ) ;
#25055 = AXIS2_PLACEMENT_3D ( 'NONE', #20150, #909, #22677 ) ;
#25056 = EDGE_LOOP ( 'NONE', ( #33562, #3593, #25205, #26409 ) ) ;
#25057 = DIRECTION ( 'NONE',  ( 1.000000000000000000, 0.000000000000000000, 0.000000000000000000 ) ) ;
#25058 = ORIENTED_EDGE ( 'NONE', *, *, #18312, .T. ) ;
#25059 = CARTESIAN_POINT ( 'NONE',  ( -35.50000000000000000, -113.2224311500466030, -0.6247823525984269599 ) ) ;
#25060 = CARTESIAN_POINT ( 'NONE',  ( -4.000000000000000000, -2.710505431213761085E-17, 55.00000000000000000 ) ) ;
#25061 = CARTESIAN_POINT ( 'NONE',  ( -35.00000000000000000, -114.0592624029313242, 4.503524454178448266 ) ) ;
#25062 = CARTESIAN_POINT ( 'NONE',  ( -34.49999999999998579, 9.432411113711806294, 117.4309090467819772 ) ) ;
#25063 = EDGE_LOOP ( 'NONE', ( #15073, #19642, #26009, #6125 ) ) ;
#25064 = CARTESIAN_POINT ( 'NONE',  ( 30.00000000000000000, 1.359357947053562196E-14, 0.000000000000000000 ) ) ;
#25065 = EDGE_CURVE ( 'NONE', #14334, #7205, #22727, .T. ) ;
#25066 = CARTESIAN_POINT ( 'NONE',  ( -35.50000000000000711, -112.9185811467682754, 1.870920967077121411 ) ) ;
#25067 = ORIENTED_EDGE ( 'NONE', *, *, #8476, .T. ) ;
#25068 = EDGE_LOOP ( 'NONE', ( #6671, #13566, #25591, #8860 ) ) ;
#25069 = EDGE_CURVE ( 'NONE', #22531, #25964, #25630, .T. ) ;
#25070 = CARTESIAN_POINT ( 'NONE',  ( -37.88768952767750164, -115.9754527089670262, 7.972274454178450043 ) ) ;
#25071 = AXIS2_PLACEMENT_3D ( 'NONE', #14287, #977, #33919 ) ;
#25072 = CARTESIAN_POINT ( 'NONE',  ( 8.000000000000000000, 21.63912866391145329, -3.968388925834584136 ) ) ;
#25073 = ORIENTED_EDGE ( 'NONE', *, *, #16382, .T. ) ;
#25074 = ORIENTED_EDGE ( 'NONE', *, *, #22451, .F. ) ;
#25075 = CARTESIAN_POINT ( 'NONE',  ( -34.50000000000000000, -112.0209493036498287, 0.9959249592223760050 ) ) ;
#25076 = AXIS2_PLACEMENT_3D ( 'NONE', #823, #650, #127 ) ;
#25077 = DIRECTION ( 'NONE',  ( -1.000000000000000000, 0.000000000000000000, 0.000000000000000000 ) ) ;
#25078 = EDGE_CURVE ( 'NONE', #211, #10299, #27908, .T. ) ;
#25079 = ORIENTED_EDGE ( 'NONE', *, *, #26918, .T. ) ;
#25080 = AXIS2_PLACEMENT_3D ( 'NONE', #31393, #9964, #28339 ) ;
#25081 = CARTESIAN_POINT ( 'NONE',  ( -34.50000000000001421, -27.48076211353330578, 101.9999999999999432 ) ) ;
#25082 = EDGE_CURVE ( 'NONE', #24515, #9009, #10096, .T. ) ;
#25083 = AXIS2_PLACEMENT_3D ( 'NONE', #18493, #34363, #15241 ) ;
#25084 = CARTESIAN_POINT ( 'NONE',  ( -35.50000000000000000, -113.9929510916434339, 10.50625754673588474 ) ) ;
#25085 = DIRECTION ( 'NONE',  ( 1.783119874454246424E-31, 1.187911941725854497E-31, -1.000000000000000000 ) ) ;
#25086 = DIRECTION ( 'NONE',  ( -1.000000000000000000, 0.000000000000000000, -0.000000000000000000 ) ) ;
#25087 = CARTESIAN_POINT ( 'NONE',  ( -34.50000000000000000, -115.8878449012421754, -1.128496220799388494 ) ) ;
#25088 = CARTESIAN_POINT ( 'NONE',  ( -39.00000000000000000, -115.9929510916434481, 12.44250253426875119 ) ) ;
#25089 = DIRECTION ( 'NONE',  ( -1.000000000000000000, 0.000000000000000000, 0.000000000000000000 ) ) ;
#25090 = CARTESIAN_POINT ( 'NONE',  ( 0.2000000000000057288, -6.997142273814354496, 0.000000000000000000 ) ) ;
#25091 = VECTOR ( 'NONE', #23599, 1000.000000000000000 ) ;
#25092 = VERTEX_POINT ( 'NONE', #5916 ) ;
#25093 = DIRECTION ( 'NONE',  ( 0.000000000000000000, 0.000000000000000000, 1.000000000000000000 ) ) ;
#25094 = CARTESIAN_POINT ( 'NONE',  ( 8.000000000000007105, -3.753907720749058541, 8.725776631572749409 ) ) ;
#25095 = LINE ( 'NONE', #19840, #1319 ) ;
#25096 = CIRCLE ( 'NONE', #11849, 15.49899999999999167 ) ;
#25097 = EDGE_CURVE ( 'NONE', #16380, #18803, #21566, .T. ) ;
#25098 = ORIENTED_EDGE ( 'NONE', *, *, #18480, .F. ) ;
#25099 = CIRCLE ( 'NONE', #18772, 7.199999999999993072 ) ;
#25100 = LINE ( 'NONE', #22382, #1312 ) ;
#25101 = DIRECTION ( 'NONE',  ( 0.000000000000000000, 0.000000000000000000, 1.000000000000000000 ) ) ;
#25102 = CARTESIAN_POINT ( 'NONE',  ( 0.000000000000000000, -9.604183132802312173, -5.908880290975638161 ) ) ;
#25103 = LINE ( 'NONE', #9070, #33372 ) ;
#25104 = AXIS2_PLACEMENT_3D ( 'NONE', #26387, #2093, #26202 ) ;
#25105 = CONTEXT_DEPENDENT_SHAPE_REPRESENTATION ( #19308, #29392 ) ;
#25106 = AXIS2_PLACEMENT_3D ( 'NONE', #32645, #13555, #4588 ) ;
#25107 = CARTESIAN_POINT ( 'NONE',  ( 4.000000000000003553, 7.162210897276456656, -51.50439529848821252 ) ) ;
#25108 = DIRECTION ( 'NONE',  ( -1.000000000000000000, -0.000000000000000000, -0.000000000000000000 ) ) ;
#25109 = CIRCLE ( 'NONE', #19882, 47.49900000000001654 ) ;
#25110 = ORIENTED_EDGE ( 'NONE', *, *, #24195, .F. ) ;
#25111 = DIRECTION ( 'NONE',  ( 0.000000000000000000, 0.000000000000000000, 1.000000000000000000 ) ) ;
#25112 = EDGE_CURVE ( 'NONE', #6684, #688, #12985, .T. ) ;
#25113 = CYLINDRICAL_SURFACE ( 'NONE', #30337, 4.000000000000000000 ) ;
#25114 = CARTESIAN_POINT ( 'NONE',  ( -44.00000000000000000, 0.000000000000000000, 0.000000000000000000 ) ) ;
#25115 = EDGE_LOOP ( 'NONE', ( #7594, #13318, #1683, #29023 ) ) ;
#25116 = EDGE_CURVE ( 'NONE', #20467, #7261, #22164, .T. ) ;
#25117 = CARTESIAN_POINT ( 'NONE',  ( -37.35495115944176803, -115.0245472910329880, 2.965225545821551734 ) ) ;
#25118 = EDGE_CURVE ( 'NONE', #14626, #18718, #26790, .T. ) ;
#25119 = VERTEX_POINT ( 'NONE', #27548 ) ;
#25120 = AXIS2_PLACEMENT_3D ( 'NONE', #23498, #34493, #31955 ) ;
#25121 = FILL_AREA_STYLE ('',( #28346 ) ) ;
#25122 = VECTOR ( 'NONE', #27361, 1000.000000000000000 ) ;
#25123 = VERTEX_POINT ( 'NONE', #32757 ) ;
#25124 = ORIENTED_EDGE ( 'NONE', *, *, #1601, .T. ) ;
#25125 = DIRECTION ( 'NONE',  ( -0.000000000000000000, 0.000000000000000000, -1.000000000000000000 ) ) ;
#25126 = VECTOR ( 'NONE', #14268, 1000.000000000000000 ) ;
#25127 = EDGE_CURVE ( 'NONE', #30873, #34917, #15834, .T. ) ;
#25128 = CARTESIAN_POINT ( 'NONE',  ( -35.50000000000000711, -113.8474311500459777, -1.624782352598427959 ) ) ;
#25129 = AXIS2_PLACEMENT_3D ( 'NONE', #28556, #12341, #6939 ) ;
#25130 = ADVANCED_FACE ( 'NONE', ( #21577 ), #19065, .T. ) ;
#25131 = FACE_OUTER_BOUND ( 'NONE', #26208, .T. ) ;
#25132 = DIRECTION ( 'NONE',  ( -0.000000000000000000, 0.000000000000000000, -1.000000000000000000 ) ) ;
#25133 = DIRECTION ( 'NONE',  ( -0.000000000000000000, 1.000000000000000000, 0.000000000000000000 ) ) ;
#25134 = AXIS2_PLACEMENT_3D ( 'NONE', #26984, #29670, #23917 ) ;
#25135 = AXIS2_PLACEMENT_3D ( 'NONE', #1028, #11632, #27691 ) ;
#25136 = CARTESIAN_POINT ( 'NONE',  ( 0.000000000000000000, 50.95304419620825342, 10.38206564895680017 ) ) ;
#25137 = CARTESIAN_POINT ( 'NONE',  ( -34.50000000000000000, -114.0743172650041686, 9.508870970061893857 ) ) ;
#25138 = CARTESIAN_POINT ( 'NONE',  ( 0.000000000000000000, 14.80634052301623171, 8.177498406287277533 ) ) ;
#25139 = UNCERTAINTY_MEASURE_WITH_UNIT (LENGTH_MEASURE( 1.000000000000000082E-05 ), #7166, 'distance_accuracy_value', 'NONE');
#25140 = CARTESIAN_POINT ( 'NONE',  ( 0.000000000000000000, -43.55304910509385508, -28.41006711800031326 ) ) ;
#25141 = CARTESIAN_POINT ( 'NONE',  ( -37.48437500000004263, -115.9929510916434481, 14.11852480586265024 ) ) ;
#25142 = CARTESIAN_POINT ( 'NONE',  ( 8.000000000000007105, 0.000000000000000000, 0.000000000000000000 ) ) ;
#25143 = EDGE_CURVE ( 'NONE', #24732, #11716, #350, .T. ) ;
#25144 = DIRECTION ( 'NONE',  ( 0.000000000000000000, 0.000000000000000000, 1.000000000000000000 ) ) ;
#25145 = CIRCLE ( 'NONE', #9618, 47.49900000000001654 ) ;
#25146 = DIRECTION ( 'NONE',  ( -1.000000000000000000, 0.000000000000000000, 0.000000000000000000 ) ) ;
#25147 = CARTESIAN_POINT ( 'NONE',  ( -42.49999999999999289, -10.50833024919765180, 77.79903810567678590 ) ) ;
#25148 = AXIS2_PLACEMENT_3D ( 'NONE', #32708, #27139, #13280 ) ;
#25149 = ADVANCED_FACE ( 'NONE', ( #19234 ), #7909, .T. ) ;
#25150 = DIRECTION ( 'NONE',  ( -1.000000000000000000, 0.000000000000000000, 0.000000000000000000 ) ) ;
#25151 = SURFACE_STYLE_USAGE ( .BOTH. , #10937 ) ;
#25152 = ORIENTED_EDGE ( 'NONE', *, *, #14047, .T. ) ;
#25153 = ADVANCED_FACE ( 'NONE', ( #24483 ), #30238, .T. ) ;
#25154 = CARTESIAN_POINT ( 'NONE',  ( -37.35495115944176803, -115.0245472910329880, 2.965225545821551734 ) ) ;
#25155 = CARTESIAN_POINT ( 'NONE',  ( 8.000000000000007105, 3.753907720749211308, -8.725776631572673026 ) ) ;
#25156 = LINE ( 'NONE', #17022, #411 ) ;
#25157 = VECTOR ( 'NONE', #13943, 1000.000000000000000 ) ;
#25158 = DIRECTION ( 'NONE',  ( -1.000000000000000000, 0.000000000000000000, 0.000000000000000000 ) ) ;
#25159 = ORIENTED_EDGE ( 'NONE', *, *, #34052, .T. ) ;
#25160 = ORIENTED_EDGE ( 'NONE', *, *, #30560, .T. ) ;
#25161 = VECTOR ( 'NONE', #15665, 1000.000000000000000 ) ;
#25162 = CARTESIAN_POINT ( 'NONE',  ( 50.00000000000000000, 0.000000000000000000, 0.000000000000000000 ) ) ;
#25163 = CARTESIAN_POINT ( 'NONE',  ( 0.000000000000000000, -2.710505431213761085E-17, -22.00000000000000000 ) ) ;
#25164 = EDGE_LOOP ( 'NONE', ( #21508, #18416, #10196, #10652 ) ) ;
#25165 = AXIS2_PLACEMENT_3D ( 'NONE', #35050, #16270, #29456 ) ;
#25166 = EDGE_CURVE ( 'NONE', #31607, #26780, #2716, .T. ) ;
#25167 = EDGE_LOOP ( 'NONE', ( #17963, #30612, #21538, #24630, #15708 ) ) ;
#25168 = EDGE_CURVE ( 'NONE', #8935, #2111, #1488, .T. ) ;
#25169 = VECTOR ( 'NONE', #35484, 1000.000000000000000 ) ;
#25170 = CARTESIAN_POINT ( 'NONE',  ( 0.000000000000000000, -2.710505431213761085E-17, -22.00000000000000000 ) ) ;
#25171 = CARTESIAN_POINT ( 'NONE',  ( 75.00000000000002842, -25.99649394950422021, 81.00003093645240426 ) ) ;
#25172 = APPLICATION_PROTOCOL_DEFINITION ( 'draft international standard', 'automotive_design', 1998, #16046 ) ;
#25173 = EDGE_CURVE ( 'NONE', #10239, #25998, #5579, .T. ) ;
#25174 = CYLINDRICAL_SURFACE ( 'NONE', #15035, 3.999999999999996447 ) ;
#25175 = CIRCLE ( 'NONE', #29220, 4.000000000000000000 ) ;
#25176 = ORIENTED_EDGE ( 'NONE', *, *, #1582, .F. ) ;
#25177 = VERTEX_POINT ( 'NONE', #27194 ) ;
#25178 = CIRCLE ( 'NONE', #18250, 20.00000000000000000 ) ;
#25179 = DIRECTION ( 'NONE',  ( 0.000000000000000000, 0.000000000000000000, 1.000000000000000000 ) ) ;
#25180 = DIRECTION ( 'NONE',  ( -1.000000000000000000, -0.000000000000000000, -0.000000000000000000 ) ) ;
#25181 = ORIENTED_EDGE ( 'NONE', *, *, #19383, .F. ) ;
#25182 = DIRECTION ( 'NONE',  ( 0.000000000000000000, -6.866613759074851423E-15, 1.000000000000000000 ) ) ;
#25183 = AXIS2_PLACEMENT_3D ( 'NONE', #462, #5696, #13798 ) ;
#25184 = CARTESIAN_POINT ( 'NONE',  ( -34.50000000000000000, -115.0140978167134165, -0.6247823525984399495 ) ) ;
#25185 = CARTESIAN_POINT ( 'NONE',  ( 7.999999999999992895, 0.000000000000000000, 0.000000000000000000 ) ) ;
#25186 = LINE ( 'NONE', #25535, #14408 ) ;
#25187 = CIRCLE ( 'NONE', #12537, 9.499000000000012989 ) ;
#25188 = CARTESIAN_POINT ( 'NONE',  ( -34.50000000000000000, -115.9929510916434481, 10.51175824272318415 ) ) ;
#25189 = FACE_OUTER_BOUND ( 'NONE', #14861, .T. ) ;
#25190 = DIRECTION ( 'NONE',  ( -1.000000000000000000, 0.000000000000000000, 0.000000000000000000 ) ) ;
#25191 = CARTESIAN_POINT ( 'NONE',  ( -35.98977351030467986, -114.9929510916434339, 14.11852173794918386 ) ) ;
#25192 = CARTESIAN_POINT ( 'NONE',  ( 4.000000000000003553, 21.63912866391140710, 3.968388925834887893 ) ) ;
#25193 = VECTOR ( 'NONE', #17074, 1000.000000000000000 ) ;
#25194 = ADVANCED_FACE ( 'NONE', ( #16542, #2885 ), #33115, .F. ) ;
#25195 = FACE_OUTER_BOUND ( 'NONE', #35088, .T. ) ;
#25196 = DIRECTION ( 'NONE',  ( 1.000000000000000000, -0.000000000000000000, 0.000000000000000000 ) ) ;
#25197 = LINE ( 'NONE', #22636, #19788 ) ;
#25198 = EDGE_CURVE ( 'NONE', #22664, #30, #34866, .T. ) ;
#25199 = ORIENTED_EDGE ( 'NONE', *, *, #313, .F. ) ;
#25200 = CARTESIAN_POINT ( 'NONE',  ( 7.999999999999992895, -27.79676263918161894, -37.88001506494798321 ) ) ;
#25201 = ORIENTED_EDGE ( 'NONE', *, *, #17409, .F. ) ;
#25202 = CARTESIAN_POINT ( 'NONE',  ( -36.94073759706866156, -111.0000000000000284, 2.628524454178448710 ) ) ;
#25203 = CARTESIAN_POINT ( 'NONE',  ( 8.000000000000000000, -16.31134495048480559, -6.336799421339987859 ) ) ;
#25204 = CARTESIAN_POINT ( 'NONE',  ( -35.50000000000000711, -112.0140978167138712, -0.4685323525984295134 ) ) ;
#25205 = ORIENTED_EDGE ( 'NONE', *, *, #15046, .F. ) ;
#25206 = ORIENTED_EDGE ( 'NONE', *, *, #12355, .T. ) ;
#25207 = CARTESIAN_POINT ( 'NONE',  ( 5.400000000000085620, -1.000000000000049516, 53.00000000000000711 ) ) ;
#25208 = CARTESIAN_POINT ( 'NONE',  ( 22.99999999999998934, 13.00000000000000888, 1.592040838891559293E-15 ) ) ;
#25209 = CIRCLE ( 'NONE', #3934, 8.000000000000012434 ) ;
#25210 = ORIENTED_EDGE ( 'NONE', *, *, #32106, .F. ) ;
#25211 = AXIS2_PLACEMENT_3D ( 'NONE', #229, #17308, #11213 ) ;
#25212 = CYLINDRICAL_SURFACE ( 'NONE', #11529, 20.00000000000000355 ) ;
#25213 = CARTESIAN_POINT ( 'NONE',  ( 1.498621416870377532, 9.427001662121964880E-16, 4.980000000000000426 ) ) ;
#25214 = EDGE_LOOP ( 'NONE', ( #21871, #14676, #8887, #19733, #382, #29507, #32158, #16330, #35439, #18210, #22575, #18281, #23980, #17561, #17837, #14945 ) ) ;
#25215 = EDGE_LOOP ( 'NONE', ( #9569, #15562, #31491, #32689 ) ) ;
#25216 = DIRECTION ( 'NONE',  ( 0.000000000000000000, 0.000000000000000000, 1.000000000000000000 ) ) ;
#25217 = AXIS2_PLACEMENT_3D ( 'NONE', #18503, #7875, #19037 ) ;
#25218 = SURFACE_SIDE_STYLE ('',( #28093 ) ) ;
#25219 = CYLINDRICAL_SURFACE ( 'NONE', #8105, 7.020000000000045759 ) ;
#25220 = ORIENTED_EDGE ( 'NONE', *, *, #20902, .T. ) ;
#25221 = VERTEX_POINT ( 'NONE', #22296 ) ;
#25222 = CARTESIAN_POINT ( 'NONE',  ( -35.50000000000000000, -113.2372261171341563, 2.916049522752222511 ) ) ;
#25223 = ORIENTED_EDGE ( 'NONE', *, *, #29524, .T. ) ;
#25224 = CARTESIAN_POINT ( 'NONE',  ( -35.50100302244946704, -114.9929510916434339, 12.65121853911337269 ) ) ;
#25225 = CARTESIAN_POINT ( 'NONE',  ( -34.50000000000000000, -113.9929510916434339, 11.91443571948720148 ) ) ;
#25226 = FACE_OUTER_BOUND ( 'NONE', #2363, .T. ) ;
#25227 = PLANE ( 'NONE',  #5921 ) ;
#25228 = CARTESIAN_POINT ( 'NONE',  ( -34.50000000000000000, -113.9929510916434339, 12.53051367006571581 ) ) ;
#25229 = DIRECTION ( 'NONE',  ( 0.000000000000000000, 0.000000000000000000, -1.000000000000000000 ) ) ;
#25230 = AXIS2_PLACEMENT_3D ( 'NONE', #31062, #14844, #6390 ) ;
#25231 = CARTESIAN_POINT ( 'NONE',  ( -35.50000000000000711, -114.9902084924877954, 10.43071793783961176 ) ) ;
#25232 = DIRECTION ( 'NONE',  ( -1.000000000000000000, 0.000000000000000000, 0.000000000000000000 ) ) ;
#25233 = AXIS2_PLACEMENT_3D ( 'NONE', #30133, #30315, #26919 ) ;
#25234 = LINE ( 'NONE', #33157, #19259 ) ;
#25235 = ADVANCED_FACE ( 'NONE', ( #14713 ), #28243, .T. ) ;
#25236 = VERTEX_POINT ( 'NONE', #34004 ) ;
#25237 = ORIENTED_EDGE ( 'NONE', *, *, #2986, .T. ) ;
#25238 = CARTESIAN_POINT ( 'NONE',  ( -23.00000000000000355, 4.000000000000000000, 4.898587196589411843E-16 ) ) ;
#25239 = CARTESIAN_POINT ( 'NONE',  ( 7.999999999999992895, 5.400000000000113154, 0.000000000000000000 ) ) ;
#25240 = EDGE_LOOP ( 'NONE', ( #28880, #31044, #15216, #7410 ) ) ;
#25241 = DIRECTION ( 'NONE',  ( 0.000000000000000000, 0.000000000000000000, 1.000000000000000000 ) ) ;
#25242 = EDGE_LOOP ( 'NONE', ( #24922, #30383, #35152, #8848 ) ) ;
#25243 = CARTESIAN_POINT ( 'NONE',  ( -35.50000000000000000, -115.0140978167138428, -0.6247823525979866455 ) ) ;
#25244 = DIRECTION ( 'NONE',  ( -1.000000000000000000, 0.000000000000000000, 0.000000000000000000 ) ) ;
#25245 = CARTESIAN_POINT ( 'NONE',  ( -37.35495115944176092, -112.9754527089670688, 8.534774454178448266 ) ) ;
#25246 = ORIENTED_EDGE ( 'NONE', *, *, #15867, .T. ) ;
#25247 = CARTESIAN_POINT ( 'NONE',  ( -34.49999999999998579, -25.98076211353322051, 84.99999999999992895 ) ) ;
#25248 = EDGE_LOOP ( 'NONE', ( #1044, #27651 ) ) ;
#25249 = SURFACE_STYLE_USAGE ( .BOTH. , #13741 ) ;
#25250 = CARTESIAN_POINT ( 'NONE',  ( -35.50000000000000000, -114.5974311500472567, -2.624782352598442614 ) ) ;
#25251 = EDGE_LOOP ( 'NONE', ( #29983, #8981, #15892, #7230, #10245, #33293 ) ) ;
#25252 = ORIENTED_EDGE ( 'NONE', *, *, #6321, .F. ) ;
#25253 = DIRECTION ( 'NONE',  ( 1.000000000000000000, -0.000000000000000000, -0.000000000000000000 ) ) ;
#25254 = VECTOR ( 'NONE', #19687, 1000.000000000000000 ) ;
#25255 = SURFACE_STYLE_FILL_AREA ( #8851 ) ;
#25256 = DIRECTION ( 'NONE',  ( -1.000000000000000000, 0.000000000000000000, 0.000000000000000000 ) ) ;
#25257 = B_SPLINE_CURVE_WITH_KNOTS ( 'NONE', 3,
 ( #32251, #13180, #18200, #13523, #29910, #24333, #24506, #23797, #29211, #16193, #34779, #21255, #5078, #24153, #32428, #2380, #7576, #4730 ),
 .UNSPECIFIED., .F., .F.,
 ( 4, 2, 2, 2, 2, 2, 2, 2, 4 ),
 ( 0.000000000000000000, 0.06250000000000000000, 0.1250000000000000000, 0.1875000000000000000, 0.2500000000000000000, 0.3125000000000000000, 0.3750000000000000000, 0.4375000000000000000, 0.5000000000000000000 ),
 .UNSPECIFIED. ) ;
#25258 = ORIENTED_EDGE ( 'NONE', *, *, #26434, .T. ) ;
#25259 = VERTEX_POINT ( 'NONE', #20463 ) ;
#25260 = CARTESIAN_POINT ( 'NONE',  ( -34.50000000000000000, -112.0141059978162019, -0.6575071456984691309 ) ) ;
#25261 = CARTESIAN_POINT ( 'NONE',  ( 4.000000000000000000, 4.627536653468036720E-16, -45.10000000000000142 ) ) ;
#25262 = ORIENTED_EDGE ( 'NONE', *, *, #15601, .F. ) ;
#25263 = PRODUCT_DEFINITION_CONTEXT ( 'detailed design', #3001, 'design' ) ;
#25264 = AXIS2_PLACEMENT_3D ( 'NONE', #31850, #9714, #10065 ) ;
#25265 = DIRECTION ( 'NONE',  ( -1.000000000000000000, -0.000000000000000000, 0.000000000000000000 ) ) ;
#25266 = CARTESIAN_POINT ( 'NONE',  ( -35.50000000000000000, -113.9929510916434339, 10.50625754673586876 ) ) ;
#25267 = DIRECTION ( 'NONE',  ( 0.000000000000000000, -1.000000000000000000, 0.000000000000000000 ) ) ;
#25268 = CARTESIAN_POINT ( 'NONE',  ( 0.000000000000000000, -36.06787431788704623, 37.45808914225476371 ) ) ;
#25269 = CARTESIAN_POINT ( 'NONE',  ( -34.50000000000000000, -112.8230659962028994, 2.866612799894348029 ) ) ;
#25270 = CARTESIAN_POINT ( 'NONE',  ( -35.50000000000000000, -114.5266723804073195, 8.577838247824468354 ) ) ;
#25271 = DIRECTION ( 'NONE',  ( -1.174092375852890260E-15, 4.222049128630259891E-16, 1.000000000000000000 ) ) ;
#25272 = FACE_OUTER_BOUND ( 'NONE', #20989, .T. ) ;
#25273 = EDGE_CURVE ( 'NONE', #3555, #19005, #21026, .T. ) ;
#25274 = EDGE_CURVE ( 'NONE', #16647, #31433, #25372, .T. ) ;
#25275 = CARTESIAN_POINT ( 'NONE',  ( 8.000000000000007105, 0.000000000000000000, 0.000000000000000000 ) ) ;
#25276 = DIRECTION ( 'NONE',  ( 1.000000000000000000, 1.734723475976807094E-16, 0.000000000000000000 ) ) ;
#25277 = DIRECTION ( 'NONE',  ( 0.000000000000000000, 0.000000000000000000, 1.000000000000000000 ) ) ;
#25278 = ORIENTED_EDGE ( 'NONE', *, *, #29434, .F. ) ;
#25279 = AXIS2_PLACEMENT_3D ( 'NONE', #7545, #4862, #15803 ) ;
#25280 = CARTESIAN_POINT ( 'NONE',  ( 0.000000000000000000, 16.71027810728552154, -2.620268201066000113 ) ) ;
#25281 = PLANE ( 'NONE',  #18711 ) ;
#25282 = LINE ( 'NONE', #970, #32632 ) ;
#25283 = DIRECTION ( 'NONE',  ( -1.226634733346697831E-16, 0.7071067811865557884, -0.7071067811865392461 ) ) ;
#25284 = ITEM_DEFINED_TRANSFORMATION ( 'NONE', 'NONE', #30533,  #21307 ) ;
#25285 = ADVANCED_FACE ( 'NONE', ( #684 ), #11664, .T. ) ;
#25286 = VECTOR ( 'NONE', #30632, 1000.000000000000000 ) ;
#25287 = AXIS2_PLACEMENT_3D ( 'NONE', #11868, #9167, #20665 ) ;
#25288 = VECTOR ( 'NONE', #1800, 1000.000000000000000 ) ;
#25289 = LINE ( 'NONE', #25107, #15282 ) ;
#25290 = CARTESIAN_POINT ( 'NONE',  ( 0.000000000000000000, 0.000000000000000000, 0.000000000000000000 ) ) ;
#25291 = ORIENTED_EDGE ( 'NONE', *, *, #9286, .F. ) ;
#25292 = DIRECTION ( 'NONE',  ( -1.000000000000000000, -0.000000000000000000, -0.000000000000000000 ) ) ;
#25293 = CYLINDRICAL_SURFACE ( 'NONE', #20543, 7.000000000000006217 ) ;
#25294 = FACE_OUTER_BOUND ( 'NONE', #25600, .T. ) ;
#25295 = EDGE_LOOP ( 'NONE', ( #22639, #5241, #28245, #9398 ) ) ;
#25296 = CARTESIAN_POINT ( 'NONE',  ( -36.25098837183130485, -114.6652019342044184, 5.683975545821551734 ) ) ;
#25297 = EDGE_LOOP ( 'NONE', ( #21917, #25159 ) ) ;
#25298 = ORIENTED_EDGE ( 'NONE', *, *, #9446, .T. ) ;
#25299 = VERTEX_POINT ( 'NONE', #3951 ) ;
#25300 = CARTESIAN_POINT ( 'NONE',  ( 8.000000000000007105, 0.000000000000000000, 0.000000000000000000 ) ) ;
#25301 = AXIS2_PLACEMENT_3D ( 'NONE', #33763, #27667, #28011 ) ;
#25302 = CARTESIAN_POINT ( 'NONE',  ( -35.50000000000000711, -114.8057644833805568, -1.624782352598427959 ) ) ;
#25303 = EDGE_CURVE ( 'NONE', #26998, #20111, #8947, .T. ) ;
#25304 = DIRECTION ( 'NONE',  ( 0.000000000000000000, 0.9848077530122085754, -0.1736481776669275556 ) ) ;
#25305 = AXIS2_PLACEMENT_3D ( 'NONE', #29886, #3228, #35469 ) ;
#25306 = CARTESIAN_POINT ( 'NONE',  ( -35.50000000000000711, -114.9927795562974069, 10.48735431211914815 ) ) ;
#25307 = FACE_BOUND ( 'NONE', #10198, .T. ) ;
#25308 = AXIS2_PLACEMENT_3D ( 'NONE', #35087, #10409, #35257 ) ;
#25309 = DIRECTION ( 'NONE',  ( -1.000000000000000000, 0.000000000000000000, 0.000000000000000000 ) ) ;
#25310 = DIRECTION ( 'NONE',  ( -1.000000000000000000, 0.000000000000000000, 0.000000000000000000 ) ) ;
#25311 = CIRCLE ( 'NONE', #14340, 52.00000000000000711 ) ;
#25312 = CARTESIAN_POINT ( 'NONE',  ( -34.50000000000000000, -114.9929510916434339, 10.51175824272318415 ) ) ;
#25313 = DIRECTION ( 'NONE',  ( -1.000000000000000000, 0.000000000000000000, 0.000000000000000000 ) ) ;
#25314 = EDGE_CURVE ( 'NONE', #29087, #34324, #25905, .T. ) ;
#25315 = PRODUCT_DEFINITION_SHAPE ( 'NONE', 'NONE',  #23811 ) ;
#25316 = EDGE_CURVE ( 'NONE', #1317, #15438, #7238, .T. ) ;
#25317 = DIRECTION ( 'NONE',  ( 1.000000000000000000, 0.000000000000000000, 0.000000000000000000 ) ) ;
#25318 = ADVANCED_FACE ( 'NONE', ( #33822 ), #9146, .T. ) ;
#25319 = CARTESIAN_POINT ( 'NONE',  ( -35.50000000000000000, -114.2899554544714960, 8.528375582263644006 ) ) ;
#25320 = CARTESIAN_POINT ( 'NONE',  ( -35.50000000000000711, -112.6043641208289188, 1.789429170677330649 ) ) ;
#25321 = DIRECTION ( 'NONE',  ( 1.000000000000000000, -5.339440136655842133E-16, -1.047965281155519420E-16 ) ) ;
#25322 = CARTESIAN_POINT ( 'NONE',  ( -46.00000000000000000, 0.000000000000000000, 81.00000000000001421 ) ) ;
#25323 = LINE ( 'NONE', #3188, #4994 ) ;
#25324 = DIRECTION ( 'NONE',  ( 1.000000000000000000, 0.000000000000000000, 0.000000000000000000 ) ) ;
#25325 =( REPRESENTATION_RELATIONSHIP ('NONE','NONE', #26607, #30285 ) REPRESENTATION_RELATIONSHIP_WITH_TRANSFORMATION ( #8195 )SHAPE_REPRESENTATION_RELATIONSHIP( ) );
#25326 = DIRECTION ( 'NONE',  ( -1.000000000000000000, 0.000000000000000000, 0.000000000000000000 ) ) ;
#25327 = CARTESIAN_POINT ( 'NONE',  ( 0.000000000000000000, 0.000000000000000000, 0.000000000000000000 ) ) ;
#25328 = ORIENTED_EDGE ( 'NONE', *, *, #3260, .T. ) ;
#25329 = AXIS2_PLACEMENT_3D ( 'NONE', #29797, #15722, #10517 ) ;
#25330 = EDGE_CURVE ( 'NONE', #16289, #4447, #17580, .T. ) ;
#25331 = CARTESIAN_POINT ( 'NONE',  ( -37.05926240293131713, -113.0000000000000000, 3.621475545821551734 ) ) ;
#25332 = DIRECTION ( 'NONE',  ( -1.000000000000000000, -1.734723475976807094E-16, -0.000000000000000000 ) ) ;
#25333 = DIRECTION ( 'NONE',  ( 0.000000000000000000, 0.9672551082808338307, -0.2538061376417690695 ) ) ;
#25334 = CARTESIAN_POINT ( 'NONE',  ( -46.00000000000000000, 0.000000000000000000, 0.000000000000000000 ) ) ;
#25335 = ADVANCED_FACE ( 'NONE', ( #30938 ), #28600, .T. ) ;
#25336 = ORIENTED_EDGE ( 'NONE', *, *, #5090, .F. ) ;
#25337 = CIRCLE ( 'NONE', #38, 7.999999999999992895 ) ;
#25338 = ORIENTED_EDGE ( 'NONE', *, *, #21370, .F. ) ;
#25339 = DIRECTION ( 'NONE',  ( -1.734723475976807094E-16, -0.4999999999999928946, -0.8660254037844427044 ) ) ;
#25340 = DIRECTION ( 'NONE',  ( 0.000000000000000000, 0.000000000000000000, 1.000000000000000000 ) ) ;
#25341 = EDGE_LOOP ( 'NONE', ( #6776, #33872 ) ) ;
#25342 = VERTEX_POINT ( 'NONE', #17413 ) ;
#25343 = VECTOR ( 'NONE', #6537, 1000.000000000000000 ) ;
#25344 = DIRECTION ( 'NONE',  ( -1.000000000000000000, 0.000000000000000000, 0.000000000000000000 ) ) ;
#25345 = DIRECTION ( 'NONE',  ( 1.000000000000000000, 0.000000000000000000, -0.000000000000000000 ) ) ;
#25346 = PRODUCT_CONTEXT ( 'NONE', #17203, 'mechanical' ) ;
#25347 = ADVANCED_FACE ( 'NONE', ( #28774 ), #17771, .T. ) ;
#25348 = CARTESIAN_POINT ( 'NONE',  ( -46.00000000000000000, 0.000000000000000000, 0.000000000000000000 ) ) ;
#25349 = VERTEX_POINT ( 'NONE', #6270 ) ;
#25350 = ORIENTED_EDGE ( 'NONE', *, *, #3993, .F. ) ;
#25351 = PRODUCT_RELATED_PRODUCT_CATEGORY ( 'part', '', ( #17537 ) ) ;
#25352 = CYLINDRICAL_SURFACE ( 'NONE', #14547, 52.00000000000000711 ) ;
#25353 = AXIS2_PLACEMENT_3D ( 'NONE', #1050, #33994, #9320 ) ;
#25354 = CARTESIAN_POINT ( 'NONE',  ( 38.00000000000000000, 1.391938065904714129E-14, -3.000000000000002665 ) ) ;
#25355 = EDGE_CURVE ( 'NONE', #30827, #31611, #26215, .T. ) ;
#25356 = ORIENTED_EDGE ( 'NONE', *, *, #1871, .F. ) ;
#25357 = CARTESIAN_POINT ( 'NONE',  ( 7.999999999999992895, -8.053585752061602321, -46.81126742072033409 ) ) ;
#25358 = CARTESIAN_POINT ( 'NONE',  ( -34.50000000000000000, -115.0140978167138712, -0.4997823525984417259 ) ) ;
#25359 = DIRECTION ( 'NONE',  ( 0.000000000000000000, 0.000000000000000000, 1.000000000000000000 ) ) ;
#25360 = FACE_BOUND ( 'NONE', #33318, .T. ) ;
#25361 = CARTESIAN_POINT ( 'NONE',  ( -39.00000000000000711, -114.9929510916434339, 12.26648026267477043 ) ) ;
#25362 = EDGE_CURVE ( 'NONE', #8016, #14329, #17236, .T. ) ;
#25363 = DIRECTION ( 'NONE',  ( 1.691777834109591064E-31, -1.187911941725854715E-31, 1.000000000000000000 ) ) ;
#25364 = CYLINDRICAL_SURFACE ( 'NONE', #16287, 8.000000000000001776 ) ;
#25365 = EDGE_CURVE ( 'NONE', #5282, #34581, #14530, .T. ) ;
#25366 = AXIS2_PLACEMENT_3D ( 'NONE', #24361, #5284, #5112 ) ;
#25367 = PRESENTATION_LAYER_ASSIGNMENT (  '', '', ( #5255 ) ) ;
#25368 = CARTESIAN_POINT ( 'NONE',  ( -34.50000000000000000, -114.2450133963102843, 8.522190569412378736 ) ) ;
#25370 = DIRECTION ( 'NONE',  ( -1.000000000000000000, 0.000000000000000000, 0.000000000000000000 ) ) ;
#25369 = AXIS2_PLACEMENT_3D ( 'NONE', #355, #16567, #5775 ) ;
#25371 = CYLINDRICAL_SURFACE ( 'NONE', #6920, 15.49899999999998457 ) ;
#25372 = LINE ( 'NONE', #31477, #32526 ) ;
#25373 = CARTESIAN_POINT ( 'NONE',  ( 0.000000000000000000, 0.000000000000000000, 0.000000000000000000 ) ) ;
#25374 = ORIENTED_EDGE ( 'NONE', *, *, #13008, .T. ) ;
#25375 = DIRECTION ( 'NONE',  ( 1.000000000000000000, -5.339440136655839175E-16, 0.000000000000000000 ) ) ;
#25376 = ORIENTED_EDGE ( 'NONE', *, *, #22975, .T. ) ;
#25377 = CARTESIAN_POINT ( 'NONE',  ( -40.02454729103296671, -115.1833782841879525, 6.659774454178448266 ) ) ;
#25378 = CARTESIAN_POINT ( 'NONE',  ( 8.000000000000007105, -7.613867765417476008, -5.679790370316101011 ) ) ;
#25379 = CARTESIAN_POINT ( 'NONE',  ( -35.50000000000000711, -112.0221129971568104, -0.7553032835231431319 ) ) ;
#25380 = EDGE_CURVE ( 'NONE', #15928, #9731, #23185, .T. ) ;
#25381 = ORIENTED_EDGE ( 'NONE', *, *, #13105, .F. ) ;
#25382 = ORIENTED_EDGE ( 'NONE', *, *, #32537, .F. ) ;
#25383 = CARTESIAN_POINT ( 'NONE',  ( 46.00000000000000000, 0.000000000000000000, 61.99999999999999289 ) ) ;
#25384 = CARTESIAN_POINT ( 'NONE',  ( 0.000000000000000000, 17.47118961583601759, 0.9861715913088272556 ) ) ;
#25385 = ORIENTED_EDGE ( 'NONE', *, *, #24034, .F. ) ;
#25386 = DIRECTION ( 'NONE',  ( -1.000000000000000000, -1.836970198721029934E-16, -0.000000000000000000 ) ) ;
#25387 = ORIENTED_EDGE ( 'NONE', *, *, #13290, .T. ) ;
#25388 = ORIENTED_EDGE ( 'NONE', *, *, #9369, .T. ) ;
#25389 = LINE ( 'NONE', #17081, #34362 ) ;
#25390 = CIRCLE ( 'NONE', #19051, 47.49900000000001654 ) ;
#25391 =( GEOMETRIC_REPRESENTATION_CONTEXT ( 3 ) GLOBAL_UNCERTAINTY_ASSIGNED_CONTEXT ( ( #34081 ) ) GLOBAL_UNIT_ASSIGNED_CONTEXT ( ( #32650, #27437, #2785 ) ) REPRESENTATION_CONTEXT ( 'NONE', 'WORKASPACE' ) );
#25392 = VECTOR ( 'NONE', #26814, 1000.000000000000000 ) ;
#25393 = EDGE_CURVE ( 'NONE', #9747, #6952, #15066, .T. ) ;
#25394 = DIRECTION ( 'NONE',  ( 0.000000000000000000, 0.000000000000000000, -1.000000000000000000 ) ) ;
#25395 = VERTEX_POINT ( 'NONE', #30759 ) ;
#25396 = ORIENTED_EDGE ( 'NONE', *, *, #24951, .F. ) ;
#25397 = CARTESIAN_POINT ( 'NONE',  ( -34.50000000000000000, -116.0215255531121983, -2.372276521655488857 ) ) ;
#25398 = EDGE_CURVE ( 'NONE', #932, #19590, #19307, .T. ) ;
#25399 = ADVANCED_FACE ( 'NONE', ( #29492 ), #26436, .T. ) ;
#25400 = DIRECTION ( 'NONE',  ( -0.000000000000000000, 0.1736481776669212829, 0.9848077530122096857 ) ) ;
#25401 = ORIENTED_EDGE ( 'NONE', *, *, #22168, .F. ) ;
#25402 = CARTESIAN_POINT ( 'NONE',  ( -36.62499999999902656, -114.9929510916434339, 13.11852480586264669 ) ) ;
#25403 = CARTESIAN_POINT ( 'NONE',  ( -38.99518666717493431, -113.9929510916434339, 12.74107470552714894 ) ) ;
#25404 = CARTESIAN_POINT ( 'NONE',  ( 70.00000000000001421, 46.40248769959371344, 64.62118051744215563 ) ) ;
#25405 = EDGE_CURVE ( 'NONE', #20378, #28584, #27932, .T. ) ;
#25406 = DIRECTION ( 'NONE',  ( 1.000000000000000000, 0.000000000000000000, 0.000000000000000000 ) ) ;
#25407 = ADVANCED_FACE ( 'NONE', ( #31640 ), #9528, .T. ) ;
#25408 = CARTESIAN_POINT ( 'NONE',  ( -34.50000000000000000, -113.9929510916434339, 10.50625754673587409 ) ) ;
#25409 = DIRECTION ( 'NONE',  ( 0.000000000000000000, -1.000000000000000000, 0.000000000000000000 ) ) ;
#25410 = CARTESIAN_POINT ( 'NONE',  ( -35.50000000000000711, -114.9929510916434339, 11.91443571948719971 ) ) ;
#25411 = CARTESIAN_POINT ( 'NONE',  ( 8.000000000000000000, 16.53603053422211389, 8.931325931664652273 ) ) ;
#25412 = CARTESIAN_POINT ( 'NONE',  ( -34.49999999999998579, -28.31857036507959791, 80.03062855292519373 ) ) ;
#25413 = ORIENTED_EDGE ( 'NONE', *, *, #22649, .T. ) ;
#25414 = ORIENTED_EDGE ( 'NONE', *, *, #5758, .T. ) ;
#25415 = CIRCLE ( 'NONE', #21953, 0.6000000000000028644 ) ;
#25416 = PRESENTATION_LAYER_ASSIGNMENT (  '', '', ( #14466 ) ) ;
#25417 = CARTESIAN_POINT ( 'NONE',  ( 0.000000000000000000, 0.000000000000000000, 50.00000000000000000 ) ) ;
#25418 = VECTOR ( 'NONE', #16861, 1000.000000000000000 ) ;
#25419 = FACE_OUTER_BOUND ( 'NONE', #2647, .T. ) ;
#25420 = ORIENTED_EDGE ( 'NONE', *, *, #8591, .F. ) ;
#25421 = FACE_OUTER_BOUND ( 'NONE', #6326, .T. ) ;
#25422 = ORIENTED_EDGE ( 'NONE', *, *, #2653, .F. ) ;
#25423 = CARTESIAN_POINT ( 'NONE',  ( -35.50000000000000000, -114.1807644833817648, -0.6247823525984269599 ) ) ;
#25424 = DIRECTION ( 'NONE',  ( -1.000000000000000000, 0.000000000000000000, 0.000000000000000000 ) ) ;
#25425 = CARTESIAN_POINT ( 'NONE',  ( -37.88768952767750164, -115.9754527089670262, 3.472274454178448266 ) ) ;
#25426 = ORIENTED_EDGE ( 'NONE', *, *, #7041, .F. ) ;
#25427 = CARTESIAN_POINT ( 'NONE',  ( -37.88768952767750164, -115.9754527089670262, 3.472274454178448266 ) ) ;
#25428 = ORIENTED_EDGE ( 'NONE', *, *, #35066, .F. ) ;
#25429 = AXIS2_PLACEMENT_3D ( 'NONE', #23768, #34756, #1990 ) ;
#25430 = FACE_OUTER_BOUND ( 'NONE', #21783, .T. ) ;
#25431 = CARTESIAN_POINT ( 'NONE',  ( -35.50000000000000000, -117.0140978167138854, -0.3747823525984422255 ) ) ;
#25432 = EDGE_LOOP ( 'NONE', ( #18634, #18729, #29605, #9193 ) ) ;
#25433 = ORIENTED_EDGE ( 'NONE', *, *, #5094, .F. ) ;
#25434 = CARTESIAN_POINT ( 'NONE',  ( -38.37230871539094323, -112.5438815906447729, 3.941024454178448710 ) ) ;
#25435 = FILL_AREA_STYLE_COLOUR ( '', #8127 ) ;
#25436 = DIRECTION ( 'NONE',  ( -1.000000000000000000, 0.000000000000000000, 0.000000000000000000 ) ) ;
#25437 = EDGE_LOOP ( 'NONE', ( #26323, #20669, #33178, #31750 ) ) ;
#25438 = VERTEX_POINT ( 'NONE', #35083 ) ;
#25439 = CARTESIAN_POINT ( 'NONE',  ( -34.50000000000000000, -112.6043641208289188, 1.789429170677330649 ) ) ;
#25440 = CYLINDRICAL_SURFACE ( 'NONE', #30954, 13.99999999999999822 ) ;
#25441 = EDGE_CURVE ( 'NONE', #13682, #20133, #1767, .T. ) ;
#25442 = AXIS2_PLACEMENT_3D ( 'NONE', #17519, #28522, #1330 ) ;
#25443 = AXIS2_PLACEMENT_3D ( 'NONE', #14880, #28398, #12195 ) ;
#25444 = ORIENTED_EDGE ( 'NONE', *, *, #33488, .F. ) ;
#25445 = AXIS2_PLACEMENT_3D ( 'NONE', #25847, #23120, #31587 ) ;
#25446 = EDGE_LOOP ( 'NONE', ( #35377, #12476, #29363, #23506 ) ) ;
#25447 = DIRECTION ( 'NONE',  ( 0.000000000000000000, 0.000000000000000000, 1.000000000000000000 ) ) ;
#25448 = CARTESIAN_POINT ( 'NONE',  ( -36.24999999999983658, -113.9929510916434339, 13.11852480586264846 ) ) ;
#25449 = FACE_OUTER_BOUND ( 'NONE', #33741, .T. ) ;
#25450 = CARTESIAN_POINT ( 'NONE',  ( 0.000000000000000000, -17.06000345190446055, 10.43821259704015425 ) ) ;
#25451 = CARTESIAN_POINT ( 'NONE',  ( -34.50000000000000000, -113.6974040292745656, 2.970979214817929481 ) ) ;
#25452 = CARTESIAN_POINT ( 'NONE',  ( -38.25557080230232998, -115.9929510916434481, 13.92914543265419525 ) ) ;
#25453 = UNCERTAINTY_MEASURE_WITH_UNIT (LENGTH_MEASURE( 1.000000000000000082E-05 ), #11202, 'distance_accuracy_value', 'NONE');
#25454 = DIRECTION ( 'NONE',  ( 0.000000000000000000, 0.000000000000000000, 1.000000000000000000 ) ) ;
#25455 = DIRECTION ( 'NONE',  ( 0.000000000000000000, 0.000000000000000000, -1.000000000000000000 ) ) ;
#25456 = LINE ( 'NONE', #776, #26910 ) ;
#25457 = FACE_OUTER_BOUND ( 'NONE', #34056, .T. ) ;
#25458 = DIRECTION ( 'NONE',  ( 1.000000000000000000, 0.000000000000000000, 0.000000000000000000 ) ) ;
#25459 = ORIENTED_EDGE ( 'NONE', *, *, #19989, .F. ) ;
#25460 = CARTESIAN_POINT ( 'NONE',  ( 7.999999999999992895, -47.49120266317497396, 0.8606222198173640869 ) ) ;
#25461 = DIRECTION ( 'NONE',  ( 1.000000000000000000, 0.000000000000000000, 0.000000000000000000 ) ) ;
#25462 = AXIS2_PLACEMENT_3D ( 'NONE', #1866, #34807, #34266 ) ;
#25463 = VECTOR ( 'NONE', #3269, 1000.000000000000114 ) ;
#25464 = DIRECTION ( 'NONE',  ( 0.000000000000000000, 0.000000000000000000, 1.000000000000000000 ) ) ;
#25465 = DIRECTION ( 'NONE',  ( -1.000000000000000000, 0.000000000000000000, 0.000000000000000000 ) ) ;
#25466 = DIRECTION ( 'NONE',  ( 8.645950338799857827E-17, -6.938893903907203726E-17, -1.000000000000000000 ) ) ;
#25467 = CARTESIAN_POINT ( 'NONE',  ( 0.000000000000000000, -17.50309955389579386, -43.60271849949381817 ) ) ;
#25468 = ORIENTED_EDGE ( 'NONE', *, *, #18898, .F. ) ;
#25469 = FACE_OUTER_BOUND ( 'NONE', #13416, .T. ) ;
#25470 = DIRECTION ( 'NONE',  ( 0.000000000000000000, 0.000000000000000000, 1.000000000000000000 ) ) ;
#25471 = DIRECTION ( 'NONE',  ( 0.000000000000000000, 0.000000000000000000, -1.000000000000000000 ) ) ;
#25472 = ORIENTED_EDGE ( 'NONE', *, *, #10929, .T. ) ;
#25473 = ORIENTED_EDGE ( 'NONE', *, *, #8778, .F. ) ;
#25474 = CARTESIAN_POINT ( 'NONE',  ( -35.99999999999999289, -113.9407375970686758, 6.996475545821551734 ) ) ;
#25475 = ORIENTED_EDGE ( 'NONE', *, *, #15461, .F. ) ;
#25476 = FILL_AREA_STYLE_COLOUR ( '', #6385 ) ;
#25478 = ORIENTED_EDGE ( 'NONE', *, *, #10829, .F. ) ;
#25477 = CIRCLE ( 'NONE', #33505, 9.499000000000011212 ) ;
#25479 = EDGE_LOOP ( 'NONE', ( #34206, #32038, #30147, #6370 ) ) ;
#25480 = LINE ( 'NONE', #22231, #21768 ) ;
#25481 = EDGE_CURVE ( 'NONE', #741, #23024, #26816, .T. ) ;
#25482 = CARTESIAN_POINT ( 'NONE',  ( -35.50000000000000711, -114.9307644833806137, -1.624782352598427959 ) ) ;
#25483 = CARTESIAN_POINT ( 'NONE',  ( -10.00000000000000000, 0.000000000000000000, 0.000000000000000000 ) ) ;
#25484 = CIRCLE ( 'NONE', #3086, 3.799999999999999822 ) ;
#25485 = CARTESIAN_POINT ( 'NONE',  ( -35.50000000000000711, -114.9929510916434339, 12.26648026267477221 ) ) ;
#25486 = CIRCLE ( 'NONE', #14534, 8.000000000000005329 ) ;
#25487 = CYLINDRICAL_SURFACE ( 'NONE', #28719, 47.49900000000001654 ) ;
#25488 = EDGE_CURVE ( 'NONE', #12307, #13559, #29099, .T. ) ;
#25489 = DIRECTION ( 'NONE',  ( -1.000000000000000000, 0.000000000000000000, 0.000000000000000000 ) ) ;
#25490 = CARTESIAN_POINT ( 'NONE',  ( -34.50000000000000000, -114.9912366357066986, 10.44580456020104720 ) ) ;
#25491 = CYLINDRICAL_SURFACE ( 'NONE', #34084, 20.00000000000000711 ) ;
#25492 = DIRECTION ( 'NONE',  ( -1.000000000000000000, -0.000000000000000000, -0.000000000000000000 ) ) ;
#25493 = ORIENTED_EDGE ( 'NONE', *, *, #14812, .T. ) ;
#25494 = CARTESIAN_POINT ( 'NONE',  ( -35.50000000000000000, -114.1928420708668028, 8.515919878418792166 ) ) ;
#25495 = CARTESIAN_POINT ( 'NONE',  ( -35.50000000000000711, -112.8655373925166572, 1.864575885149403423 ) ) ;
#25496 = CARTESIAN_POINT ( 'NONE',  ( 7.999999999999992895, 18.53613841426858500, -48.58406706613885007 ) ) ;
#25497 = CARTESIAN_POINT ( 'NONE',  ( 0.000000000000000000, 13.85708833600033252, -45.43276465116652219 ) ) ;
#25498 = AXIS2_PLACEMENT_3D ( 'NONE', #21926, #24121, #35284 ) ;
#25499 = AXIS2_PLACEMENT_3D ( 'NONE', #15366, #9634, #34485 ) ;
#25500 = CARTESIAN_POINT ( 'NONE',  ( 7.999999999999992895, 0.000000000000000000, 0.000000000000000000 ) ) ;
#25501 = DIRECTION ( 'NONE',  ( 1.000000000000000000, -4.524158825347490025E-15, -1.174092375852883357E-15 ) ) ;
#25502 = CARTESIAN_POINT ( 'NONE',  ( 7.999999999999992895, 0.000000000000000000, 0.000000000000000000 ) ) ;
#25503 = CARTESIAN_POINT ( 'NONE',  ( 7.999999999999992895, 3.840921266750509488, -47.34345070675166767 ) ) ;
#25504 = ORIENTED_EDGE ( 'NONE', *, *, #28219, .F. ) ;
#25505 = CARTESIAN_POINT ( 'NONE',  ( -36.33479806579561000, -114.7490116281687165, 1.691024454178448932 ) ) ;
#25506 = CARTESIAN_POINT ( 'NONE',  ( -21.15833593587365513, -25.27980021920989984, 89.21410161513770731 ) ) ;
#25507 = DIRECTION ( 'NONE',  ( 0.000000000000000000, -0.1253332335643113360, 0.9921147013144769877 ) ) ;
#25508 = VERTEX_POINT ( 'NONE', #4299 ) ;
#25509 = ORIENTED_EDGE ( 'NONE', *, *, #19133, .T. ) ;
#25510 = AXIS2_PLACEMENT_3D ( 'NONE', #9740, #20700, #26131 ) ;
#25511 = CARTESIAN_POINT ( 'NONE',  ( -34.50000000000001421, -18.77980021920990694, 100.4724318643354053 ) ) ;
#25512 = AXIS2_PLACEMENT_3D ( 'NONE', #14357, #10970, #27879 ) ;
#25513 = LINE ( 'NONE', #4098, #27310 ) ;
#25514 = ORIENTED_EDGE ( 'NONE', *, *, #34, .T. ) ;
#25515 = CARTESIAN_POINT ( 'NONE',  ( -34.92058450342251064, -116.1632251905417945, 7.691024454178450043 ) ) ;
#25516 = AXIS2_PLACEMENT_3D ( 'NONE', #7081, #21112, #34821 ) ;
#25517 = ORIENTED_EDGE ( 'NONE', *, *, #15444, .F. ) ;
#25518 = ADVANCED_FACE ( 'NONE', ( #7512 ), #34537, .T. ) ;
#25519 = DIRECTION ( 'NONE',  ( 0.000000000000000000, 0.000000000000000000, 1.000000000000000000 ) ) ;
#25520 = EDGE_CURVE ( 'NONE', #13855, #192, #13119, .T. ) ;
#25521 = CYLINDRICAL_SURFACE ( 'NONE', #35556, 20.00000000000000355 ) ;
#25522 = SHAPE_DEFINITION_REPRESENTATION ( #22712, #7982 ) ;
#25523 = CARTESIAN_POINT ( 'NONE',  ( 7.999999999999992895, 49.25004636492413113, -16.68630974939708267 ) ) ;
#25524 = ORIENTED_EDGE ( 'NONE', *, *, #30074, .F. ) ;
#25525 = VERTEX_POINT ( 'NONE', #21002 ) ;
#25526 = VECTOR ( 'NONE', #29486, 1000.000000000000227 ) ;
#25527 = CARTESIAN_POINT ( 'NONE',  ( 0.000000000000000000, 11.06713717293261467, -13.55483219355716606 ) ) ;
#25528 = CARTESIAN_POINT ( 'NONE',  ( 65.00000000000001421, 58.94749845961094792, 75.40996905927893579 ) ) ;
#25529 = EDGE_CURVE ( 'NONE', #13350, #34564, #1592, .T. ) ;
#25530 = ORIENTED_EDGE ( 'NONE', *, *, #26046, .T. ) ;
#25531 = DIRECTION ( 'NONE',  ( 0.000000000000000000, 0.000000000000000000, 1.000000000000000000 ) ) ;
#25532 = EDGE_CURVE ( 'NONE', #18497, #30005, #14122, .T. ) ;
#25533 = CARTESIAN_POINT ( 'NONE',  ( -34.50000000000000000, -115.0140978167140986, -0.6247823525984417259 ) ) ;
#25534 = CARTESIAN_POINT ( 'NONE',  ( 54.99999999999999289, -64.99999999999997158, -25.00000000000000000 ) ) ;
#25535 = CARTESIAN_POINT ( 'NONE',  ( 0.2142857142857085284, -10.49781318335649161, -1.200000000000006617 ) ) ;
#25536 = EDGE_CURVE ( 'NONE', #6545, #35594, #18726, .T. ) ;
#25537 = APPLICATION_CONTEXT ( 'automotive_design' ) ;
#25538 = CIRCLE ( 'NONE', #20907, 9.499000000000009436 ) ;
#25539 = CARTESIAN_POINT ( 'NONE',  ( -34.50000000000000000, -115.9382890315277308, 10.02636389016632812 ) ) ;
#25540 = AXIS2_PLACEMENT_3D ( 'NONE', #2437, #728, #32848 ) ;
#25541 = FACE_OUTER_BOUND ( 'NONE', #25214, .T. ) ;
#25542 = DIRECTION ( 'NONE',  ( 1.000000000000000000, 0.000000000000000000, 0.000000000000000000 ) ) ;
#25543 = CARTESIAN_POINT ( 'NONE',  ( -39.00000000000000711, -114.9929510916434339, 12.56351784598954779 ) ) ;
#25544 = DIRECTION ( 'NONE',  ( 0.000000000000000000, 0.4817536741017100499, 0.8763066800438665815 ) ) ;
#25545 = FACE_OUTER_BOUND ( 'NONE', #12393, .T. ) ;
#25546 = DIRECTION ( 'NONE',  ( 0.000000000000000000, 0.000000000000000000, 1.000000000000000000 ) ) ;
#25547 = DIRECTION ( 'NONE',  ( 1.000000000000000000, 0.000000000000000000, 0.000000000000000000 ) ) ;
#25548 = ORIENTED_EDGE ( 'NONE', *, *, #10815, .T. ) ;
#25549 = FACE_OUTER_BOUND ( 'NONE', #1754, .T. ) ;
#25550 = ORIENTED_EDGE ( 'NONE', *, *, #4997, .F. ) ;
#25551 = CARTESIAN_POINT ( 'NONE',  ( -39.07941549657749647, -116.1632251905417803, 7.558975545821551734 ) ) ;
#25552 = DIRECTION ( 'NONE',  ( 1.000000000000000000, 0.000000000000000000, 0.000000000000000000 ) ) ;
#25553 = EDGE_CURVE ( 'NONE', #26780, #19478, #3842, .T. ) ;
#25554 = CARTESIAN_POINT ( 'NONE',  ( -35.50000000000000711, -116.0012805033554883, -0.7876962586524312027 ) ) ;
#25555 = ORIENTED_EDGE ( 'NONE', *, *, #24840, .T. ) ;
#25556 = ORIENTED_EDGE ( 'NONE', *, *, #30791, .T. ) ;
#25557 = CARTESIAN_POINT ( 'NONE',  ( -42.49999999999999289, -28.69486372867102375, 88.29903810567654432 ) ) ;
#25558 = DIRECTION ( 'NONE',  ( 0.000000000000000000, -0.9822872507286904975, 0.1873813145857149698 ) ) ;
#25559 = ORIENTED_EDGE ( 'NONE', *, *, #2029, .T. ) ;
#25560 = ORIENTED_EDGE ( 'NONE', *, *, #7911, .T. ) ;
#25561 = CIRCLE ( 'NONE', #4857, 10.99999999999999645 ) ;
#25562 = EDGE_CURVE ( 'NONE', #28677, #14718, #18184, .T. ) ;
#25563 = CYLINDRICAL_SURFACE ( 'NONE', #17686, 19.99999999999998579 ) ;
#25564 = CIRCLE ( 'NONE', #30721, 47.49900000000001654 ) ;
#25565 = ORIENTED_EDGE ( 'NONE', *, *, #30394, .T. ) ;
#25566 = ORIENTED_EDGE ( 'NONE', *, *, #35060, .F. ) ;
#25567 = EDGE_CURVE ( 'NONE', #35528, #708, #21365, .T. ) ;
#25568 = CARTESIAN_POINT ( 'NONE',  ( -34.97545270896703329, -114.7691647218148745, 4.090225545821551734 ) ) ;
#25569 = ADVANCED_FACE ( 'NONE', ( #18130 ), #23910, .T. ) ;
#25570 = SURFACE_STYLE_USAGE ( .BOTH. , #28266 ) ;
#25571 = CIRCLE ( 'NONE', #27297, 14.70000000000000107 ) ;
#25572 = DIRECTION ( 'NONE',  ( -1.000000000000000000, -0.000000000000000000, 0.000000000000000000 ) ) ;
#25573 = VERTEX_POINT ( 'NONE', #34903 ) ;
#25574 = ORIENTED_EDGE ( 'NONE', *, *, #25273, .F. ) ;
#25575 = CARTESIAN_POINT ( 'NONE',  ( -35.50000000000000000, -112.8832452823708792, -2.621568770093253953 ) ) ;
#25576 = DIRECTION ( 'NONE',  ( 0.000000000000000000, -0.9848077530122095746, 0.1736481776669212551 ) ) ;
#25577 = ORIENTED_EDGE ( 'NONE', *, *, #28455, .T. ) ;
#25578 = CARTESIAN_POINT ( 'NONE',  ( -36.87500000000098055, -114.9929510916434339, 13.11852480586264669 ) ) ;
#25579 = EDGE_CURVE ( 'NONE', #34823, #19114, #32184, .T. ) ;
#25580 = CARTESIAN_POINT ( 'NONE',  ( -38.98077402996267438, -113.9929510916434339, 12.86289566494346204 ) ) ;
#25581 = CARTESIAN_POINT ( 'NONE',  ( 0.1085714285714300953, -3.798448662927791819, 0.000000000000000000 ) ) ;
#25582 = CARTESIAN_POINT ( 'NONE',  ( 4.000000000000003553, 25.61928775981107265, -45.25098998563451147 ) ) ;
#25583 = CARTESIAN_POINT ( 'NONE',  ( -37.69578139638701941, -113.9929510916434339, 14.10650203519847778 ) ) ;
#25584 = DIRECTION ( 'NONE',  ( -1.000000000000000000, 0.000000000000000000, 0.000000000000000000 ) ) ;
#25585 = CARTESIAN_POINT ( 'NONE',  ( -35.95915003344517658, -114.9929510916434339, 13.11692036158763308 ) ) ;
#25586 = CARTESIAN_POINT ( 'NONE',  ( 8.000000000000000000, 0.000000000000000000, 0.000000000000000000 ) ) ;
#25587 = ORIENTED_EDGE ( 'NONE', *, *, #29353, .T. ) ;
#25589 = AXIS2_PLACEMENT_3D ( 'NONE', #33973, #25877, #14868 ) ;
#25588 = CARTESIAN_POINT ( 'NONE',  ( 8.000000000000000000, 0.000000000000000000, 0.000000000000000000 ) ) ;
#25590 = FACE_OUTER_BOUND ( 'NONE', #5685, .T. ) ;
#25591 = ORIENTED_EDGE ( 'NONE', *, *, #4602, .F. ) ;
#25592 = CARTESIAN_POINT ( 'NONE',  ( -35.50000000000000711, -114.9929510916434339, 10.51725893871048889 ) ) ;
#25593 = VERTEX_POINT ( 'NONE', #7680 ) ;
#25594 = DIRECTION ( 'NONE',  ( -1.000000000000000000, 0.000000000000000000, 0.000000000000000000 ) ) ;
#25595 = CARTESIAN_POINT ( 'NONE',  ( 8.000000000000007105, 0.000000000000000000, 0.000000000000000000 ) ) ;
#25596 = EDGE_CURVE ( 'NONE', #22478, #32982, #16457, .T. ) ;
#25597 = VECTOR ( 'NONE', #26623, 1000.000000000000000 ) ;
#25598 = EDGE_LOOP ( 'NONE', ( #18384, #21467, #16360, #14963 ) ) ;
#25599 = CARTESIAN_POINT ( 'NONE',  ( 0.000000000000000000, -19.77827456857337651, 2.969824084036395639 ) ) ;
#25600 = EDGE_LOOP ( 'NONE', ( #21369, #13980, #5207, #16192 ) ) ;
#25601 = CIRCLE ( 'NONE', #14648, 22.00000000000000000 ) ;
#25602 = CARTESIAN_POINT ( 'NONE',  ( -35.50000000000000000, -115.0140978167138712, -0.1247823525984438492 ) ) ;
#25603 = DIRECTION ( 'NONE',  ( 0.000000000000000000, 0.000000000000000000, 1.000000000000000000 ) ) ;
#25604 = EDGE_CURVE ( 'NONE', #1850, #2693, #5361, .T. ) ;
#25605 = CARTESIAN_POINT ( 'NONE',  ( -35.00000000000000000, -114.0592624029313242, 1.503524454178448710 ) ) ;
#25606 = ORIENTED_EDGE ( 'NONE', *, *, #17908, .T. ) ;
#25607 = CARTESIAN_POINT ( 'NONE',  ( -36.11231047232249125, -112.0245472910329880, 4.222274454178449155 ) ) ;
#25608 = DIRECTION ( 'NONE',  ( 0.02857142857143298367, -0.9995917534020514195, -4.555780455966494792E-16 ) ) ;
#25609 = CARTESIAN_POINT ( 'NONE',  ( -35.50000000000000711, -115.3362660311619692, -1.573728109101206085 ) ) ;
#25610 = ORIENTED_EDGE ( 'NONE', *, *, #18232, .F. ) ;
#25611 = VERTEX_POINT ( 'NONE', #32895 ) ;
#25612 = ADVANCED_FACE ( 'NONE', ( #19537 ), #22250, .T. ) ;
#25613 = CYLINDRICAL_SURFACE ( 'NONE', #9626, 7.199999999999994849 ) ;
#25614 = ADVANCED_FACE ( 'NONE', ( #10934 ), #11110, .T. ) ;
#25615 = LINE ( 'NONE', #27950, #31649 ) ;
#25616 = VERTEX_POINT ( 'NONE', #27675 ) ;
#25617 = EDGE_LOOP ( 'NONE', ( #33354, #9699, #13358, #24279 ) ) ;
#25618 = CARTESIAN_POINT ( 'NONE',  ( -34.50000000000000000, -112.6605569508015350, 1.812590711673265575 ) ) ;
#25619 = CARTESIAN_POINT ( 'NONE',  ( 39.30000000000000426, 7.219292880973646134E-15, 0.000000000000000000 ) ) ;
#25620 = CLOSED_SHELL ( 'NONE', ( #16300, #7258, #14925, #33259, #25635, #22943, #9497, #18065, #31025, #23371, #6982, #13046, #15457, #26238, #23603, #35248, #1586, #14446, #18256, #1951, #32063, #17125, #26288, #25038, #14970, #27957, #25194, #12836, #30226, #8477, #19351, #13273, #4408, #29052, #6363, #23564, #34432, #9096, #33631, #24928, #6726, #6078, #7943, #6002, #9574, #31255, #19289 ) ) ;
#25621 = ORIENTED_EDGE ( 'NONE', *, *, #29094, .F. ) ;
#25622 = ORIENTED_EDGE ( 'NONE', *, *, #18304, .F. ) ;
#25623 = CARTESIAN_POINT ( 'NONE',  ( 7.999999999999992895, -34.03046037009232094, -33.13733193845841640 ) ) ;
#25624 = AXIS2_PLACEMENT_3D ( 'NONE', #7119, #6944, #4445 ) ;
#25625 = CARTESIAN_POINT ( 'NONE',  ( -37.99599240977853754, -113.9929510916434339, 12.68378527132499656 ) ) ;
#25626 = DIRECTION ( 'NONE',  ( -1.000000000000000000, -0.000000000000000000, -0.000000000000000000 ) ) ;
#25627 = CARTESIAN_POINT ( 'NONE',  ( 0.000000000000000000, -20.99948489194393275, -42.60488980472803888 ) ) ;
#25628 = CARTESIAN_POINT ( 'NONE',  ( -36.31249999999994316, -113.9929510916434339, 13.11852480586264846 ) ) ;
#25629 = CARTESIAN_POINT ( 'NONE',  ( -35.83891589277641287, -115.9929510916434481, 13.09299768411358400 ) ) ;
#25630 = CIRCLE ( 'NONE', #34835, 3.800000000000018918 ) ;
#25631 = DIRECTION ( 'NONE',  ( -1.000000000000000000, -0.000000000000000000, -0.000000000000000000 ) ) ;
#25632 = CARTESIAN_POINT ( 'NONE',  ( 8.000000000000000000, 0.000000000000000000, 0.000000000000000000 ) ) ;
#25633 = DIRECTION ( 'NONE',  ( -1.000000000000000000, 0.000000000000000000, -0.000000000000000000 ) ) ;
#25634 = DIRECTION ( 'NONE',  ( 0.000000000000000000, 0.000000000000000000, -1.000000000000000000 ) ) ;
#25635 = ADVANCED_FACE ( 'NONE', ( #30543 ), #5190, .T. ) ;
#25636 = ORIENTED_EDGE ( 'NONE', *, *, #34839, .T. ) ;
#25637 = CARTESIAN_POINT ( 'NONE',  ( 3.799999999999999822, 0.000000000000000000, 60.00000000000000000 ) ) ;
#25638 = CARTESIAN_POINT ( 'NONE',  ( 0.000000000000000000, -42.03146605346771025, -22.12489237027362421 ) ) ;
#25639 = EDGE_CURVE ( 'NONE', #17618, #23216, #2666, .T. ) ;
#25640 = AXIS2_PLACEMENT_3D ( 'NONE', #29812, #35045, #15377 ) ;
#25641 = CARTESIAN_POINT ( 'NONE',  ( 8.000000000000000000, -4.460989585140847424, -16.92083251265332322 ) ) ;
#25642 = DIRECTION ( 'NONE',  ( 1.783119874454246424E-31, 1.187911941725854497E-31, -1.000000000000000000 ) ) ;
#25643 = CARTESIAN_POINT ( 'NONE',  ( 0.000000000000000000, 44.61570720899095477, -14.73072383765580717 ) ) ;
#25644 = CARTESIAN_POINT ( 'NONE',  ( 0.000000000000000000, 0.3151488735050472778, -11.27190672109269087 ) ) ;
#25645 = VECTOR ( 'NONE', #22372, 1000.000000000000000 ) ;
#25646 = CIRCLE ( 'NONE', #4399, 0.1999999999999992339 ) ;
#25647 = ORIENTED_EDGE ( 'NONE', *, *, #20666, .F. ) ;
#25648 = AXIS2_PLACEMENT_3D ( 'NONE', #33183, #30489, #6337 ) ;
#25649 = DIRECTION ( 'NONE',  ( 0.000000000000000000, -0.1253332335643113360, 0.9921147013144769877 ) ) ;
#25650 = DIRECTION ( 'NONE',  ( -1.174092375852890260E-15, 4.222049128630259891E-16, 1.000000000000000000 ) ) ;
#25651 = CARTESIAN_POINT ( 'NONE',  ( -39.49999999999999289, -1.387778780781445676E-14, 110.0000000000000000 ) ) ;
#25652 = ORIENTED_EDGE ( 'NONE', *, *, #7701, .F. ) ;
#25653 = ORIENTED_EDGE ( 'NONE', *, *, #26455, .T. ) ;
#25654 = CARTESIAN_POINT ( 'NONE',  ( -36.33479806579561000, -114.7490116281687165, 4.691024454178447378 ) ) ;
#25655 = ORIENTED_EDGE ( 'NONE', *, *, #5805, .F. ) ;
#25656 = AXIS2_PLACEMENT_3D ( 'NONE', #20923, #3686, #25835 ) ;
#25657 = PRESENTATION_STYLE_ASSIGNMENT (( #19344 ) ) ;
#25658 = AXIS2_PLACEMENT_3D ( 'NONE', #6093, #31294, #25727 ) ;
#25659 = VERTEX_POINT ( 'NONE', #29849 ) ;
#25660 = ORIENTED_EDGE ( 'NONE', *, *, #8641, .T. ) ;
#25661 = FACE_OUTER_BOUND ( 'NONE', #16018, .T. ) ;
#25662 = LINE ( 'NONE', #993, #26390 ) ;
#25663 = LINE ( 'NONE', #9439, #32892 ) ;
#25664 = CIRCLE ( 'NONE', #10132, 20.00000000000001066 ) ;
#25665 = CARTESIAN_POINT ( 'NONE',  ( -35.83891589277640577, -114.9929510916434339, 13.09299768411358222 ) ) ;
#25666 = DIRECTION ( 'NONE',  ( 0.000000000000000000, 0.5877852522924681411, 0.8090169943749510040 ) ) ;
#25667 = DIRECTION ( 'NONE',  ( -0.000000000000000000, 0.000000000000000000, -1.000000000000000000 ) ) ;
#25668 = CIRCLE ( 'NONE', #17595, 4.000000000000003553 ) ;
#25669 = AXIS2_PLACEMENT_3D ( 'NONE', #22827, #33825, #9149 ) ;
#25670 = CARTESIAN_POINT ( 'NONE',  ( -34.50000000000000000, -114.6604609523327838, 9.751889438017201428 ) ) ;
#25671 = FACE_OUTER_BOUND ( 'NONE', #19254, .T. ) ;
#25672 = CIRCLE ( 'NONE', #31417, 20.00000000000000355 ) ;
#25673 = PLANE ( 'NONE',  #2555 ) ;
#25674 = VERTEX_POINT ( 'NONE', #10754 ) ;
#25675 = CARTESIAN_POINT ( 'NONE',  ( -35.50000000000000000, -115.9710363517788068, 10.20486393345008835 ) ) ;
#25676 = CARTESIAN_POINT ( 'NONE',  ( 7.999999999999992895, 46.19362259308845609, -8.585149169757999132 ) ) ;
#25677 = LINE ( 'NONE', #9280, #31738 ) ;
#25678 = AXIS2_PLACEMENT_3D ( 'NONE', #19292, #30302, #14070 ) ;
#25679 = DIRECTION ( 'NONE',  ( -1.000000000000000000, 0.000000000000000000, 0.000000000000000000 ) ) ;
#25680 = DIRECTION ( 'NONE',  ( 0.000000000000000000, -0.2486898871648415554, -0.9685831611286345177 ) ) ;
#25681 = CARTESIAN_POINT ( 'NONE',  ( -42.49999999999999289, -21.76666049839546346, 85.70096189432329936 ) ) ;
#25682 = CARTESIAN_POINT ( 'NONE',  ( -34.49999999999998579, -14.17619866229204106, 94.12476896299857287 ) ) ;
#25683 = EDGE_CURVE ( 'NONE', #5115, #12651, #31995, .T. ) ;
#25684 = CARTESIAN_POINT ( 'NONE',  ( 0.000000000000000000, 0.000000000000000000, 52.00000000000000711 ) ) ;
#25685 = CYLINDRICAL_SURFACE ( 'NONE', #8614, 4.000000000000000000 ) ;
#25686 = ORIENTED_EDGE ( 'NONE', *, *, #25971, .T. ) ;
#25687 = CARTESIAN_POINT ( 'NONE',  ( -37.74901162816869515, -114.6652019342044042, 2.066024454178448710 ) ) ;
#25688 = DIRECTION ( 'NONE',  ( 0.000000000000000000, 0.000000000000000000, -1.000000000000000000 ) ) ;
#25689 = DIRECTION ( 'NONE',  ( -1.000000000000000000, 0.000000000000000000, 0.000000000000000000 ) ) ;
#25690 = VERTEX_POINT ( 'NONE', #19371 ) ;
#25691 = AXIS2_PLACEMENT_3D ( 'NONE', #9364, #31331, #6657 ) ;
#25692 = ORIENTED_EDGE ( 'NONE', *, *, #23772, .T. ) ;
#25693 = DIRECTION ( 'NONE',  ( -1.000000000000000000, -1.836970198721029934E-16, -0.000000000000000000 ) ) ;
#25694 = AXIS2_PLACEMENT_3D ( 'NONE', #19472, #30470, #3109 ) ;
#25695 = DIRECTION ( 'NONE',  ( -1.000000000000000000, 0.000000000000000000, 0.000000000000000000 ) ) ;
#25696 = ORIENTED_EDGE ( 'NONE', *, *, #938, .F. ) ;
#25697 = CARTESIAN_POINT ( 'NONE',  ( -38.30190309005061522, -116.9754527089670546, 7.972274454178450043 ) ) ;
#25698 = EDGE_CURVE ( 'NONE', #16117, #34424, #2691, .T. ) ;
#25699 = ORIENTED_EDGE ( 'NONE', *, *, #18595, .T. ) ;
#25700 = MECHANICAL_DESIGN_GEOMETRIC_PRESENTATION_REPRESENTATION (  '', ( #29113 ), #29143 ) ;
#25701 = AXIS2_PLACEMENT_3D ( 'NONE', #1725, #32489, #18271 ) ;
#25702 = CIRCLE ( 'NONE', #22237, 10.00000000000000000 ) ;
#25703 = LINE ( 'NONE', #12187, #18693 ) ;
#25704 = DIRECTION ( 'NONE',  ( -1.000000000000000000, 0.000000000000000000, 0.000000000000000000 ) ) ;
#25705 = AXIS2_PLACEMENT_3D ( 'NONE', #14953, #33692, #12269 ) ;
#25706 = APPLICATION_PROTOCOL_DEFINITION ( 'draft international standard', 'automotive_design', 1998, #15835 ) ;
#25707 = CARTESIAN_POINT ( 'NONE',  ( 0.000000000000000000, 46.87740477351717061, -3.172455868805379442 ) ) ;
#25709 = ORIENTED_EDGE ( 'NONE', *, *, #17176, .T. ) ;
#25708 = AXIS2_PLACEMENT_3D ( 'NONE', #17733, #23314, #4792 ) ;
#25710 = VERTEX_POINT ( 'NONE', #33072 ) ;
#25711 = DIRECTION ( 'NONE',  ( 0.000000000000000000, 0.000000000000000000, 1.000000000000000000 ) ) ;
#25712 = DIRECTION ( 'NONE',  ( -1.000000000000000000, 0.000000000000000000, 0.000000000000000000 ) ) ;
#25713 = VERTEX_POINT ( 'NONE', #32716 ) ;
#25714 = CARTESIAN_POINT ( 'NONE',  ( 0.000000000000000000, -11.27190672109260028, -0.3151488735048807444 ) ) ;
#25715 = AXIS2_PLACEMENT_3D ( 'NONE', #13797, #16703, #16536 ) ;
#25716 = CARTESIAN_POINT ( 'NONE',  ( -34.50000000000000000, -112.9185811467682754, 1.870920967077121411 ) ) ;
#25717 = DIRECTION ( 'NONE',  ( 0.000000000000000000, 0.000000000000000000, -1.000000000000000000 ) ) ;
#25718 = PLANE ( 'NONE',  #25353 ) ;
#25719 = CARTESIAN_POINT ( 'NONE',  ( -34.50000000000000000, -114.3496480102005251, 8.538090462223289379 ) ) ;
#25720 = CIRCLE ( 'NONE', #4450, 4.800000000000000711 ) ;
#25721 = CYLINDRICAL_SURFACE ( 'NONE', #13999, 20.00000000000000711 ) ;
#25722 = DIRECTION ( 'NONE',  ( 0.000000000000000000, 0.000000000000000000, 1.000000000000000000 ) ) ;
#25723 = CARTESIAN_POINT ( 'NONE',  ( -34.50000000000000000, -114.4680894751352156, 8.562575367713533225 ) ) ;
#25724 = FACE_OUTER_BOUND ( 'NONE', #33521, .T. ) ;
#25725 = LINE ( 'NONE', #14712, #19004 ) ;
#25726 = AXIS2_PLACEMENT_3D ( 'NONE', #12816, #16019, #10101 ) ;
#25727 = DIRECTION ( 'NONE',  ( 0.000000000000000000, 0.000000000000000000, 1.000000000000000000 ) ) ;
#25728 = CARTESIAN_POINT ( 'NONE',  ( 0.9999999999999731326, -4.808326913196006913, -0.7999999999999951594 ) ) ;
#25729 = EDGE_CURVE ( 'NONE', #23216, #30129, #15890, .T. ) ;
#25730 = ORIENTED_EDGE ( 'NONE', *, *, #10772, .T. ) ;
#25731 = ADVANCED_FACE ( 'NONE', ( #30194 ), #5531, .T. ) ;
#25732 = AXIS2_PLACEMENT_3D ( 'NONE', #16501, #5016, #24446 ) ;
#25733 = DIRECTION ( 'NONE',  ( 0.000000000000000000, -6.938893903907228378E-15, 1.000000000000000000 ) ) ;
#25734 = ORIENTED_EDGE ( 'NONE', *, *, #32912, .F. ) ;
#25735 = CARTESIAN_POINT ( 'NONE',  ( -34.00000000000000000, -114.0592624029313242, 9.003524454178446490 ) ) ;
#25736 = CARTESIAN_POINT ( 'NONE',  ( 8.000000000000000000, 13.55483219355744673, -11.06713717293225407 ) ) ;
#25737 = CARTESIAN_POINT ( 'NONE',  ( -35.50000000000000711, -116.0140978167138712, -0.4997823525984418369 ) ) ;
#25738 = EDGE_LOOP ( 'NONE', ( #33747, #29287 ) ) ;
#25739 = ORIENTED_EDGE ( 'NONE', *, *, #20745, .F. ) ;
#25740 = LINE ( 'NONE', #8622, #16565 ) ;
#25741 = LINE ( 'NONE', #1071, #10602 ) ;
#25742 = VERTEX_POINT ( 'NONE', #2488 ) ;
#25743 = EDGE_CURVE ( 'NONE', #26843, #12757, #3246, .T. ) ;
#25744 = ORIENTED_EDGE ( 'NONE', *, *, #24840, .F. ) ;
#25745 = CIRCLE ( 'NONE', #10216, 8.000000000000000000 ) ;
#25746 = VECTOR ( 'NONE', #5697, 1000.000000000000000 ) ;
#25747 = DIRECTION ( 'NONE',  ( 0.000000000000000000, 0.000000000000000000, -1.000000000000000000 ) ) ;
#25748 = VERTEX_POINT ( 'NONE', #16490 ) ;
#25749 = CARTESIAN_POINT ( 'NONE',  ( -35.62769128460905677, -112.5438815906447729, 5.308975545821551734 ) ) ;
#25750 = VECTOR ( 'NONE', #2905, 1000.000000000000000 ) ;
#25751 = CYLINDRICAL_SURFACE ( 'NONE', #9267, 10.99999999999999645 ) ;
#25752 = ORIENTED_EDGE ( 'NONE', *, *, #11756, .F. ) ;
#25753 = ORIENTED_EDGE ( 'NONE', *, *, #12804, .T. ) ;
#25754 = CARTESIAN_POINT ( 'NONE',  ( -35.50000000000000000, -112.3697613878167658, -2.522673865603075605 ) ) ;
#25755 = AXIS2_PLACEMENT_3D ( 'NONE', #19213, #16686, #30736 ) ;
#25756 = DIRECTION ( 'NONE',  ( -1.000000000000000000, 0.000000000000000000, 0.000000000000000000 ) ) ;
#25757 = ORIENTED_EDGE ( 'NONE', *, *, #12507, .T. ) ;
#25758 = VECTOR ( 'NONE', #19339, 1000.000000000000000 ) ;
#25759 = CARTESIAN_POINT ( 'NONE',  ( -38.00000000000000711, -114.9929510916434339, 12.56351784598954779 ) ) ;
#25760 = EDGE_CURVE ( 'NONE', #26513, #17877, #27506, .T. ) ;
#25761 = CARTESIAN_POINT ( 'NONE',  ( -34.50000000000000000, -114.0185793162512908, 9.502217742515812304 ) ) ;
#25762 = CARTESIAN_POINT ( 'NONE',  ( -2.000000000000000888, -4.694161725993254197E-16, -6.765000000000044977 ) ) ;
#25763 = DIRECTION ( 'NONE',  ( 0.02857142857142376188, 0.9995917534020517525, 3.884870526907702485E-16 ) ) ;
#25764 = CARTESIAN_POINT ( 'NONE',  ( -35.51674767832922441, -113.9929510916434339, 14.04194344061634325 ) ) ;
#25765 = DIRECTION ( 'NONE',  ( -1.000000000000000000, 0.000000000000000000, 0.000000000000000000 ) ) ;
#25766 = CARTESIAN_POINT ( 'NONE',  ( -36.01562499999996447, -114.9929510916434339, 13.11852480586264669 ) ) ;
#25767 = VECTOR ( 'NONE', #9772, 1000.000000000000000 ) ;
#25768 = PRESENTATION_STYLE_ASSIGNMENT (( #17992 ) ) ;
#25769 = ORIENTED_EDGE ( 'NONE', *, *, #25939, .T. ) ;
#25770 = CYLINDRICAL_SURFACE ( 'NONE', #6063, 4.000000000000000000 ) ;
#25771 = CARTESIAN_POINT ( 'NONE',  ( 4.000000000000003553, -9.637487275701184686, 10.15474465512046542 ) ) ;
#25772 = ADVANCED_FACE ( 'NONE', ( #24794 ), #24967, .T. ) ;
#25773 = ORIENTED_EDGE ( 'NONE', *, *, #8047, .F. ) ;
#25774 = EDGE_CURVE ( 'NONE', #32593, #6961, #8978, .T. ) ;
#25775 = CARTESIAN_POINT ( 'NONE',  ( -35.50000000000000711, -114.9902084924877954, 10.43071793783961176 ) ) ;
#25776 = ORIENTED_EDGE ( 'NONE', *, *, #6649, .F. ) ;
#25777 = AXIS2_PLACEMENT_3D ( 'NONE', #34942, #24303, #27006 ) ;
#25778 = EDGE_CURVE ( 'NONE', #35547, #13527, #24267, .T. ) ;
#25779 = DIRECTION ( 'NONE',  ( 0.000000000000000000, -0.9510565162951500895, -0.3090169943749581649 ) ) ;
#25780 = CIRCLE ( 'NONE', #21156, 19.99999999999998579 ) ;
#25781 = ORIENTED_EDGE ( 'NONE', *, *, #435, .T. ) ;
#25782 = AXIS2_PLACEMENT_3D ( 'NONE', #26227, #29959, #1566 ) ;
#25783 = DIRECTION ( 'NONE',  ( -1.000000000000000000, 0.000000000000000000, 0.000000000000000000 ) ) ;
#25784 = ORIENTED_EDGE ( 'NONE', *, *, #28883, .T. ) ;
#25785 = CARTESIAN_POINT ( 'NONE',  ( -35.50000000000000000, -113.0140978167129617, -0.6247823525984270709 ) ) ;
#25786 = LINE ( 'NONE', #9022, #8690 ) ;
#25787 = CARTESIAN_POINT ( 'NONE',  ( -34.97545270896703329, -113.2308352781851539, 7.409774454178451819 ) ) ;
#25788 = EDGE_CURVE ( 'NONE', #11685, #34870, #32527, .T. ) ;
#25789 = VERTEX_POINT ( 'NONE', #14146 ) ;
#25790 = CIRCLE ( 'NONE', #2213, 17.49900000000002720 ) ;
#25791 = CARTESIAN_POINT ( 'NONE',  ( -39.02454729103295961, -114.7691647218148745, 2.159774454178448710 ) ) ;
#25792 = ADVANCED_FACE ( 'NONE', ( #28199 ), #33412, .T. ) ;
#25793 = CARTESIAN_POINT ( 'NONE',  ( 8.000000000000007105, 9.433698091065187086, -1.111908866155128628 ) ) ;
#25794 = CARTESIAN_POINT ( 'NONE',  ( -35.50000000000000711, -113.4307644833805000, -1.624782352598427959 ) ) ;
#25795 = VERTEX_POINT ( 'NONE', #34133 ) ;
#25796 = ORIENTED_EDGE ( 'NONE', *, *, #33326, .F. ) ;
#25797 = DIRECTION ( 'NONE',  ( 0.000000000000000000, 0.000000000000000000, 1.000000000000000000 ) ) ;
#25798 = DIRECTION ( 'NONE',  ( -1.000000000000000000, -0.000000000000000000, 0.000000000000000000 ) ) ;
#25799 = ORIENTED_EDGE ( 'NONE', *, *, #2527, .T. ) ;
#25800 = ORIENTED_EDGE ( 'NONE', *, *, #16705, .F. ) ;
#25801 = CARTESIAN_POINT ( 'NONE',  ( -34.50000000000000000, -116.0140978167138712, -0.4997823525984418369 ) ) ;
#25802 = DIRECTION ( 'NONE',  ( 0.000000000000000000, 0.000000000000000000, 1.000000000000000000 ) ) ;
#25803 = AXIS2_PLACEMENT_3D ( 'NONE', #18648, #19178, #21703 ) ;
#25804 = EDGE_LOOP ( 'NONE', ( #24309, #30418, #18866, #28804 ) ) ;
#25805 = ORIENTED_EDGE ( 'NONE', *, *, #16025, .F. ) ;
#25806 = CARTESIAN_POINT ( 'NONE',  ( 0.000000000000000000, -6.336799421339930127, 16.31134495048480915 ) ) ;
#25807 = EDGE_CURVE ( 'NONE', #29543, #19637, #6230, .T. ) ;
#25808 = AXIS2_PLACEMENT_3D ( 'NONE', #25619, #14080, #17132 ) ;
#25809 = CARTESIAN_POINT ( 'NONE',  ( -36.99999999999988631, -113.9929510916434339, 13.11852480586264846 ) ) ;
#25810 = EDGE_CURVE ( 'NONE', #31265, #27370, #17547, .T. ) ;
#25811 = CARTESIAN_POINT ( 'NONE',  ( -34.50000000000000000, -113.0796441757086939, 1.890140615870383956 ) ) ;
#25812 = ADVANCED_FACE ( 'NONE', ( #22958 ), #22778, .T. ) ;
#25813 = CARTESIAN_POINT ( 'NONE',  ( -35.50000000000000000, -113.9929510916434339, 10.59426868253284226 ) ) ;
#25814 = CARTESIAN_POINT ( 'NONE',  ( -35.50000000000000000, -115.9895221797699065, 10.38535157366622563 ) ) ;
#25815 = CARTESIAN_POINT ( 'NONE',  ( 8.000000000000000000, 0.000000000000000000, 0.000000000000000000 ) ) ;
#25816 = DIRECTION ( 'NONE',  ( -1.000000000000000000, 0.000000000000000000, 0.000000000000000000 ) ) ;
#25817 = EDGE_CURVE ( 'NONE', #21217, #3103, #8417, .T. ) ;
#25818 = ORIENTED_EDGE ( 'NONE', *, *, #30318, .F. ) ;
#25819 = EDGE_CURVE ( 'NONE', #8438, #35587, #19704, .T. ) ;
#25820 = CARTESIAN_POINT ( 'NONE',  ( 0.000000000000000000, -2.710505431213761085E-17, 55.00000000000000000 ) ) ;
#25821 = FACE_OUTER_BOUND ( 'NONE', #34610, .T. ) ;
#25822 = CARTESIAN_POINT ( 'NONE',  ( 0.000000000000000000, 0.000000000000000000, -32.00000000000000000 ) ) ;
#25823 = VERTEX_POINT ( 'NONE', #3901 ) ;
#25824 = CARTESIAN_POINT ( 'NONE',  ( 0.000000000000000000, -2.710505431213761085E-17, 29.09999999999999787 ) ) ;
#25825 = PLANE ( 'NONE',  #30267 ) ;
#25826 = PLANE ( 'NONE',  #17083 ) ;
#25827 = DIRECTION ( 'NONE',  ( -1.000000000000000000, 0.000000000000000000, 0.000000000000000000 ) ) ;
#25828 = CONTEXT_DEPENDENT_SHAPE_REPRESENTATION ( #14946, #6121 ) ;
#25829 = AXIS2_PLACEMENT_3D ( 'NONE', #11881, #19615, #22152 ) ;
#25830 = DIRECTION ( 'NONE',  ( -1.000000000000000000, 0.000000000000000000, -0.000000000000000000 ) ) ;
#25831 = CARTESIAN_POINT ( 'NONE',  ( 8.000000000000000000, 0.000000000000000000, 0.000000000000000000 ) ) ;
#25832 = EDGE_CURVE ( 'NONE', #5217, #27829, #7830, .T. ) ;
#25833 = ORIENTED_EDGE ( 'NONE', *, *, #9015, .T. ) ;
#25834 = AXIS2_PLACEMENT_3D ( 'NONE', #6875, #12645, #1475 ) ;
#25835 = DIRECTION ( 'NONE',  ( 0.000000000000000000, 0.000000000000000000, -1.000000000000000000 ) ) ;
#25836 = CARTESIAN_POINT ( 'NONE',  ( -34.50000000000000000, -117.0140978167138854, -0.1247823525984438492 ) ) ;
#25837 = DIRECTION ( 'NONE',  ( 1.000000000000000000, -0.000000000000000000, 0.000000000000000000 ) ) ;
#25838 = VERTEX_POINT ( 'NONE', #17015 ) ;
#25839 = ORIENTED_EDGE ( 'NONE', *, *, #9869, .T. ) ;
#25840 = CARTESIAN_POINT ( 'NONE',  ( -36.94073759706866156, -113.0000000000000000, 2.628524454178448710 ) ) ;
#25841 = ORIENTED_EDGE ( 'NONE', *, *, #2464, .T. ) ;
#25842 = ORIENTED_EDGE ( 'NONE', *, *, #14127, .F. ) ;
#25843 = EDGE_LOOP ( 'NONE', ( #2725, #2374, #2062, #17679 ) ) ;
#25844 = CARTESIAN_POINT ( 'NONE',  ( -34.50000000000000000, -113.0140978167134449, 0.8752176474011410523 ) ) ;
#25845 = CARTESIAN_POINT ( 'NONE',  ( -35.50000000000000711, -115.8878449012421754, -1.128496220799388494 ) ) ;
#25846 = ADVANCED_FACE ( 'NONE', ( #6571 ), #14857, .T. ) ;
#25847 = CARTESIAN_POINT ( 'NONE',  ( 0.000000000000000000, 0.000000000000000000, 0.000000000000000000 ) ) ;
#25848 = EDGE_CURVE ( 'NONE', #10144, #4193, #25323, .T. ) ;
#25849 = CARTESIAN_POINT ( 'NONE',  ( -35.50000000000000711, -114.9929510916434339, 12.59102132592610523 ) ) ;
#25850 = CARTESIAN_POINT ( 'NONE',  ( 7.999999999999992895, -43.83938735307282997, 18.28286404005782728 ) ) ;
#25851 = AXIS2_PLACEMENT_3D ( 'NONE', #280, #17001, #25666 ) ;
#25852 = CYLINDRICAL_SURFACE ( 'NONE', #7976, 4.000000000000000000 ) ;
#25853 = CARTESIAN_POINT ( 'NONE',  ( -34.50000000000000000, -114.9929510916434339, 12.17846912687782712 ) ) ;
#25854 = LINE ( 'NONE', #1899, #9943 ) ;
#25855 = CIRCLE ( 'NONE', #29865, 14.00000000000000000 ) ;
#25856 = EDGE_CURVE ( 'NONE', #26512, #5410, #15295, .T. ) ;
#25857 = CARTESIAN_POINT ( 'NONE',  ( 8.000000000000000000, 18.48663108841359559, -3.384281271887881637 ) ) ;
#25858 = ORIENTED_EDGE ( 'NONE', *, *, #1521, .F. ) ;
#25859 = CIRCLE ( 'NONE', #3431, 4.000000000000000000 ) ;
#25860 = CARTESIAN_POINT ( 'NONE',  ( -35.50000000000000000, -115.7766462221073454, 9.569741527169023598 ) ) ;
#25861 = CARTESIAN_POINT ( 'NONE',  ( -35.50000000000000711, -112.0140978167138712, 0.6252176474015680441 ) ) ;
#25862 = SURFACE_STYLE_FILL_AREA ( #19232 ) ;
#25863 = EDGE_CURVE ( 'NONE', #15928, #25438, #13041, .T. ) ;
#25864 = CIRCLE ( 'NONE', #15474, 47.49900000000001654 ) ;
#25865 = LINE ( 'NONE', #24833, #11788 ) ;
#25866 = CARTESIAN_POINT ( 'NONE',  ( 0.000000000000000000, 6.860320204751340079, -13.89802171851375689 ) ) ;
#25867 = DIRECTION ( 'NONE',  ( -1.000000000000000000, 0.000000000000000000, 0.000000000000000000 ) ) ;
#25868 = CYLINDRICAL_SURFACE ( 'NONE', #10083, 9.499000000000000554 ) ;
#25869 = CARTESIAN_POINT ( 'NONE',  ( -50.00000000000000000, 0.000000000000000000, 0.000000000000000000 ) ) ;
#25870 = CARTESIAN_POINT ( 'NONE',  ( 0.000000000000000000, 0.000000000000000000, 0.000000000000000000 ) ) ;
#25871 = EDGE_LOOP ( 'NONE', ( #7888, #10373, #31883, #19810 ) ) ;
#25872 = CARTESIAN_POINT ( 'NONE',  ( -36.25098837183130485, -114.6652019342044184, 7.183975545821551734 ) ) ;
#25873 = FACE_OUTER_BOUND ( 'NONE', #31895, .T. ) ;
#25874 = DIRECTION ( 'NONE',  ( 0.000000000000000000, 1.000000000000000000, 0.000000000000000000 ) ) ;
#25875 = ORIENTED_EDGE ( 'NONE', *, *, #16677, .F. ) ;
#25876 = ORIENTED_EDGE ( 'NONE', *, *, #9449, .T. ) ;
#25877 = DIRECTION ( 'NONE',  ( 1.000000000000000000, 0.000000000000000000, 0.000000000000000000 ) ) ;
#25878 = EDGE_LOOP ( 'NONE', ( #26036, #8473 ) ) ;
#25879 = CARTESIAN_POINT ( 'NONE',  ( -39.99999999999999289, -114.0592624029313242, 6.246475545821551734 ) ) ;
#25880 = VERTEX_POINT ( 'NONE', #19883 ) ;
#25881 = DIRECTION ( 'NONE',  ( 0.000000000000000000, 0.000000000000000000, -1.000000000000000000 ) ) ;
#25882 = CARTESIAN_POINT ( 'NONE',  ( 7.999999999999992895, -27.79676263918161894, -37.88001506494798321 ) ) ;
#25883 = CONICAL_SURFACE ( 'NONE', #28164, 4.980000000000017302, 0.5675376247847534472 ) ;
#25884 = PRODUCT_DEFINITION_FORMATION_WITH_SPECIFIED_SOURCE ( 'ANY', '', #31654, .NOT_KNOWN. ) ;
#25885 = AXIS2_PLACEMENT_3D ( 'NONE', #2698, #19529, #34934 ) ;
#25886 = SHAPE_DEFINITION_REPRESENTATION ( #7225, #13971 ) ;
#25887 = CARTESIAN_POINT ( 'NONE',  ( 7.999999999999992895, 43.55304910509447325, -28.41006711799937179 ) ) ;
#25888 = ORIENTED_EDGE ( 'NONE', *, *, #32911, .F. ) ;
#25889 = EDGE_LOOP ( 'NONE', ( #9785, #12677, #22144, #10026 ) ) ;
#25890 = ADVANCED_FACE ( 'NONE', ( #27845 ), #14668, .T. ) ;
#25891 = CARTESIAN_POINT ( 'NONE',  ( 70.00001200000004076, -27.02775365097033244, 81.10410929332667251 ) ) ;
#25892 = CARTESIAN_POINT ( 'NONE',  ( 7.999999999999992895, 0.000000000000000000, 0.000000000000000000 ) ) ;
#25893 = ORIENTED_EDGE ( 'NONE', *, *, #666, .F. ) ;
#25894 = CARTESIAN_POINT ( 'NONE',  ( -1.600000000000004086, -12.74999999999999822, -1.200000000000006617 ) ) ;
#25895 = CARTESIAN_POINT ( 'NONE',  ( -34.50000000000000000, -115.0140978167138712, 0.3752176474015737617 ) ) ;
#25896 = CARTESIAN_POINT ( 'NONE',  ( 1.519999999999994245, -4.846123502488801633E-16, -6.984000000000015085 ) ) ;
#25897 = FACE_OUTER_BOUND ( 'NONE', #32963, .T. ) ;
#25898 = CARTESIAN_POINT ( 'NONE',  ( -34.50000000000000000, -115.9895221797699065, 10.38535157366622563 ) ) ;
#25899 = CIRCLE ( 'NONE', #24740, 14.00000000000000000 ) ;
#25900 = FACE_OUTER_BOUND ( 'NONE', #5297, .T. ) ;
#25901 = FACE_OUTER_BOUND ( 'NONE', #31344, .T. ) ;
#25902 = CARTESIAN_POINT ( 'NONE',  ( -34.50000000000000000, -114.1185248058629611, 8.507048908356933836 ) ) ;
#25903 = CARTESIAN_POINT ( 'NONE',  ( -1.799999999999995604, 8.399942390771673342E-16, 4.000000000000000000 ) ) ;
#25904 = CARTESIAN_POINT ( 'NONE',  ( 0.000000000000000000, 46.87740477351717061, 16.82754413119462455 ) ) ;
#25905 = LINE ( 'NONE', #6802, #19858 ) ;
#25906 = DIRECTION ( 'NONE',  ( -1.000000000000000000, -0.000000000000000000, -0.000000000000000000 ) ) ;
#25907 = CARTESIAN_POINT ( 'NONE',  ( 0.000000000000000000, -44.61570720899105424, 14.73072383765550164 ) ) ;
#25908 = ORIENTED_EDGE ( 'NONE', *, *, #11207, .F. ) ;
#25909 = CIRCLE ( 'NONE', #10387, 20.00000000000000355 ) ;
#25910 = AXIS2_PLACEMENT_3D ( 'NONE', #16369, #33132, #6110 ) ;
#25911 = CARTESIAN_POINT ( 'NONE',  ( -36.94073759706868287, -116.9999999999999858, 2.871475545821551290 ) ) ;
#25912 = DIRECTION ( 'NONE',  ( -1.000000000000000000, -8.673617379884000959E-17, -1.502314598737161250E-16 ) ) ;
#25913 = CARTESIAN_POINT ( 'NONE',  ( -35.50000000000000000, -114.1185248058627053, 1.007048908356900085 ) ) ;
#25914 = EDGE_LOOP ( 'NONE', ( #839, #10896, #30651, #12140 ) ) ;
#25915 = ORIENTED_EDGE ( 'NONE', *, *, #33935, .T. ) ;
#25916 = PRODUCT_DEFINITION_SHAPE ( 'NONE', 'NONE',  #35636 ) ;
#25917 = CARTESIAN_POINT ( 'NONE',  ( 7.999999999999992895, 2.123073309835863842, -47.45152853935333326 ) ) ;
#25918 = ORIENTED_EDGE ( 'NONE', *, *, #16144, .F. ) ;
#25919 = ORIENTED_EDGE ( 'NONE', *, *, #30598, .T. ) ;
#25920 = CARTESIAN_POINT ( 'NONE',  ( 1.110223024625156540E-13, -1.000000000000042633, 45.00000000000000711 ) ) ;
#25921 = CARTESIAN_POINT ( 'NONE',  ( -35.54388159064475872, -115.3723087153909432, 5.683975545821551734 ) ) ;
#25922 = AXIS2_PLACEMENT_3D ( 'NONE', #6086, #22625, #23176 ) ;
#25923 = DIRECTION ( 'NONE',  ( -1.000000000000000000, 0.000000000000000000, 0.000000000000000000 ) ) ;
#25924 = DIRECTION ( 'NONE',  ( 1.000000000000000000, -0.000000000000000000, -0.000000000000000000 ) ) ;
#25925 = ORIENTED_EDGE ( 'NONE', *, *, #5536, .T. ) ;
#25926 = ORIENTED_EDGE ( 'NONE', *, *, #8200, .F. ) ;
#25927 = CARTESIAN_POINT ( 'NONE',  ( -35.50000000000000000, -114.3474311500471572, -2.624782352598442614 ) ) ;
#25928 = EDGE_CURVE ( 'NONE', #25030, #16010, #25109, .T. ) ;
#25929 = LINE ( 'NONE', #23215, #29303 ) ;
#25930 = AXIS2_PLACEMENT_3D ( 'NONE', #18765, #29769, #13378 ) ;
#25931 =( GEOMETRIC_REPRESENTATION_CONTEXT ( 3 ) GLOBAL_UNCERTAINTY_ASSIGNED_CONTEXT ( ( #22196 ) ) GLOBAL_UNIT_ASSIGNED_CONTEXT ( ( #10200, #24244, #10914 ) ) REPRESENTATION_CONTEXT ( 'NONE', 'WORKASPACE' ) );
#25932 = ORIENTED_EDGE ( 'NONE', *, *, #1360, .T. ) ;
#25933 = VECTOR ( 'NONE', #13525, 1000.000000000000000 ) ;
#25934 = CARTESIAN_POINT ( 'NONE',  ( -37.99899697755054717, -114.9929510916434339, 12.65121853911336736 ) ) ;
#25935 = AXIS2_PLACEMENT_3D ( 'NONE', #22274, #27699, #24988 ) ;
#25936 = CARTESIAN_POINT ( 'NONE',  ( -38.42182118622945808, -113.9929510916434339, 13.81802396319329773 ) ) ;
#25937 = CARTESIAN_POINT ( 'NONE',  ( 8.000000000000000000, 6.860320204751148232, 13.89802171851385459 ) ) ;
#25938 = DIRECTION ( 'NONE',  ( -1.000000000000000000, -0.000000000000000000, 0.000000000000000000 ) ) ;
#25939 = EDGE_CURVE ( 'NONE', #16008, #3725, #30283, .T. ) ;
#25940 = CARTESIAN_POINT ( 'NONE',  ( -38.99699093265172678, -113.9929510916434339, 12.71660600561481402 ) ) ;
#25941 = FACE_OUTER_BOUND ( 'NONE', #9911, .T. ) ;
#25942 = CARTESIAN_POINT ( 'NONE',  ( -35.50100302244946704, -114.9929510916434339, 12.65121853911337269 ) ) ;
#25943 = ORIENTED_EDGE ( 'NONE', *, *, #20853, .F. ) ;
#25944 = CARTESIAN_POINT ( 'NONE',  ( 7.999999999999992895, 47.22458491092828581, -5.098390039073752433 ) ) ;
#25945 = FACE_OUTER_BOUND ( 'NONE', #303, .T. ) ;
#25946 = ORIENTED_EDGE ( 'NONE', *, *, #17320, .F. ) ;
#25947 = CARTESIAN_POINT ( 'NONE',  ( -35.51597953369718397, -114.9929510916434339, 12.74811950270164473 ) ) ;
#25948 = ORIENTED_EDGE ( 'NONE', *, *, #14161, .T. ) ;
#25949 = CARTESIAN_POINT ( 'NONE',  ( -38.99999999999999289, -113.9407375970686900, 3.753524454178449155 ) ) ;
#25950 = VERTEX_POINT ( 'NONE', #9284 ) ;
#25951 = DIRECTION ( 'NONE',  ( 1.000000000000000000, 0.000000000000000000, 0.000000000000000000 ) ) ;
#25952 = ORIENTED_EDGE ( 'NONE', *, *, #31040, .T. ) ;
#25953 = CARTESIAN_POINT ( 'NONE',  ( -34.50000000000000000, -113.0140978167142833, 0.8752176474015604946 ) ) ;
#25954 = CARTESIAN_POINT ( 'NONE',  ( -3.799999999999999822, -2.710505431213761085E-17, 45.89999999999999858 ) ) ;
#25955 = CARTESIAN_POINT ( 'NONE',  ( -36.11231047232249125, -112.0245472910329880, 7.222274454178451819 ) ) ;
#25956 = CIRCLE ( 'NONE', #31112, 7.200000000000006395 ) ;
#25957 = ORIENTED_EDGE ( 'NONE', *, *, #19016, .T. ) ;
#25958 = CARTESIAN_POINT ( 'NONE',  ( -35.02454729103298803, -114.8876895276775087, 6.097274454178449155 ) ) ;
#25959 = EDGE_CURVE ( 'NONE', #27460, #13434, #31250, .T. ) ;
#25960 = APPLICATION_CONTEXT ( 'automotive_design' ) ;
#25961 = CARTESIAN_POINT ( 'NONE',  ( 4.000000000000003553, -19.35373470438990395, 10.46102064772334295 ) ) ;
#25962 = CARTESIAN_POINT ( 'NONE',  ( -35.50000000000000711, -112.8835768857893527, -1.616767172155725740 ) ) ;
#25963 = ORIENTED_EDGE ( 'NONE', *, *, #28431, .T. ) ;
#25964 = VERTEX_POINT ( 'NONE', #16841 ) ;
#25965 = CARTESIAN_POINT ( 'NONE',  ( -46.00000000000000000, 1.347111479062090574E-15, 59.00000000000000000 ) ) ;
#25966 = CARTESIAN_POINT ( 'NONE',  ( -0.2142857142857362840, -10.49781318335649161, -1.200000000000006617 ) ) ;
#25967 = ORIENTED_EDGE ( 'NONE', *, *, #759, .F. ) ;
#25968 = ORIENTED_EDGE ( 'NONE', *, *, #34379, .T. ) ;
#25969 = CARTESIAN_POINT ( 'NONE',  ( -34.50000000000000000, -112.8920926830253677, 2.874852253704053062 ) ) ;
#25970 = DIRECTION ( 'NONE',  ( -1.000000000000000000, 0.000000000000000000, 0.000000000000000000 ) ) ;
#25971 = EDGE_CURVE ( 'NONE', #29518, #9746, #14145, .T. ) ;
#25972 = ADVANCED_FACE ( 'NONE', ( #15376 ), #12336, .F. ) ;
#25973 = EDGE_CURVE ( 'NONE', #18506, #14392, #22777, .T. ) ;
#25974 = ORIENTED_EDGE ( 'NONE', *, *, #27407, .F. ) ;
#25975 = ORIENTED_EDGE ( 'NONE', *, *, #28159, .T. ) ;
#25976 = DIRECTION ( 'NONE',  ( -1.000000000000000000, -0.000000000000000000, -0.000000000000000000 ) ) ;
#25977 = CARTESIAN_POINT ( 'NONE',  ( -37.98402046630260287, -113.9929510916434339, 12.74811950270164296 ) ) ;
#25978 = CARTESIAN_POINT ( 'NONE',  ( 8.000000000000000000, 0.000000000000000000, 0.000000000000000000 ) ) ;
#25979 = EDGE_CURVE ( 'NONE', #25748, #34245, #18780, .T. ) ;
#25980 = CIRCLE ( 'NONE', #34023, 1.000000000000000444 ) ;
#25981 = VECTOR ( 'NONE', #13829, 1000.000000000000000 ) ;
#25982 = CARTESIAN_POINT ( 'NONE',  ( -35.50000000000000000, -113.9929510916434339, 12.56351784598954424 ) ) ;
#25983 = ADVANCED_FACE ( 'NONE', ( #31779 ), #28735, .T. ) ;
#25984 = CARTESIAN_POINT ( 'NONE',  ( -35.49999931242378182, -115.9929510916434481, 12.61439929482945743 ) ) ;
#25985 = DIRECTION ( 'NONE',  ( -1.000000000000000000, 0.000000000000000000, 0.000000000000000000 ) ) ;
#25986 = DIRECTION ( 'NONE',  ( 1.000000000000000000, 0.000000000000000000, 0.000000000000000000 ) ) ;
#25987 = LINE ( 'NONE', #17866, #25767 ) ;
#25988 = DIRECTION ( 'NONE',  ( 1.000000000000000000, -0.000000000000000000, -0.000000000000000000 ) ) ;
#25989 = CARTESIAN_POINT ( 'NONE',  ( -34.49999999999998579, -30.19486372867095980, 84.29903810567654432 ) ) ;
#25990 = ORIENTED_EDGE ( 'NONE', *, *, #25441, .T. ) ;
#25991 = PRESENTATION_LAYER_ASSIGNMENT (  '', '', ( #3582 ) ) ;
#25992 = CARTESIAN_POINT ( 'NONE',  ( 0.000000000000000000, 0.000000000000000000, 0.000000000000000000 ) ) ;
#25993 = CARTESIAN_POINT ( 'NONE',  ( -35.50000000000000711, -112.8356783780338759, 1.859636627348750348 ) ) ;
#25994 = FACE_OUTER_BOUND ( 'NONE', #35326, .T. ) ;
#25995 = LINE ( 'NONE', #15701, #3238 ) ;
#25996 = DIRECTION ( 'NONE',  ( -1.000000000000000000, 0.000000000000000000, 0.000000000000000000 ) ) ;
#25997 = EDGE_CURVE ( 'NONE', #19518, #26450, #28908, .T. ) ;
#25998 = VERTEX_POINT ( 'NONE', #4257 ) ;
#25999 = DIRECTION ( 'NONE',  ( -1.000000000000000000, 0.000000000000000000, 0.000000000000000000 ) ) ;
#26000 = CARTESIAN_POINT ( 'NONE',  ( -34.50000000000000000, -114.6807644833805000, -2.624782352598442614 ) ) ;
#26001 = EDGE_CURVE ( 'NONE', #21432, #4018, #15028, .T. ) ;
#26002 = CARTESIAN_POINT ( 'NONE',  ( 0.000000000000000000, 15.92965478239619515, 15.17386234660388844 ) ) ;
#26003 = ORIENTED_EDGE ( 'NONE', *, *, #27880, .F. ) ;
#26004 = ORIENTED_EDGE ( 'NONE', *, *, #22729, .F. ) ;
#26005 = CARTESIAN_POINT ( 'NONE',  ( -38.02454729103296671, -114.3549511594417396, 2.159774454178448710 ) ) ;
#26006 = ORIENTED_EDGE ( 'NONE', *, *, #9269, .F. ) ;
#26007 = CIRCLE ( 'NONE', #31163, 3.799999999999999822 ) ;
#26008 = SURFACE_SIDE_STYLE ('',( #9970 ) ) ;
#26009 = ORIENTED_EDGE ( 'NONE', *, *, #16337, .T. ) ;
#26010 = ORIENTED_EDGE ( 'NONE', *, *, #22168, .T. ) ;
#26011 = CARTESIAN_POINT ( 'NONE',  ( -34.50000000000000000, -113.0140978167139991, 0.8752176474014555785 ) ) ;
#26012 =( REPRESENTATION_RELATIONSHIP ('NONE','NONE', #26607, #7982 ) REPRESENTATION_RELATIONSHIP_WITH_TRANSFORMATION ( #16454 )SHAPE_REPRESENTATION_RELATIONSHIP( ) );
#26013 = EDGE_CURVE ( 'NONE', #11969, #34614, #27438, .T. ) ;
#26014 = ADVANCED_FACE ( 'NONE', ( #12524 ), #23502, .T. ) ;
#26015 = EDGE_CURVE ( 'NONE', #30768, #13700, #26391, .T. ) ;
#26016 = DIRECTION ( 'NONE',  ( 3.154042683594196600E-16, -1.000000000000000000, 0.000000000000000000 ) ) ;
#26017 = CARTESIAN_POINT ( 'NONE',  ( 4.000000000000003553, -51.19683565102450729, 9.104066087303298360 ) ) ;
#26018 = AXIS2_PLACEMENT_3D ( 'NONE', #30507, #9239, #22733 ) ;
#26019 = CARTESIAN_POINT ( 'NONE',  ( -35.50000000000000711, -114.9929510916434339, 11.38636890470581164 ) ) ;
#26020 = LINE ( 'NONE', #9983, #9202 ) ;
#26021 = DIRECTION ( 'NONE',  ( -1.000000000000000000, -0.000000000000000000, -0.000000000000000000 ) ) ;
#26022 = EDGE_CURVE ( 'NONE', #7932, #3037, #4436, .T. ) ;
#26023 = CARTESIAN_POINT ( 'NONE',  ( -37.49023442168701337, -114.9929510916434339, 14.11852773550420359 ) ) ;
#26024 = CARTESIAN_POINT ( 'NONE',  ( 0.000000000000000000, -18.48663108841361336, 3.384281271887747078 ) ) ;
#26025 = CARTESIAN_POINT ( 'NONE',  ( 7.999999999999992895, -2.123073309834833111, -47.45152853935339010 ) ) ;
#26026 = ORIENTED_EDGE ( 'NONE', *, *, #22301, .F. ) ;
#26027 = CARTESIAN_POINT ( 'NONE',  ( -39.00000000000000000, -115.9929510916434481, 12.17846912687782179 ) ) ;
#26029 = CARTESIAN_POINT ( 'NONE',  ( -35.50000000000000711, -114.6807644833805000, -1.624782352598427959 ) ) ;
#26028 = AXIS2_PLACEMENT_3D ( 'NONE', #26735, #21302, #32470 ) ;
#26030 = CARTESIAN_POINT ( 'NONE',  ( 0.2142857142857085284, -10.49781318335649161, -1.200000000000006617 ) ) ;
#26031 = CARTESIAN_POINT ( 'NONE',  ( 0.000000000000000000, 44.25018368420744252, 27.31155879685197263 ) ) ;
#26032 = FACE_OUTER_BOUND ( 'NONE', #3874, .T. ) ;
#26033 = CARTESIAN_POINT ( 'NONE',  ( 0.000000000000000000, 6.336799421339804894, 16.31134495048487310 ) ) ;
#26034 = LINE ( 'NONE', #31431, #13060 ) ;
#26035 = CARTESIAN_POINT ( 'NONE',  ( 0.000000000000000000, 0.000000000000000000, 55.00000000000000000 ) ) ;
#26036 = ORIENTED_EDGE ( 'NONE', *, *, #35166, .T. ) ;
#26037 = CARTESIAN_POINT ( 'NONE',  ( -37.99999999999998579, -114.0592624029313242, 7.746475545821553510 ) ) ;
#26038 = CARTESIAN_POINT ( 'NONE',  ( 4.000000000000003553, 3.268936481846174136, 13.61301047812919762 ) ) ;
#26039 = DIRECTION ( 'NONE',  ( -1.000000000000000000, 0.000000000000000000, 0.000000000000000000 ) ) ;
#26040 = EDGE_CURVE ( 'NONE', #4109, #8056, #23383, .T. ) ;
#26041 = EDGE_LOOP ( 'NONE', ( #16106, #22093, #29676, #1679 ) ) ;
#26042 = AXIS2_PLACEMENT_3D ( 'NONE', #15512, #23462, #18043 ) ;
#26043 = ORIENTED_EDGE ( 'NONE', *, *, #24467, .T. ) ;
#26044 = CIRCLE ( 'NONE', #19138, 10.99999999999999467 ) ;
#26045 = CARTESIAN_POINT ( 'NONE',  ( 8.000000000000000000, 13.55483219355729396, 11.06713717293245658 ) ) ;
#26046 = EDGE_CURVE ( 'NONE', #19601, #13102, #8451, .T. ) ;
#26047 = LINE ( 'NONE', #28567, #31897 ) ;
#26048 = ORIENTED_EDGE ( 'NONE', *, *, #17774, .T. ) ;
#26049 = CARTESIAN_POINT ( 'NONE',  ( -40.02454729103296671, -112.8166217158120332, 7.840225545821554398 ) ) ;
#26050 = EDGE_LOOP ( 'NONE', ( #12234, #1938, #13751, #32167 ) ) ;
#26051 = FACE_OUTER_BOUND ( 'NONE', #15642, .T. ) ;
#26052 = AXIS2_PLACEMENT_3D ( 'NONE', #5669, #5146, #16086 ) ;
#26053 = VECTOR ( 'NONE', #15101, 1000.000000000000000 ) ;
#26054 = DIRECTION ( 'NONE',  ( 0.000000000000000000, 1.000000000000000000, -1.067522139062650474E-15 ) ) ;
#26055 = EDGE_CURVE ( 'NONE', #8765, #11436, #15554, .T. ) ;
#26056 = AXIS2_PLACEMENT_3D ( 'NONE', #16461, #33561, #22394 ) ;
#26057 = ADVANCED_FACE ( 'NONE', ( #26032 ), #1542, .T. ) ;
#26058 = DIRECTION ( 'NONE',  ( 0.000000000000000000, 0.5000000000000092149, -0.8660254037844333785 ) ) ;
#26059 = VERTEX_POINT ( 'NONE', #29088 ) ;
#26060 = ORIENTED_EDGE ( 'NONE', *, *, #15180, .F. ) ;
#26061 = CARTESIAN_POINT ( 'NONE',  ( 39.30000000000000426, -10.49999999999999112, 0.000000000000000000 ) ) ;
#26062 = FACE_OUTER_BOUND ( 'NONE', #32067, .T. ) ;
#26063 = ORIENTED_EDGE ( 'NONE', *, *, #11721, .F. ) ;
#26064 = DIRECTION ( 'NONE',  ( 0.000000000000000000, 0.000000000000000000, 1.000000000000000000 ) ) ;
#26065 = AXIS2_PLACEMENT_3D ( 'NONE', #3039, #14001, #24994 ) ;
#26066 = CARTESIAN_POINT ( 'NONE',  ( -34.50000000000000000, -112.0577668799241309, 1.173706424699810569 ) ) ;
#26067 = FACE_OUTER_BOUND ( 'NONE', #5339, .T. ) ;
#26068 = CARTESIAN_POINT ( 'NONE',  ( 0.000000000000000000, -2.710505431213761085E-17, 45.89999999999999858 ) ) ;
#26069 = AXIS2_PLACEMENT_3D ( 'NONE', #2435, #7993, #24745 ) ;
#26070 = CARTESIAN_POINT ( 'NONE',  ( -37.42187499999996447, -115.9929510916434481, 14.11852480586265024 ) ) ;
#26071 = CYLINDRICAL_SURFACE ( 'NONE', #28968, 4.872650870659778199 ) ;
#26072 = CARTESIAN_POINT ( 'NONE',  ( 0.000000000000000000, -47.32430374665948136, 21.55018039121510398 ) ) ;
#26073 = CARTESIAN_POINT ( 'NONE',  ( -39.00000000000000711, -114.9929510916434339, 12.53051367006571937 ) ) ;
#26074 = CARTESIAN_POINT ( 'NONE',  ( 0.000000000000000000, 0.000000000000000000, 0.000000000000000000 ) ) ;
#26075 = CARTESIAN_POINT ( 'NONE',  ( 30.00000000000000000, 11.00000000000000711, 0.000000000000000000 ) ) ;
#26076 = CARTESIAN_POINT ( 'NONE',  ( 50.00005079999998969, 4.898587196589412829E-16, -4.000000000000000000 ) ) ;
#26077 = DIRECTION ( 'NONE',  ( 0.000000000000000000, 0.000000000000000000, -1.000000000000000000 ) ) ;
#26078 = CIRCLE ( 'NONE', #27242, 4.800000000000001599 ) ;
#26079 = CIRCLE ( 'NONE', #23761, 8.000000000000007105 ) ;
#26080 = CARTESIAN_POINT ( 'NONE',  ( 0.000000000000000000, 0.000000000000000000, -40.00000000000000000 ) ) ;
#26081 = VERTEX_POINT ( 'NONE', #1723 ) ;
#26082 = CARTESIAN_POINT ( 'NONE',  ( -34.02454729103297382, -112.6980969099494132, 5.402725545821552622 ) ) ;
#26083 = CARTESIAN_POINT ( 'NONE',  ( 0.000000000000000000, -9.433698091065103597, 1.111908866155073117 ) ) ;
#26084 = CARTESIAN_POINT ( 'NONE',  ( -35.50000000000000000, -113.0140978167129617, -0.6247823525984270709 ) ) ;
#26085 = EDGE_CURVE ( 'NONE', #6113, #29440, #18268, .T. ) ;
#26086 = ORIENTED_EDGE ( 'NONE', *, *, #7055, .F. ) ;
#26087 = ORIENTED_EDGE ( 'NONE', *, *, #5305, .T. ) ;
#26088 = EDGE_CURVE ( 'NONE', #29062, #1635, #4620, .T. ) ;
#26089 = CYLINDRICAL_SURFACE ( 'NONE', #33820, 3.800000000000018918 ) ;
#26090 = CYLINDRICAL_SURFACE ( 'NONE', #11742, 4.800000000000000711 ) ;
#26091 = ORIENTED_EDGE ( 'NONE', *, *, #21998, .T. ) ;
#26092 = ORIENTED_EDGE ( 'NONE', *, *, #20173, .F. ) ;
#26093 = ORIENTED_EDGE ( 'NONE', *, *, #16752, .F. ) ;
#26094 = CIRCLE ( 'NONE', #22048, 52.00000000000000711 ) ;
#26095 = DIRECTION ( 'NONE',  ( 0.000000000000000000, -0.9822872507286865007, -0.1873813145857355644 ) ) ;
#26096 = CARTESIAN_POINT ( 'NONE',  ( -38.45611840935523418, -112.6276912846090568, 6.433975545821550845 ) ) ;
#26097 = CARTESIAN_POINT ( 'NONE',  ( -22.00000000000001066, -25.98076211353320630, 84.99999999999994316 ) ) ;
#26098 = CARTESIAN_POINT ( 'NONE',  ( 4.000000000000003553, -10.15474465512046542, 9.637487275701101197 ) ) ;
#26099 = ORIENTED_EDGE ( 'NONE', *, *, #5616, .F. ) ;
#26100 = VERTEX_POINT ( 'NONE', #10180 ) ;
#26101 = CARTESIAN_POINT ( 'NONE',  ( -35.50000000000000000, -113.8474311500459777, -2.624782352598442614 ) ) ;
#26102 = CIRCLE ( 'NONE', #2553, 47.49900000000000944 ) ;
#26103 = CIRCLE ( 'NONE', #18040, 9.999999999999994671 ) ;
#26104 = CARTESIAN_POINT ( 'NONE',  ( 0.000000000000000000, 1.111908866155100650, 9.433698091065117808 ) ) ;
#26105 = CARTESIAN_POINT ( 'NONE',  ( 0.000000000000000000, -6.359167119270593638, 18.96209359615092183 ) ) ;
#26106 = VERTEX_POINT ( 'NONE', #15734 ) ;
#26107 = CARTESIAN_POINT ( 'NONE',  ( -38.00000000000000711, -114.9929510916434339, 12.59652202191340820 ) ) ;
#26108 = CARTESIAN_POINT ( 'NONE',  ( -34.50000000000000000, -114.9929510916434339, 10.72628538622835670 ) ) ;
#26109 = CARTESIAN_POINT ( 'NONE',  ( 8.000000000000000000, 0.000000000000000000, 0.000000000000000000 ) ) ;
#26110 = CARTESIAN_POINT ( 'NONE',  ( -35.95915003344517658, -114.9929510916434339, 13.11692036158763308 ) ) ;
#26111 = DIRECTION ( 'NONE',  ( -1.000000000000000000, 0.000000000000000000, 0.000000000000000000 ) ) ;
#26112 = CARTESIAN_POINT ( 'NONE',  ( -35.93867112612154102, -113.9929510916434339, 14.11732072679899197 ) ) ;
#26113 = CARTESIAN_POINT ( 'NONE',  ( -34.49999999999998579, -29.98076211353323473, 83.49999999999990052 ) ) ;
#26114 = CARTESIAN_POINT ( 'NONE',  ( -35.50400759022159036, -114.9929510916434339, 12.68378527132497524 ) ) ;
#26115 = CYLINDRICAL_SURFACE ( 'NONE', #28571, 17.49900000000000233 ) ;
#26116 = ORIENTED_EDGE ( 'NONE', *, *, #21518, .T. ) ;
#26117 = DIRECTION ( 'NONE',  ( 0.000000000000000000, 0.000000000000000000, 1.000000000000000000 ) ) ;
#26118 = CARTESIAN_POINT ( 'NONE',  ( 7.999999999999992895, 22.82995208772687334, 41.06517797613670950 ) ) ;
#26119 = ORIENTED_EDGE ( 'NONE', *, *, #17774, .F. ) ;
#26120 = CARTESIAN_POINT ( 'NONE',  ( -35.50400759022159036, -114.9929510916434339, 12.68378527132497524 ) ) ;
#26121 = ORIENTED_EDGE ( 'NONE', *, *, #31500, .T. ) ;
#26122 = CARTESIAN_POINT ( 'NONE',  ( -38.45611840935523418, -115.3723087153909432, 2.066024454178448710 ) ) ;
#26123 = ORIENTED_EDGE ( 'NONE', *, *, #18519, .F. ) ;
#26124 = CARTESIAN_POINT ( 'NONE',  ( 8.000000000000007105, 0.000000000000000000, 0.000000000000000000 ) ) ;
#26125 = ORIENTED_EDGE ( 'NONE', *, *, #19446, .F. ) ;
#26126 = AXIS2_PLACEMENT_3D ( 'NONE', #15973, #16146, #27162 ) ;
#26127 = EDGE_CURVE ( 'NONE', #5642, #21593, #32141, .T. ) ;
#26128 = CIRCLE ( 'NONE', #23237, 8.000000000000008882 ) ;
#26129 = CARTESIAN_POINT ( 'NONE',  ( -34.50000000000000000, -113.0140978167138712, -0.3122823525984338988 ) ) ;
#26130 = DIRECTION ( 'NONE',  ( -1.000000000000000000, 0.000000000000000000, 0.000000000000000000 ) ) ;
#26131 = DIRECTION ( 'NONE',  ( 0.000000000000000000, 0.000000000000000000, 1.000000000000000000 ) ) ;
#26132 = EDGE_LOOP ( 'NONE', ( #26985, #6296 ) ) ;
#26133 = CARTESIAN_POINT ( 'NONE',  ( -39.02454729103295961, -114.7691647218148745, 6.659774454178450043 ) ) ;
#26134 = CYLINDRICAL_SURFACE ( 'NONE', #29745, 19.99999999999998579 ) ;
#26135 = CARTESIAN_POINT ( 'NONE',  ( -35.50000000000000711, -113.3474311500483935, -1.624782352598427959 ) ) ;
#26136 = EDGE_LOOP ( 'NONE', ( #20909, #31010, #34475, #29672 ) ) ;
#26137 = VERTEX_POINT ( 'NONE', #33033 ) ;
#26138 = LINE ( 'NONE', #20710, #4487 ) ;
#26139 = EDGE_CURVE ( 'NONE', #31396, #5642, #12465, .T. ) ;
#26140 = CARTESIAN_POINT ( 'NONE',  ( -55.00000000000000000, 6.123233995736780087E-16, 5.000000000000011546 ) ) ;
#26141 = ORIENTED_EDGE ( 'NONE', *, *, #7009, .F. ) ;
#26142 = ORIENTED_EDGE ( 'NONE', *, *, #35166, .F. ) ;
#26143 = CARTESIAN_POINT ( 'NONE',  ( -34.50000000000000000, -113.2224311500466030, -1.624782352598427959 ) ) ;
#26144 = CARTESIAN_POINT ( 'NONE',  ( -35.50000000000000711, -112.0209493036498287, 0.9959249592223760050 ) ) ;
#26145 = DIRECTION ( 'NONE',  ( 1.783119874454246424E-31, 1.187911941725854497E-31, -1.000000000000000000 ) ) ;
#26146 = VERTEX_POINT ( 'NONE', #29984 ) ;
#26147 = VERTEX_POINT ( 'NONE', #2813 ) ;
#26148 = DIRECTION ( 'NONE',  ( 0.000000000000000000, 0.9848077530122092416, -0.1736481776669233923 ) ) ;
#26149 = CARTESIAN_POINT ( 'NONE',  ( -37.56526046546249376, -113.9929510916434339, 13.11451721564129258 ) ) ;
#26150 = AXIS2_PLACEMENT_3D ( 'NONE', #9854, #29136, #4489 ) ;
#26151 = DIRECTION ( 'NONE',  ( -1.000000000000000000, -0.000000000000000000, -0.000000000000000000 ) ) ;
#26152 = CARTESIAN_POINT ( 'NONE',  ( -35.50000102263781798, -113.9929510916434339, 12.62466071271731494 ) ) ;
#26153 = AXIS2_PLACEMENT_3D ( 'NONE', #7732, #10628, #18716 ) ;
#26154 = CARTESIAN_POINT ( 'NONE',  ( -35.50000000000000000, -115.9929081983957104, 10.49113315946066294 ) ) ;
#26155 = CARTESIAN_POINT ( 'NONE',  ( 0.000000000000000000, 0.000000000000000000, -52.50000000000000000 ) ) ;
#26156 = DIRECTION ( 'NONE',  ( 0.000000000000000000, 0.000000000000000000, 1.000000000000000000 ) ) ;
#26157 = ORIENTED_EDGE ( 'NONE', *, *, #34299, .T. ) ;
#26158 = DIRECTION ( 'NONE',  ( -1.000000000000000000, 0.000000000000000000, 0.000000000000000000 ) ) ;
#26159 = CARTESIAN_POINT ( 'NONE',  ( 0.000000000000000000, 0.000000000000000000, -52.50000000000000000 ) ) ;
#26160 = CARTESIAN_POINT ( 'NONE',  ( 4.000000000000003553, 24.47917365150010127, -45.87777302070911389 ) ) ;
#26161 = AXIS2_PLACEMENT_3D ( 'NONE', #21621, #15686, #26704 ) ;
#26162 = ORIENTED_EDGE ( 'NONE', *, *, #11007, .T. ) ;
#26163 = DIRECTION ( 'NONE',  ( 0.000000000000000000, 0.000000000000000000, -1.000000000000000000 ) ) ;
#26164 = EDGE_CURVE ( 'NONE', #24623, #24853, #9005, .T. ) ;
#26165 = CARTESIAN_POINT ( 'NONE',  ( -35.50000000000000711, -114.1807644833817648, -1.624782352598427959 ) ) ;
#26166 = DIRECTION ( 'NONE',  ( 1.000000000000000000, -0.000000000000000000, -0.000000000000000000 ) ) ;
#26167 = EDGE_CURVE ( 'NONE', #29381, #29599, #84, .T. ) ;
#26168 = CONTEXT_DEPENDENT_SHAPE_REPRESENTATION ( #28532, #2677 ) ;
#26169 = CARTESIAN_POINT ( 'NONE',  ( -34.50000000000001421, -35.77980021920998155, 98.97243186433534845 ) ) ;
#26170 = DIRECTION ( 'NONE',  ( -1.000000000000000000, 0.000000000000000000, 0.000000000000000000 ) ) ;
#26171 = ORIENTED_EDGE ( 'NONE', *, *, #26827, .F. ) ;
#26172 = AXIS2_PLACEMENT_3D ( 'NONE', #15551, #32137, #6935 ) ;
#26173 = CARTESIAN_POINT ( 'NONE',  ( -0.1717365941144438635, -6.008326913195953800, 0.000000000000000000 ) ) ;
#26174 = CIRCLE ( 'NONE', #14082, 52.00000000000000711 ) ;
#26175 = CARTESIAN_POINT ( 'NONE',  ( -34.50000000000000000, -111.0141141789186605, -0.6738694770610589302 ) ) ;
#26176 = DIRECTION ( 'NONE',  ( -1.000000000000000000, -0.000000000000000000, 0.000000000000000000 ) ) ;
#26177 = ORIENTED_EDGE ( 'NONE', *, *, #16677, .T. ) ;
#26178 = ORIENTED_EDGE ( 'NONE', *, *, #27997, .F. ) ;
#26179 = CARTESIAN_POINT ( 'NONE',  ( -37.66520193420439711, -114.7490116281687023, 9.058975545821549957 ) ) ;
#26180 = EDGE_CURVE ( 'NONE', #29210, #31461, #35213, .T. ) ;
#26181 = SURFACE_SIDE_STYLE ('',( #1165 ) ) ;
#26182 = VERTEX_POINT ( 'NONE', #13249 ) ;
#26183 = ORIENTED_EDGE ( 'NONE', *, *, #29239, .T. ) ;
#26184 = CARTESIAN_POINT ( 'NONE',  ( -35.50000000000000000, -114.1807644833817648, -0.6247823525984269599 ) ) ;
#26185 = CIRCLE ( 'NONE', #10664, 20.00000000000000711 ) ;
#26186 = PLANE ( 'NONE',  #25233 ) ;
#26187 = CARTESIAN_POINT ( 'NONE',  ( -38.50000000000000711, -114.9929510916434339, 10.50625754673587231 ) ) ;
#26188 = AXIS2_PLACEMENT_3D ( 'NONE', #28459, #30800, #6664 ) ;
#26189 = CARTESIAN_POINT ( 'NONE',  ( -35.91854304697313438, -114.9929510916434339, 13.11211614918345703 ) ) ;
#26190 = DIRECTION ( 'NONE',  ( 1.000000000000000000, -5.339440136655842133E-16, -1.047965281155519420E-16 ) ) ;
#26191 = ADVANCED_FACE ( 'NONE', ( #24222 ), #16450, .F. ) ;
#26192 = CARTESIAN_POINT ( 'NONE',  ( -36.07812499999994316, -114.9929510916434339, 14.11852480586264846 ) ) ;
#26193 = LINE ( 'NONE', #34661, #15090 ) ;
#26194 = EDGE_CURVE ( 'NONE', #251, #4339, #35573, .T. ) ;
#26195 = CARTESIAN_POINT ( 'NONE',  ( 0.000000000000000000, -44.61570720899084819, -14.73072383765613935 ) ) ;
#26196 = VERTEX_POINT ( 'NONE', #10898 ) ;
#26197 = CARTESIAN_POINT ( 'NONE',  ( -35.50000000000000000, -115.9929510916434481, 12.59102132592610346 ) ) ;
#26198 = CARTESIAN_POINT ( 'NONE',  ( -35.50000000000000711, -115.9630435732166518, -0.9469505670456015434 ) ) ;
#26199 = FILL_AREA_STYLE ('',( #28904 ) ) ;
#26200 = DIRECTION ( 'NONE',  ( -1.000000000000000000, 0.000000000000000000, -0.000000000000000000 ) ) ;
#26201 = VECTOR ( 'NONE', #22563, 1000.000000000000000 ) ;
#26202 = DIRECTION ( 'NONE',  ( 0.000000000000000000, -0.9510565162951500895, -0.3090169943749581649 ) ) ;
#26203 = DIRECTION ( 'NONE',  ( 0.000000000000000000, 0.000000000000000000, 1.000000000000000000 ) ) ;
#26204 = DIRECTION ( 'NONE',  ( -1.000000000000000000, 0.000000000000000000, 0.000000000000000000 ) ) ;
#26205 = ADVANCED_FACE ( 'NONE', ( #16262, #32681 ), #8004, .T. ) ;
#26206 = FACE_OUTER_BOUND ( 'NONE', #32447, .T. ) ;
#26207 = DIRECTION ( 'NONE',  ( 0.000000000000000000, -0.9980267284282723361, 0.06279051952930261860 ) ) ;
#26208 = EDGE_LOOP ( 'NONE', ( #13549, #28313, #29213, #491 ) ) ;
#26209 = ADVANCED_FACE ( 'NONE', ( #18988 ), #21863, .T. ) ;
#26210 = EDGE_CURVE ( 'NONE', #4109, #8679, #35384, .T. ) ;
#26211 = CARTESIAN_POINT ( 'NONE',  ( -37.97545270896702618, -114.4734759653044023, 9.152725545821551734 ) ) ;
#26212 = CARTESIAN_POINT ( 'NONE',  ( -46.00000000000000000, -25.98076211353320275, 84.99999999999992895 ) ) ;
#26213 = CARTESIAN_POINT ( 'NONE',  ( 7.999999999999992895, -2.123073309835510791, 47.45152853935334747 ) ) ;
#26214 = VERTEX_POINT ( 'NONE', #29811 ) ;
#26215 = CIRCLE ( 'NONE', #15861, 52.00000000000000711 ) ;
#26216 = ORIENTED_EDGE ( 'NONE', *, *, #20173, .T. ) ;
#26217 = DIRECTION ( 'NONE',  ( 0.000000000000000000, 0.4999999999999989453, 0.8660254037844392627 ) ) ;
#26218 = VERTEX_POINT ( 'NONE', #32856 ) ;
#26219 = CARTESIAN_POINT ( 'NONE',  ( -34.97545270896703329, -114.7691647218148745, 2.590225545821551734 ) ) ;
#26220 = EDGE_CURVE ( 'NONE', #7064, #16271, #26273, .T. ) ;
#26221 = ORIENTED_EDGE ( 'NONE', *, *, #30560, .F. ) ;
#26222 = EDGE_CURVE ( 'NONE', #4505, #9311, #10746, .T. ) ;
#26223 = DIRECTION ( 'NONE',  ( 0.000000000000000000, -0.8660254037844431485, 0.4999999999999921729 ) ) ;
#26224 = ORIENTED_EDGE ( 'NONE', *, *, #11458, .T. ) ;
#26225 = CARTESIAN_POINT ( 'NONE',  ( 50.00000000000000000, 10.00000000000000888, 110.0000000000000000 ) ) ;
#26226 = CIRCLE ( 'NONE', #22759, 52.00000000000000711 ) ;
#26227 = CARTESIAN_POINT ( 'NONE',  ( 7.999999999999992895, 42.41764978026606769, 20.20639853260304619 ) ) ;
#26228 = AXIS2_PLACEMENT_3D ( 'NONE', #14933, #1265, #17458 ) ;
#26229 = AXIS2_PLACEMENT_3D ( 'NONE', #34366, #6622, #22638 ) ;
#26230 = CARTESIAN_POINT ( 'NONE',  ( 50.00000000000000711, -25.98076211353320275, 78.99999999999992895 ) ) ;
#26231 = VERTEX_POINT ( 'NONE', #13589 ) ;
#26232 = ORIENTED_EDGE ( 'NONE', *, *, #32745, .F. ) ;
#26233 = AXIS2_PLACEMENT_3D ( 'NONE', #32492, #5156, #5328 ) ;
#26234 = CARTESIAN_POINT ( 'NONE',  ( 70.00001200000001234, -29.87665282020647695, 86.04699153743705153 ) ) ;
#26235 = DIRECTION ( 'NONE',  ( -1.000000000000000000, 0.000000000000000000, 0.000000000000000000 ) ) ;
#26236 = ORIENTED_EDGE ( 'NONE', *, *, #18719, .F. ) ;
#26237 = DIRECTION ( 'NONE',  ( -1.000000000000000000, -0.000000000000000000, -0.000000000000000000 ) ) ;
#26238 = ADVANCED_FACE ( 'NONE', ( #24758 ), #24582, .T. ) ;
#26239 = AXIS2_PLACEMENT_3D ( 'NONE', #30379, #5704, #16664 ) ;
#26240 = CARTESIAN_POINT ( 'NONE',  ( 0.000000000000000000, 0.6505223195690454929, -51.99593080916758936 ) ) ;
#26241 = DIRECTION ( 'NONE',  ( 1.000000000000000000, 1.734723475976807094E-16, 0.000000000000000000 ) ) ;
#26242 = CARTESIAN_POINT ( 'NONE',  ( -35.80421860361284558, -115.9929510916434481, 14.10650203519841916 ) ) ;
#26243 = EDGE_CURVE ( 'NONE', #2951, #3338, #11071, .T. ) ;
#26244 = CYLINDRICAL_SURFACE ( 'NONE', #27256, 4.000000000000000000 ) ;
#26245 = CARTESIAN_POINT ( 'NONE',  ( 7.999999999999992895, 47.00885577955422434, -6.806061952191799769 ) ) ;
#26246 = EDGE_CURVE ( 'NONE', #8832, #3989, #19330, .T. ) ;
#26247 = CARTESIAN_POINT ( 'NONE',  ( -34.50000000000000000, -115.9915791193162420, 10.43066258751475139 ) ) ;
#26248 = CARTESIAN_POINT ( 'NONE',  ( 0.9999999999999453770, -6.008326913195871199, -0.7999999999999951594 ) ) ;
#26249 = DIRECTION ( 'NONE',  ( 1.000000000000000000, 0.000000000000000000, 0.000000000000000000 ) ) ;
#26250 = CARTESIAN_POINT ( 'NONE',  ( 0.000000000000000000, -2.710505431213761085E-17, -46.00000000000000000 ) ) ;
#26251 = CARTESIAN_POINT ( 'NONE',  ( 0.000000000000000000, 14.87816164169121080, -4.342730381189718436 ) ) ;
#26252 = AXIS2_PLACEMENT_3D ( 'NONE', #20872, #33081, #5711 ) ;
#26253 = CARTESIAN_POINT ( 'NONE',  ( -1.498621416870349332, 0.000000000000000000, 0.000000000000000000 ) ) ;
#26254 = DIRECTION ( 'NONE',  ( 0.000000000000000000, 0.000000000000000000, -1.000000000000000000 ) ) ;
#26255 = ORIENTED_EDGE ( 'NONE', *, *, #14093, .F. ) ;
#26256 = ADVANCED_FACE ( 'NONE', ( #27643 ), #18628, .T. ) ;
#26257 = CARTESIAN_POINT ( 'NONE',  ( -40.02454729103296671, -112.8166217158120332, 3.340225545821551290 ) ) ;
#26258 = EDGE_CURVE ( 'NONE', #27614, #7369, #605, .T. ) ;
#26259 = DIRECTION ( 'NONE',  ( -1.000000000000000000, -0.000000000000000000, -0.000000000000000000 ) ) ;
#26260 = CIRCLE ( 'NONE', #30851, 13.99999999999999645 ) ;
#26261 = CARTESIAN_POINT ( 'NONE',  ( -35.50000000000000000, -113.0140978167138712, 0.0002176474015660057743 ) ) ;
#26262 = VERTEX_POINT ( 'NONE', #11418 ) ;
#26263 = ORIENTED_EDGE ( 'NONE', *, *, #7913, .T. ) ;
#26264 = AXIS2_PLACEMENT_3D ( 'NONE', #1690, #28872, #15163 ) ;
#26265 = CARTESIAN_POINT ( 'NONE',  ( 46.00000000000000000, -25.98076211353320275, 84.99999999999992895 ) ) ;
#26266 = CARTESIAN_POINT ( 'NONE',  ( 5.400000000000071410, 0.9999999999999662492, 55.00000000000000711 ) ) ;
#26267 = ORIENTED_EDGE ( 'NONE', *, *, #19460, .T. ) ;
#26268 = AXIS2_PLACEMENT_3D ( 'NONE', #27319, #2317, #24266 ) ;
#26269 = ORIENTED_EDGE ( 'NONE', *, *, #20914, .T. ) ;
#26271 = EDGE_LOOP ( 'NONE', ( #24421, #8263, #21247, #26489 ) ) ;
#26270 = AXIS2_PLACEMENT_3D ( 'NONE', #8846, #5640, #24893 ) ;
#26272 = EDGE_CURVE ( 'NONE', #9129, #8057, #14451, .T. ) ;
#26273 = CIRCLE ( 'NONE', #979, 0.2000000000000005107 ) ;
#26274 = LINE ( 'NONE', #17791, #28062 ) ;
#26275 = CYLINDRICAL_SURFACE ( 'NONE', #18850, 3.799999999999999822 ) ;
#26276 = CARTESIAN_POINT ( 'NONE',  ( 7.999999999999992895, 39.55064067543064965, 25.36340625197373910 ) ) ;
#26277 = ORIENTED_EDGE ( 'NONE', *, *, #24342, .T. ) ;
#26278 = ORIENTED_EDGE ( 'NONE', *, *, #10722, .F. ) ;
#26279 = CARTESIAN_POINT ( 'NONE',  ( -35.50000000000000000, -111.7850029017436810, -2.224114562373086912 ) ) ;
#26280 = CIRCLE ( 'NONE', #10756, 20.00000000000000711 ) ;
#26281 = CARTESIAN_POINT ( 'NONE',  ( 8.000000000000000000, 14.87816164169115218, 4.342730381189920941 ) ) ;
#26282 = DIRECTION ( 'NONE',  ( 1.000000000000000000, 0.000000000000000000, 0.000000000000000000 ) ) ;
#26283 = VERTEX_POINT ( 'NONE', #22556 ) ;
#26284 = CARTESIAN_POINT ( 'NONE',  ( -37.51635661748575501, -114.9929510916434339, 13.11827392651459157 ) ) ;
#26285 = AXIS2_PLACEMENT_3D ( 'NONE', #18452, #12888, #29449 ) ;
#26286 = EDGE_CURVE ( 'NONE', #34443, #29380, #11238, .T. ) ;
#26287 = AXIS2_PLACEMENT_3D ( 'NONE', #25247, #17119, #14066 ) ;
#26288 = ADVANCED_FACE ( 'NONE', ( #14820 ), #9245, .F. ) ;
#26289 = CARTESIAN_POINT ( 'NONE',  ( -34.50000000000000000, -114.9929510916434339, 10.55026311463432087 ) ) ;
#26290 = AXIS2_PLACEMENT_3D ( 'NONE', #15552, #1908, #10177 ) ;
#26291 = FACE_BOUND ( 'NONE', #1780, .T. ) ;
#26292 = VECTOR ( 'NONE', #25339, 1000.000000000000227 ) ;
#26293 = CARTESIAN_POINT ( 'NONE',  ( -37.80727372874345349, -114.9929510916434339, 13.01835785830664527 ) ) ;
#26294 = CARTESIAN_POINT ( 'NONE',  ( -42.49999999999999289, -31.64142946139416424, 97.80456345124107997 ) ) ;
#26295 = CARTESIAN_POINT ( 'NONE',  ( -39.00000000000000000, -113.9929510916434339, 11.91443571948719615 ) ) ;
#26296 = DIRECTION ( 'NONE',  ( 0.000000000000000000, 0.000000000000000000, -1.000000000000000000 ) ) ;
#26297 = DIRECTION ( 'NONE',  ( -1.000000000000000000, 0.000000000000000000, 0.000000000000000000 ) ) ;
#26298 = DIRECTION ( 'NONE',  ( 0.000000000000000000, -0.4999999999999888978, -0.8660254037844450359 ) ) ;
#26299 = ORIENTED_EDGE ( 'NONE', *, *, #27523, .F. ) ;
#26300 = CARTESIAN_POINT ( 'NONE',  ( 0.000000000000000000, 11.46872990052444408, -45.56340405422432127 ) ) ;
#26301 = DIRECTION ( 'NONE',  ( -1.000000000000000000, 0.000000000000000000, 0.000000000000000000 ) ) ;
#26302 = VERTEX_POINT ( 'NONE', #8532 ) ;
#26303 = CARTESIAN_POINT ( 'NONE',  ( -35.50000000000000711, -114.9929510916434339, 10.94631322572069365 ) ) ;
#26304 = VERTEX_POINT ( 'NONE', #25460 ) ;
#26305 = EDGE_CURVE ( 'NONE', #15074, #25051, #11587, .T. ) ;
#26306 = CARTESIAN_POINT ( 'NONE',  ( -36.23083527818512550, -116.0245472910329880, 1.784774454178448932 ) ) ;
#26307 = AXIS2_PLACEMENT_3D ( 'NONE', #8214, #16838, #22075 ) ;
#26308 = ORIENTED_EDGE ( 'NONE', *, *, #31500, .F. ) ;
#26309 = DIRECTION ( 'NONE',  ( -1.000000000000000000, 0.000000000000000000, 0.000000000000000000 ) ) ;
#26310 = ORIENTED_EDGE ( 'NONE', *, *, #28883, .F. ) ;
#26311 = VECTOR ( 'NONE', #7673, 1000.000000000000000 ) ;
#26312 = CARTESIAN_POINT ( 'NONE',  ( -34.50000000000000000, -113.0140978167137717, -0.6411448143358797758 ) ) ;
#26313 = DIRECTION ( 'NONE',  ( 1.000000000000000000, -0.000000000000000000, -0.000000000000000000 ) ) ;
#26314 = CARTESIAN_POINT ( 'NONE',  ( -38.99999999999999289, -113.9407375970686900, 6.753524454178448266 ) ) ;
#26315 = EDGE_LOOP ( 'NONE', ( #24644, #30254 ) ) ;
#26316 = CARTESIAN_POINT ( 'NONE',  ( -38.30190309005061522, -116.9754527089670546, 1.972274454178448932 ) ) ;
#26317 = CIRCLE ( 'NONE', #8492, 47.49900000000000944 ) ;
#26318 = VECTOR ( 'NONE', #34776, 1000.000000000000000 ) ;
#26319 = VECTOR ( 'NONE', #12092, 1000.000000000000000 ) ;
#26320 = FACE_BOUND ( 'NONE', #4598, .T. ) ;
#26321 = CARTESIAN_POINT ( 'NONE',  ( -35.50000000000000711, -116.0140896356112989, -0.6575071456984549201 ) ) ;
#26322 = ORIENTED_EDGE ( 'NONE', *, *, #35259, .F. ) ;
#26323 = ORIENTED_EDGE ( 'NONE', *, *, #34999, .F. ) ;
#26324 = CARTESIAN_POINT ( 'NONE',  ( -50.00000000000000000, 10.00000000000000888, 110.0000000000000000 ) ) ;
#26325 = AXIS2_PLACEMENT_3D ( 'NONE', #8014, #29461, #8188 ) ;
#26326 = CARTESIAN_POINT ( 'NONE',  ( -44.00000000000000000, 0.000000000000000000, 0.000000000000000000 ) ) ;
#26327 = ORIENTED_EDGE ( 'NONE', *, *, #5103, .F. ) ;
#26328 = EDGE_LOOP ( 'NONE', ( #13035, #11177, #879, #4597 ) ) ;
#26329 = CARTESIAN_POINT ( 'NONE',  ( -34.50000000000000000, -112.8690837874180062, 2.872105769100646189 ) ) ;
#26330 = CARTESIAN_POINT ( 'NONE',  ( -35.50000000000000711, -112.1222502514821144, 1.343475657184566296 ) ) ;
#26331 = CARTESIAN_POINT ( 'NONE',  ( 0.000000000000000000, 0.000000000000000000, 0.000000000000000000 ) ) ;
#26332 = ORIENTED_EDGE ( 'NONE', *, *, #22013, .T. ) ;
#26333 = ORIENTED_EDGE ( 'NONE', *, *, #17819, .F. ) ;
#26334 = LINE ( 'NONE', #32086, #9155 ) ;
#26335 = CIRCLE ( 'NONE', #34380, 4.800000000000004263 ) ;
#26336 = ADVANCED_FACE ( 'NONE', ( #16973 ), #27981, .T. ) ;
#26337 = AXIS2_PLACEMENT_3D ( 'NONE', #6483, #3799, #28454 ) ;
#26338 = CARTESIAN_POINT ( 'NONE',  ( -38.00000000000000711, -113.9929510916434339, 11.21034663311206181 ) ) ;
#26339 = DIRECTION ( 'NONE',  ( -1.047965281155519667E-16, -6.938893903907192632E-17, -1.000000000000000000 ) ) ;
#26340 = CARTESIAN_POINT ( 'NONE',  ( -35.50000000000000000, -113.9929510916434339, 10.68227981832981044 ) ) ;
#26341 = AXIS2_PLACEMENT_3D ( 'NONE', #7365, #26636, #13135 ) ;
#26342 = CARTESIAN_POINT ( 'NONE',  ( -35.91854304697312728, -115.9929510916434481, 13.11211614918345703 ) ) ;
#26343 = DIRECTION ( 'NONE',  ( -1.000000000000000000, 0.000000000000000000, 0.000000000000000000 ) ) ;
#26344 = VECTOR ( 'NONE', #8236, 1000.000000000000000 ) ;
#26345 = CARTESIAN_POINT ( 'NONE',  ( -10.00000000000000178, 0.000000000000000000, 0.000000000000000000 ) ) ;
#26346 = ORIENTED_EDGE ( 'NONE', *, *, #11674, .T. ) ;
#26347 = CARTESIAN_POINT ( 'NONE',  ( 0.000000000000000000, -18.53613841426757602, -48.58406706613921244 ) ) ;
#26348 = DIRECTION ( 'NONE',  ( -1.000000000000000000, -0.000000000000000000, -0.000000000000000000 ) ) ;
#26349 = COLOUR_RGB ( '', 0.08235294, 0.09019608, 0.10196078) ;
#26350 = LINE ( 'NONE', #23268, #17982 ) ;
#26351 = ORIENTED_EDGE ( 'NONE', *, *, #27329, .T. ) ;
#26352 = DIRECTION ( 'NONE',  ( 0.000000000000000000, 0.000000000000000000, 1.000000000000000000 ) ) ;
#26353 = CARTESIAN_POINT ( 'NONE',  ( -35.50000000000000711, -115.0795240838853886, -1.623175561345890472 ) ) ;
#26354 = LINE ( 'NONE', #35003, #21306 ) ;
#26355 = ITEM_DEFINED_TRANSFORMATION ( 'NONE', 'NONE', #31674,  #21307 ) ;
#26356 = CARTESIAN_POINT ( 'NONE',  ( -35.50000000000000711, -114.1264797827112574, 9.515205387299289441 ) ) ;
#26357 = DIRECTION ( 'NONE',  ( 1.000000000000000000, 1.734723475976807094E-16, 0.000000000000000000 ) ) ;
#26358 = ORIENTED_EDGE ( 'NONE', *, *, #25355, .F. ) ;
#26359 = FACE_OUTER_BOUND ( 'NONE', #24237, .T. ) ;
#26360 = CARTESIAN_POINT ( 'NONE',  ( -34.50000000000000000, -112.7530559548648341, -2.608751991713152307 ) ) ;
#26361 = DIRECTION ( 'NONE',  ( -1.000000000000000000, 0.000000000000000000, 0.000000000000000000 ) ) ;
#26362 = VERTEX_POINT ( 'NONE', #20197 ) ;
#26363 = VERTEX_POINT ( 'NONE', #19506 ) ;
#26364 = CARTESIAN_POINT ( 'NONE',  ( -37.97545270896701908, -113.5265240346955977, 5.347274454178449155 ) ) ;
#26365 = AXIS2_PLACEMENT_3D ( 'NONE', #34693, #31449, #1209 ) ;
#26366 =( NAMED_UNIT ( * ) PLANE_ANGLE_UNIT ( ) SI_UNIT ( $, .RADIAN. ) );
#26367 = ORIENTED_EDGE ( 'NONE', *, *, #14396, .T. ) ;
#26368 = ORIENTED_EDGE ( 'NONE', *, *, #7109, .F. ) ;
#26369 = VECTOR ( 'NONE', #30660, 1000.000000000000000 ) ;
#26370 = CARTESIAN_POINT ( 'NONE',  ( -35.50000000000000000, -115.0140978167138712, 0.0002176474015578471800 ) ) ;
#26371 = DIRECTION ( 'NONE',  ( 0.02857142857143298714, -0.9995917534020514195, -4.555780455966493806E-16 ) ) ;
#26372 = DIRECTION ( 'NONE',  ( -1.000000000000000000, 0.000000000000000000, 0.000000000000000000 ) ) ;
#26373 = EDGE_CURVE ( 'NONE', #3282, #17290, #24330, .T. ) ;
#26374 = CARTESIAN_POINT ( 'NONE',  ( -37.66108410722335265, -114.9929510916434339, 13.09299768411426790 ) ) ;
#26375 = CARTESIAN_POINT ( 'NONE',  ( 4.000000000000003553, 19.83898331853685448, 9.508666619816713350 ) ) ;
#26376 = EDGE_CURVE ( 'NONE', #5465, #4806, #28351, .T. ) ;
#26377 = CARTESIAN_POINT ( 'NONE',  ( -34.57658136524562309, -114.9929510916434339, 13.10177712753338497 ) ) ;
#26378 = DIRECTION ( 'NONE',  ( 1.000000000000000000, -1.110223024625156540E-16, 0.000000000000000000 ) ) ;
#26379 = CARTESIAN_POINT ( 'NONE',  ( 5.400000000000003020, 1.000000000000000888, -22.00000000000000000 ) ) ;
#26380 = ORIENTED_EDGE ( 'NONE', *, *, #7218, .F. ) ;
#26381 = EDGE_CURVE ( 'NONE', #751, #15153, #16246, .T. ) ;
#26382 = CARTESIAN_POINT ( 'NONE',  ( -35.60016694755736211, -115.9929510916434481, 12.92579853460621386 ) ) ;
#26383 = CARTESIAN_POINT ( 'NONE',  ( -35.50000000000000711, -116.0140978167138712, 0.6252176474015648244 ) ) ;
#26384 = DIRECTION ( 'NONE',  ( -1.000000000000000000, 0.000000000000000000, 0.000000000000000000 ) ) ;
#26385 = FACE_OUTER_BOUND ( 'NONE', #10913, .T. ) ;
#26386 = AXIS2_PLACEMENT_3D ( 'NONE', #34121, #32089, #14478 ) ;
#26387 = CARTESIAN_POINT ( 'NONE',  ( 7.999999999999992895, -6.109652351741458709, -46.58570277113513214 ) ) ;
#26388 = ORIENTED_EDGE ( 'NONE', *, *, #25567, .T. ) ;
#26389 = EDGE_CURVE ( 'NONE', #28254, #24948, #12238, .T. ) ;
#26390 = VECTOR ( 'NONE', #11973, 1000.000000000000000 ) ;
#26391 = LINE ( 'NONE', #20603, #5588 ) ;
#26392 = PLANE ( 'NONE',  #3208 ) ;
#26393 = DIRECTION ( 'NONE',  ( 0.000000000000000000, -0.6427876096865456912, 0.7660444431189726844 ) ) ;
#26394 = CYLINDRICAL_SURFACE ( 'NONE', #32788, 7.199999999999993960 ) ;
#26395 = EDGE_LOOP ( 'NONE', ( #28468, #25023, #16736, #24332 ) ) ;
#26396 = CARTESIAN_POINT ( 'NONE',  ( -35.99999999999999289, -114.0592624029313242, 4.503524454178447378 ) ) ;
#26397 = DIRECTION ( 'NONE',  ( 0.000000000000000000, 0.000000000000000000, 1.000000000000000000 ) ) ;
#26398 = FACE_OUTER_BOUND ( 'NONE', #18736, .T. ) ;
#26399 = ORIENTED_EDGE ( 'NONE', *, *, #2269, .T. ) ;
#26400 = ORIENTED_EDGE ( 'NONE', *, *, #22741, .T. ) ;
#26401 = FILL_AREA_STYLE ('',( #34685 ) ) ;
#26402 = DIRECTION ( 'NONE',  ( -1.000000000000000000, 1.734723475976807094E-16, 0.000000000000000000 ) ) ;
#26403 = ORIENTED_EDGE ( 'NONE', *, *, #25112, .F. ) ;
#26404 = CARTESIAN_POINT ( 'NONE',  ( -37.76916472181486739, -116.0245472910329880, 2.965225545821551290 ) ) ;
#26405 = VERTEX_POINT ( 'NONE', #968 ) ;
#26406 = EDGE_CURVE ( 'NONE', #908, #5854, #178, .T. ) ;
#26407 = CARTESIAN_POINT ( 'NONE',  ( -3.799999999999999822, 4.382607293638566128E-16, 38.90000000000000568 ) ) ;
#26408 = VERTEX_POINT ( 'NONE', #27813 ) ;
#26409 = ORIENTED_EDGE ( 'NONE', *, *, #16358, .F. ) ;
#26410 = CARTESIAN_POINT ( 'NONE',  ( 4.000000000000003553, -13.56094713063537327, -50.20060470671755581 ) ) ;
#26411 = CARTESIAN_POINT ( 'NONE',  ( 8.000000000000000000, -15.46619997295641369, -1.007799283846847471 ) ) ;
#26412 = AXIS2_PLACEMENT_3D ( 'NONE', #11609, #33236, #14132 ) ;
#26413 = CARTESIAN_POINT ( 'NONE',  ( -42.49999999999999289, -27.93100416606583991, 81.50764321173598148 ) ) ;
#26414 = ORIENTED_EDGE ( 'NONE', *, *, #22694, .T. ) ;
#26415 = ORIENTED_EDGE ( 'NONE', *, *, #18068, .F. ) ;
#26416 = CIRCLE ( 'NONE', #27047, 4.000000000000000000 ) ;
#26417 = EDGE_CURVE ( 'NONE', #17643, #22617, #19842, .T. ) ;
#26418 = DIRECTION ( 'NONE',  ( 1.000000000000000000, -0.000000000000000000, -0.000000000000000000 ) ) ;
#26419 = CARTESIAN_POINT ( 'NONE',  ( -0.1085714285714300953, -3.798448662927791819, -0.7999999999999951594 ) ) ;
#26420 = EDGE_CURVE ( 'NONE', #5854, #26576, #31028, .T. ) ;
#26421 = EDGE_CURVE ( 'NONE', #7183, #20895, #25100, .T. ) ;
#26423 = VERTEX_POINT ( 'NONE', #28157 ) ;
#26422 = AXIS2_PLACEMENT_3D ( 'NONE', #27930, #13894, #3278 ) ;
#26424 = DIRECTION ( 'NONE',  ( -1.000000000000000000, 0.000000000000000000, 0.000000000000000000 ) ) ;
#26425 = CIRCLE ( 'NONE', #28732, 8.000000000000000000 ) ;
#26426 = FACE_OUTER_BOUND ( 'NONE', #5292, .T. ) ;
#26427 = CARTESIAN_POINT ( 'NONE',  ( -50.00000000000000000, 0.000000000000000000, 70.00000000000000000 ) ) ;
#26428 = CARTESIAN_POINT ( 'NONE',  ( -36.01562499999997158, -115.9929510916434481, 14.11852480586265024 ) ) ;
#26429 = CARTESIAN_POINT ( 'NONE',  ( 1.599999999999990985, -4.753539400292362697E-14, 7.020000000000020890 ) ) ;
#26430 = CARTESIAN_POINT ( 'NONE',  ( -36.94073759706868287, -112.0000000000000142, 4.128524454178449155 ) ) ;
#26431 = EDGE_CURVE ( 'NONE', #14725, #2330, #30855, .T. ) ;
#26432 = CARTESIAN_POINT ( 'NONE',  ( -34.50000000000000000, -115.9929524668003182, 10.51038305125561401 ) ) ;
#26433 = CARTESIAN_POINT ( 'NONE',  ( 7.999999999999992895, -49.25004636492401033, 16.68630974939741662 ) ) ;
#26434 = EDGE_CURVE ( 'NONE', #15509, #19295, #14627, .T. ) ;
#26435 = CARTESIAN_POINT ( 'NONE',  ( 8.000000000000000000, -5.482169781018935595, 16.00140663693123599 ) ) ;
#26436 = CYLINDRICAL_SURFACE ( 'NONE', #8388, 20.00000000000000355 ) ;
#26437 = DIRECTION ( 'NONE',  ( -1.000000000000000000, 0.000000000000000000, 0.000000000000000000 ) ) ;
#26438 = FACE_OUTER_BOUND ( 'NONE', #31527, .T. ) ;
#26439 = ORIENTED_EDGE ( 'NONE', *, *, #1833, .T. ) ;
#26440 = CIRCLE ( 'NONE', #11489, 6.984000000000015085 ) ;
#26441 = CARTESIAN_POINT ( 'NONE',  ( -37.05926240293131713, -112.0000000000000142, 5.121475545821551734 ) ) ;
#26442 = DIRECTION ( 'NONE',  ( -1.000000000000000000, -0.000000000000000000, -0.000000000000000000 ) ) ;
#26443 = CARTESIAN_POINT ( 'NONE',  ( -35.50000000000000000, -113.0140978167138712, -0.6247823525985405357 ) ) ;
#26444 = ORIENTED_EDGE ( 'NONE', *, *, #23066, .T. ) ;
#26445 = AXIS2_PLACEMENT_3D ( 'NONE', #21931, #19408, #19912 ) ;
#26446 = ORIENTED_EDGE ( 'NONE', *, *, #25393, .F. ) ;
#26447 = CARTESIAN_POINT ( 'NONE',  ( 0.000000000000000000, 47.32430374665962347, -21.55018039121475582 ) ) ;
#26448 = FACE_OUTER_BOUND ( 'NONE', #18021, .T. ) ;
#26449 = ORIENTED_EDGE ( 'NONE', *, *, #30915, .T. ) ;
#26450 = VERTEX_POINT ( 'NONE', #6534 ) ;
#26451 = STYLED_ITEM ( 'NONE', ( #24972 ), #10370 ) ;
#26452 = CARTESIAN_POINT ( 'NONE',  ( 0.000000000000000000, 9.508666619816942500, -19.83898331853677632 ) ) ;
#26453 = VECTOR ( 'NONE', #35055, 1000.000000000000000 ) ;
#26454 = VERTEX_POINT ( 'NONE', #28506 ) ;
#26455 = EDGE_CURVE ( 'NONE', #23525, #28758, #32413, .T. ) ;
#26456 = CARTESIAN_POINT ( 'NONE',  ( 7.999999999999992895, 20.99948489194482448, -42.60488980472762677 ) ) ;
#26457 = DIRECTION ( 'NONE',  ( -1.783119874454246424E-31, -1.187911941725854497E-31, 1.000000000000000000 ) ) ;
#26458 = DIRECTION ( 'NONE',  ( 1.000000000000000000, 0.000000000000000000, 0.000000000000000000 ) ) ;
#26459 = DIRECTION ( 'NONE',  ( 0.000000000000000000, 0.000000000000000000, -1.000000000000000000 ) ) ;
#26460 = VERTEX_POINT ( 'NONE', #18370 ) ;
#26461 = VERTEX_POINT ( 'NONE', #26847 ) ;
#26462 = CARTESIAN_POINT ( 'NONE',  ( -35.50000000000000711, -113.0557643173828524, -1.624792769101735868 ) ) ;
#26463 = DIRECTION ( 'NONE',  ( 0.000000000000000000, 0.000000000000000000, -1.000000000000000000 ) ) ;
#26464 = EDGE_CURVE ( 'NONE', #14939, #10958, #9945, .T. ) ;
#26465 = VECTOR ( 'NONE', #67, 1000.000000000000114 ) ;
#26466 = EDGE_CURVE ( 'NONE', #5432, #15608, #737, .T. ) ;
#26467 = CARTESIAN_POINT ( 'NONE',  ( 46.00000000000000000, -25.98076211353320275, 76.99999999999992895 ) ) ;
#26468 = ORIENTED_EDGE ( 'NONE', *, *, #23949, .F. ) ;
#26469 = CARTESIAN_POINT ( 'NONE',  ( -3.799999999999999822, 4.382607293638566128E-16, 29.09999999999999787 ) ) ;
#26470 = VECTOR ( 'NONE', #29361, 1000.000000000000000 ) ;
#26471 = CARTESIAN_POINT ( 'NONE',  ( -34.50000000000000000, -112.9415908020655195, 1.873661708251232572 ) ) ;
#26472 = CARTESIAN_POINT ( 'NONE',  ( -34.50015059926905536, -114.9929510916434339, 12.64306614848962695 ) ) ;
#26473 = DIRECTION ( 'NONE',  ( 0.000000000000000000, 0.000000000000000000, 1.000000000000000000 ) ) ;
#26474 = CARTESIAN_POINT ( 'NONE',  ( -37.50613590685470911, -114.9929510916434339, 13.11852378322482515 ) ) ;
#26475 = CARTESIAN_POINT ( 'NONE',  ( 8.000000000000000000, -6.860320204751044315, -13.89802171851389900 ) ) ;
#26476 = AXIS2_PLACEMENT_3D ( 'NONE', #27984, #20375, #608 ) ;
#26477 = AXIS2_PLACEMENT_3D ( 'NONE', #12545, #20431, #4636 ) ;
#26478 = CARTESIAN_POINT ( 'NONE',  ( -34.50000000000000000, -114.1264797827112574, 9.515205387299289441 ) ) ;
#26480 = DIRECTION ( 'NONE',  ( 0.000000000000000000, 0.000000000000000000, -1.000000000000000000 ) ) ;
#26479 = AXIS2_PLACEMENT_3D ( 'NONE', #754, #3303, #11920 ) ;
#26481 = ADVANCED_FACE ( 'NONE', ( #21418 ), #21585, .T. ) ;
#26482 = DIRECTION ( 'NONE',  ( 0.000000000000000000, 0.000000000000000000, 1.000000000000000000 ) ) ;
#26483 =( NAMED_UNIT ( * ) SI_UNIT ( $, .STERADIAN. ) SOLID_ANGLE_UNIT ( ) );
#26484 = VERTEX_POINT ( 'NONE', #7563 ) ;
#26485 = LINE ( 'NONE', #4535, #16400 ) ;
#26486 = DIRECTION ( 'NONE',  ( 1.000000000000000000, -0.000000000000000000, -0.000000000000000000 ) ) ;
#26487 = VERTEX_POINT ( 'NONE', #7397 ) ;
#26488 = CARTESIAN_POINT ( 'NONE',  ( -37.80727372874345349, -114.9929510916434339, 13.01835785830664527 ) ) ;
#26489 = ORIENTED_EDGE ( 'NONE', *, *, #10573, .F. ) ;
#26490 = CARTESIAN_POINT ( 'NONE',  ( 8.000000000000000000, -14.87816164169118416, 4.342730381189816136 ) ) ;
#26491 = CARTESIAN_POINT ( 'NONE',  ( 8.000000000000000000, 0.000000000000000000, 4.000000000000000000 ) ) ;
#26492 = ORIENTED_EDGE ( 'NONE', *, *, #32076, .T. ) ;
#26493 = CARTESIAN_POINT ( 'NONE',  ( -1.479000000000007642, -3.480549182199860587E-16, -5.016000000000010672 ) ) ;
#26494 = ORIENTED_EDGE ( 'NONE', *, *, #17647, .F. ) ;
#26495 = CARTESIAN_POINT ( 'NONE',  ( -34.50000000000000000, -113.0256022645180707, 0.8765908897032291813 ) ) ;
#26496 = DIRECTION ( 'NONE',  ( 0.000000000000000000, 0.000000000000000000, -1.000000000000000000 ) ) ;
#26497 = DIRECTION ( 'NONE',  ( 0.000000000000000000, 0.000000000000000000, 1.000000000000000000 ) ) ;
#26498 = CIRCLE ( 'NONE', #24201, 19.99999999999998579 ) ;
#26499 = EDGE_LOOP ( 'NONE', ( #28847, #17606, #9514, #7704 ) ) ;
#26500 = CARTESIAN_POINT ( 'NONE',  ( -38.99999999999999289, -113.9407375970686900, 8.253524454178448266 ) ) ;
#26501 = ADVANCED_FACE ( 'NONE', ( #29370 ), #4715, .T. ) ;
#26502 = CIRCLE ( 'NONE', #27064, 17.49900000000000233 ) ;
#26503 = EDGE_CURVE ( 'NONE', #33824, #21774, #8219, .T. ) ;
#26504 = CARTESIAN_POINT ( 'NONE',  ( 0.000000000000000000, 0.3212489022567689423, -16.91141623315866482 ) ) ;
#26505 = DIRECTION ( 'NONE',  ( 1.000000000000000000, 0.000000000000000000, 0.000000000000000000 ) ) ;
#26506 = ORIENTED_EDGE ( 'NONE', *, *, #28893, .T. ) ;
#26508 = VERTEX_POINT ( 'NONE', #5240 ) ;
#26507 = EDGE_CURVE ( 'NONE', #31835, #21432, #18901, .T. ) ;
#26509 = DIRECTION ( 'NONE',  ( 1.000000000000000000, 0.000000000000000000, 0.000000000000000000 ) ) ;
#26510 =( LENGTH_UNIT ( ) NAMED_UNIT ( * ) SI_UNIT ( .MILLI., .METRE. ) );
#26511 = CARTESIAN_POINT ( 'NONE',  ( 7.999999999999992895, -39.78933988720132220, 24.98727647984988565 ) ) ;
#26512 = VERTEX_POINT ( 'NONE', #29194 ) ;
#26513 = VERTEX_POINT ( 'NONE', #29547 ) ;
#26514 = CARTESIAN_POINT ( 'NONE',  ( -34.50000000000000000, -115.0795240838853886, -1.623175561345890472 ) ) ;
#26515 = PRODUCT_DEFINITION_SHAPE ( 'NONE', 'NONE',  #35616 ) ;
#26516 = EDGE_CURVE ( 'NONE', #31713, #19471, #7201, .T. ) ;
#26517 = CARTESIAN_POINT ( 'NONE',  ( 8.000000000000000000, 4.460989585141205360, -16.92083251265323085 ) ) ;
#26518 = EDGE_LOOP ( 'NONE', ( #19811, #25013, #22349, #1722 ) ) ;
#26519 = ORIENTED_EDGE ( 'NONE', *, *, #6251, .F. ) ;
#26520 = EDGE_CURVE ( 'NONE', #9824, #27576, #26669, .T. ) ;
#26521 = DIRECTION ( 'NONE',  ( 1.000000000000000000, 1.734723475976807094E-16, 0.000000000000000000 ) ) ;
#26522 = CARTESIAN_POINT ( 'NONE',  ( -38.00000000000000711, -113.9929510916434339, 12.17846912687782179 ) ) ;
#26523 = AXIS2_PLACEMENT_3D ( 'NONE', #26068, #31812, #18484 ) ;
#26524 = CARTESIAN_POINT ( 'NONE',  ( -9.999999999999994671, 0.000000000000000000, 0.000000000000000000 ) ) ;
#26525 = CARTESIAN_POINT ( 'NONE',  ( -37.89983305244309264, -113.9929510916434339, 12.92579853460519423 ) ) ;
#26526 = CARTESIAN_POINT ( 'NONE',  ( -37.93687354226506869, -115.9929510916434481, 12.87038173996323565 ) ) ;
#26527 = CARTESIAN_POINT ( 'NONE',  ( -9.999999999999994671, 0.000000000000000000, 0.000000000000000000 ) ) ;
#26528 = DIRECTION ( 'NONE',  ( 0.000000000000000000, 0.000000000000000000, 1.000000000000000000 ) ) ;
#26529 = ORIENTED_EDGE ( 'NONE', *, *, #6968, .T. ) ;
#26530 = CIRCLE ( 'NONE', #5827, 1.000000000000000888 ) ;
#26531 = DIRECTION ( 'NONE',  ( 0.000000000000000000, -1.000000000000000000, 0.000000000000000000 ) ) ;
#26532 = CARTESIAN_POINT ( 'NONE',  ( 0.000000000000000000, 0.000000000000000000, 0.000000000000000000 ) ) ;
#26533 = CIRCLE ( 'NONE', #34600, 47.49900000000000944 ) ;
#26534 = DIRECTION ( 'NONE',  ( 1.000000000000000000, -0.000000000000000000, -0.000000000000000000 ) ) ;
#26535 = VERTEX_POINT ( 'NONE', #10458 ) ;
#26536 = DIRECTION ( 'NONE',  ( -1.000000000000000000, 0.000000000000000000, -0.000000000000000000 ) ) ;
#26537 = CARTESIAN_POINT ( 'NONE',  ( -35.50000000000000711, -112.0157046079661995, -0.6902086197697556713 ) ) ;
#26538 = CARTESIAN_POINT ( 'NONE',  ( 55.00000000000000000, 10.00000000000000888, -25.00000000000000000 ) ) ;
#26539 = CARTESIAN_POINT ( 'NONE',  ( -35.50000000000000711, -114.2305202833893816, 9.534416457224700991 ) ) ;
#26540 = DIRECTION ( 'NONE',  ( 0.000000000000000000, 0.9048270524660176894, 0.4257792915650767118 ) ) ;
#26541 = ADVANCED_FACE ( 'NONE', ( #23596 ), #13338, .T. ) ;
#26542 = ORIENTED_EDGE ( 'NONE', *, *, #7792, .T. ) ;
#26543 = EDGE_CURVE ( 'NONE', #28617, #18809, #33595, .T. ) ;
#26544 = LINE ( 'NONE', #1877, #18212 ) ;
#26545 = CARTESIAN_POINT ( 'NONE',  ( -34.50000000000000000, -114.8474311500471572, -2.624782352598442614 ) ) ;
#26546 = FACE_OUTER_BOUND ( 'NONE', #9019, .T. ) ;
#26547 = ORIENTED_EDGE ( 'NONE', *, *, #4066, .T. ) ;
#26548 = ORIENTED_EDGE ( 'NONE', *, *, #15258, .F. ) ;
#26549 = CIRCLE ( 'NONE', #8117, 14.00000000000000000 ) ;
#26550 = CARTESIAN_POINT ( 'NONE',  ( -36.94073759706866156, -113.0000000000000000, 8.628524454178448266 ) ) ;
#26551 = DIRECTION ( 'NONE',  ( -1.000000000000000000, -0.000000000000000000, -0.000000000000000000 ) ) ;
#26552 = VERTEX_POINT ( 'NONE', #29719 ) ;
#26553 = VERTEX_POINT ( 'NONE', #10088 ) ;
#26554 = CARTESIAN_POINT ( 'NONE',  ( -35.50000000000000000, -113.3474311500483935, -0.6247823525984269599 ) ) ;
#26555 = CIRCLE ( 'NONE', #5855, 7.020000000000045759 ) ;
#26556 =( GEOMETRIC_REPRESENTATION_CONTEXT ( 3 ) GLOBAL_UNCERTAINTY_ASSIGNED_CONTEXT ( ( #19716 ) ) GLOBAL_UNIT_ASSIGNED_CONTEXT ( ( #26510, #29565, #1844 ) ) REPRESENTATION_CONTEXT ( 'NONE', 'WORKASPACE' ) );
#26557 = CIRCLE ( 'NONE', #8155, 20.00000000000000355 ) ;
#26558 = CARTESIAN_POINT ( 'NONE',  ( 30.00000000000000000, 1.359357947053562196E-14, 0.000000000000000000 ) ) ;
#26559 = DIRECTION ( 'NONE',  ( 1.000000000000000000, -0.000000000000000000, -0.000000000000000000 ) ) ;
#26560 = CARTESIAN_POINT ( 'NONE',  ( -35.50000000000000000, -113.9557924591415627, 10.50182206170499555 ) ) ;
#26561 = LINE ( 'NONE', #1897, #29345 ) ;
#26562 = CARTESIAN_POINT ( 'NONE',  ( -35.80421860361284558, -114.9929510916434339, 14.10650203519841916 ) ) ;
#26563 = DIRECTION ( 'NONE',  ( -1.000000000000000000, 0.000000000000000000, 0.000000000000000000 ) ) ;
#26564 = DIRECTION ( 'NONE',  ( 0.000000000000000000, 0.000000000000000000, -1.000000000000000000 ) ) ;
#26565 = ORIENTED_EDGE ( 'NONE', *, *, #18274, .F. ) ;
#26566 = CARTESIAN_POINT ( 'NONE',  ( -36.50000000000010658, -115.9929510916434481, 13.11852480586264846 ) ) ;
#26567 = CYLINDRICAL_SURFACE ( 'NONE', #15353, 47.49900000000001654 ) ;
#26568 = CARTESIAN_POINT ( 'NONE',  ( 8.000000000000007105, 0.000000000000000000, 0.000000000000000000 ) ) ;
#26569 = DIRECTION ( 'NONE',  ( -1.000000000000000000, 0.000000000000000000, 0.000000000000000000 ) ) ;
#26570 = DIRECTION ( 'NONE',  ( 1.000000000000000000, 0.000000000000000000, 0.000000000000000000 ) ) ;
#26571 = VERTEX_POINT ( 'NONE', #34588 ) ;
#26572 = DIRECTION ( 'NONE',  ( 1.000000000000000000, -5.339440136655842133E-16, -1.047965281155519420E-16 ) ) ;
#26573 = LINE ( 'NONE', #34675, #2650 ) ;
#26574 = LINE ( 'NONE', #12708, #14191 ) ;
#26575 = CARTESIAN_POINT ( 'NONE',  ( 8.000000000000000000, 2.494040418455619523, -18.62763138773847871 ) ) ;
#26576 = VERTEX_POINT ( 'NONE', #9908 ) ;
#26577 = VECTOR ( 'NONE', #13277, 1000.000000000000114 ) ;
#26578 = CARTESIAN_POINT ( 'NONE',  ( -36.64504884055823908, -115.0245472910329880, 4.784774454178448266 ) ) ;
#26579 = CIRCLE ( 'NONE', #3014, 7.199999999999986855 ) ;
#26580 = CARTESIAN_POINT ( 'NONE',  ( 0.000000000000000000, 22.82995208772746665, -41.06517797613640397 ) ) ;
#26581 = DIRECTION ( 'NONE',  ( -1.783119874454246424E-31, -1.187911941725854497E-31, 1.000000000000000000 ) ) ;
#26582 = EDGE_LOOP ( 'NONE', ( #32085, #2196, #15528, #32109 ) ) ;
#26583 = VERTEX_POINT ( 'NONE', #5063 ) ;
#26584 = EDGE_CURVE ( 'NONE', #4328, #25742, #6581, .T. ) ;
#26585 = CARTESIAN_POINT ( 'NONE',  ( -34.49999999999998579, -39.90017302060828541, 86.49999999999991473 ) ) ;
#26586 = VERTEX_POINT ( 'NONE', #31870 ) ;
#26587 = CARTESIAN_POINT ( 'NONE',  ( -39.07941549657749647, -116.1632251905417803, 6.058975545821550845 ) ) ;
#26588 = ORIENTED_EDGE ( 'NONE', *, *, #30655, .T. ) ;
#26589 = CARTESIAN_POINT ( 'NONE',  ( 0.000000000000000000, 0.000000000000000000, 0.000000000000000000 ) ) ;
#26591 = ORIENTED_EDGE ( 'NONE', *, *, #12357, .T. ) ;
#26590 = AXIS2_PLACEMENT_3D ( 'NONE', #13412, #24394, #19152 ) ;
#26592 = ORIENTED_EDGE ( 'NONE', *, *, #10155, .T. ) ;
#26593 = CYLINDRICAL_SURFACE ( 'NONE', #2817, 4.000000000000000000 ) ;
#26594 = EDGE_CURVE ( 'NONE', #27346, #13312, #23846, .T. ) ;
#26595 = DIRECTION ( 'NONE',  ( 1.000000000000000000, -5.339440136655842133E-16, -1.047965281155519420E-16 ) ) ;
#26596 = VERTEX_POINT ( 'NONE', #15475 ) ;
#26597 = VERTEX_POINT ( 'NONE', #32059 ) ;
#26598 = CARTESIAN_POINT ( 'NONE',  ( 0.000000000000000000, 0.000000000000000000, 0.000000000000000000 ) ) ;
#26599 = AXIS2_PLACEMENT_3D ( 'NONE', #9938, #4379, #7235 ) ;
#26600 = DIRECTION ( 'NONE',  ( -1.000000000000000000, 0.000000000000000000, 0.000000000000000000 ) ) ;
#26601 = AXIS2_PLACEMENT_3D ( 'NONE', #24252, #35239, #30012 ) ;
#26602 = ORIENTED_EDGE ( 'NONE', *, *, #1583, .F. ) ;
#26603 = CIRCLE ( 'NONE', #20234, 4.800000000000000711 ) ;
#26604 = CARTESIAN_POINT ( 'NONE',  ( 0.000000000000000000, 0.000000000000000000, 0.000000000000000000 ) ) ;
#26605 = FACE_OUTER_BOUND ( 'NONE', #29283, .T. ) ;
#26606 = DIRECTION ( 'NONE',  ( -1.000000000000000000, 0.000000000000000000, 0.000000000000000000 ) ) ;
#26607 = SHAPE_REPRESENTATION ( 'BR-594', ( #12649, #21310, #25287, #29896, #5180, #20660, #18437, #23645, #28729, #2309, #30533, #22388, #6877, #6956, #1208, #9243, #19579, #2947, #27022, #29386, #27096, #11557, #13847, #31674, #16141, #31596, #5810, #16060, #10418, #627, #33979, #23034, #5257, #14988, #7523, #13299, #33400, #25935, #27665, #32256, #16707 ), #13240 ) ;
#26608 = CARTESIAN_POINT ( 'NONE',  ( -34.50000000000000000, -115.9929510916434481, 12.17846912687782712 ) ) ;
#26609 = DIRECTION ( 'NONE',  ( 0.000000000000000000, 0.000000000000000000, 1.000000000000000000 ) ) ;
#26610 = CARTESIAN_POINT ( 'NONE',  ( -37.88768952767750164, -115.9754527089670262, 7.972274454178450043 ) ) ;
#26611 = CARTESIAN_POINT ( 'NONE',  ( -34.50000000000000000, -114.5266723804073195, 8.577838247824468354 ) ) ;
#26612 = DIRECTION ( 'NONE',  ( 0.000000000000000000, -0.9510565162951502005, -0.3090169943749580539 ) ) ;
#26613 = CARTESIAN_POINT ( 'NONE',  ( 0.000000000000000000, -49.65209126885753221, -15.44894276735603356 ) ) ;
#26614 = VECTOR ( 'NONE', #4386, 1000.000000000000000 ) ;
#26615 = AXIS2_PLACEMENT_3D ( 'NONE', #22244, #634, #6561 ) ;
#26616 = CARTESIAN_POINT ( 'NONE',  ( 0.000000000000000000, 11.90021268425617329, -45.45261810511203038 ) ) ;
#26617 = DIRECTION ( 'NONE',  ( 1.000000000000000000, 0.000000000000000000, 0.000000000000000000 ) ) ;
#26618 = CARTESIAN_POINT ( 'NONE',  ( 4.000000000000003553, -35.11945359308137427, 38.34871548466002622 ) ) ;
#26619 = DIRECTION ( 'NONE',  ( -1.000000000000000000, 0.000000000000000000, 0.000000000000000000 ) ) ;
#26620 = ORIENTED_EDGE ( 'NONE', *, *, #5723, .T. ) ;
#26621 = AXIS2_PLACEMENT_3D ( 'NONE', #18841, #32709, #4996 ) ;
#26622 = CARTESIAN_POINT ( 'NONE',  ( -36.94073759706868287, -115.9999999999999858, 2.871475545821551290 ) ) ;
#26623 = DIRECTION ( 'NONE',  ( 1.000000000000000000, 0.000000000000000000, 0.000000000000000000 ) ) ;
#26624 = CARTESIAN_POINT ( 'NONE',  ( -35.50000000000000000, -113.0140978167138712, 0.8127176474015720409 ) ) ;
#26625 = VERTEX_POINT ( 'NONE', #26491 ) ;
#26626 = ORIENTED_EDGE ( 'NONE', *, *, #24730, .T. ) ;
#26627 = AXIS2_PLACEMENT_3D ( 'NONE', #21489, #32482, #7815 ) ;
#26628 = EDGE_CURVE ( 'NONE', #27701, #16891, #14618, .T. ) ;
#26629 = DIRECTION ( 'NONE',  ( -1.000000000000000000, 0.000000000000000000, 0.000000000000000000 ) ) ;
#26630 = VECTOR ( 'NONE', #25763, 999.9999999999998863 ) ;
#26631 = FACE_OUTER_BOUND ( 'NONE', #6774, .T. ) ;
#26632 = ORIENTED_EDGE ( 'NONE', *, *, #5249, .F. ) ;
#26633 = EDGE_CURVE ( 'NONE', #20288, #13349, #31315, .T. ) ;
#26634 = ORIENTED_EDGE ( 'NONE', *, *, #27732, .T. ) ;
#26635 = ORIENTED_EDGE ( 'NONE', *, *, #3903, .F. ) ;
#26636 = DIRECTION ( 'NONE',  ( -1.000000000000000000, 0.000000000000000000, 0.000000000000000000 ) ) ;
#26637 = CARTESIAN_POINT ( 'NONE',  ( -35.62769128460905677, -112.5438815906447729, 9.808975545821551734 ) ) ;
#26638 = EDGE_CURVE ( 'NONE', #31912, #14640, #20940, .T. ) ;
#26639 = DIRECTION ( 'NONE',  ( 0.000000000000000000, 0.000000000000000000, -1.000000000000000000 ) ) ;
#26640 = EDGE_CURVE ( 'NONE', #22316, #10719, #22123, .T. ) ;
#26641 = CARTESIAN_POINT ( 'NONE',  ( 0.000000000000000000, -17.47118961583598917, -0.9861715913089493801 ) ) ;
#26642 = VERTEX_POINT ( 'NONE', #2723 ) ;
#26643 = ORIENTED_EDGE ( 'NONE', *, *, #34888, .T. ) ;
#26644 = AXIS2_PLACEMENT_3D ( 'NONE', #35110, #13315, #11136 ) ;
#26645 = CARTESIAN_POINT ( 'NONE',  ( -35.50000000000000711, -112.0460568841087223, -0.8839717462762063382 ) ) ;
#26646 = CARTESIAN_POINT ( 'NONE',  ( 8.000000000000000000, 10.62435788049461571, -13.16139124467909483 ) ) ;
#26647 = CARTESIAN_POINT ( 'NONE',  ( 0.000000000000000000, 0.000000000000000000, 0.000000000000000000 ) ) ;
#26648 = ORIENTED_EDGE ( 'NONE', *, *, #9664, .F. ) ;
#26649 = PLANE ( 'NONE',  #28724 ) ;
#26650 = CARTESIAN_POINT ( 'NONE',  ( 0.000000000000000000, 0.000000000000000000, 0.000000000000000000 ) ) ;
#26651 = VECTOR ( 'NONE', #24532, 1000.000000000000000 ) ;
#26652 = CARTESIAN_POINT ( 'NONE',  ( -34.50000000000000000, -114.9912366357066986, 10.44580456020104720 ) ) ;
#26653 = VECTOR ( 'NONE', #27671, 1000.000000000000000 ) ;
#26654 = CARTESIAN_POINT ( 'NONE',  ( -1.498621416870293155, -4.871103520542888323E-16, -7.020000000000045759 ) ) ;
#26655 = CARTESIAN_POINT ( 'NONE',  ( -36.50000000000011369, -114.9929510916434339, 13.11852480586264669 ) ) ;
#26656 = DIRECTION ( 'NONE',  ( 0.000000000000000000, -0.5877852522924621459, -0.8090169943749555559 ) ) ;
#26657 = CARTESIAN_POINT ( 'NONE',  ( -34.50000000000000000, -114.8211182053456838, 9.932864235516914775 ) ) ;
#26658 = LINE ( 'NONE', #1812, #11870 ) ;
#26659 = ADVANCED_FACE ( 'NONE', ( #2543 ), #14201, .T. ) ;
#26660 = CARTESIAN_POINT ( 'NONE',  ( -38.00000000000000711, -114.9929510916434339, 10.50625754673587231 ) ) ;
#26661 = CARTESIAN_POINT ( 'NONE',  ( 7.999999999999992895, 0.000000000000000000, 0.000000000000000000 ) ) ;
#26662 = ORIENTED_EDGE ( 'NONE', *, *, #27146, .F. ) ;
#26663 = DIRECTION ( 'NONE',  ( -1.000000000000000000, 0.000000000000000000, 0.000000000000000000 ) ) ;
#26664 = DIRECTION ( 'NONE',  ( 0.000000000000000000, 0.000000000000000000, 1.000000000000000000 ) ) ;
#26665 = ORIENTED_EDGE ( 'NONE', *, *, #1005, .F. ) ;
#26666 = CARTESIAN_POINT ( 'NONE',  ( -37.43749999999998579, -114.9929510916434339, 13.11852480586264669 ) ) ;
#26667 = ORIENTED_EDGE ( 'NONE', *, *, #15610, .T. ) ;
#26668 = CARTESIAN_POINT ( 'NONE',  ( -35.54388159064475872, -112.6276912846090568, 7.316024454178449155 ) ) ;
#26669 = LINE ( 'NONE', #1644, #10638 ) ;
#26670 = ORIENTED_EDGE ( 'NONE', *, *, #30199, .T. ) ;
#26671 = AXIS2_PLACEMENT_3D ( 'NONE', #7335, #18485, #17766 ) ;
#26672 = VERTEX_POINT ( 'NONE', #25203 ) ;
#26673 = AXIS2_PLACEMENT_3D ( 'NONE', #18618, #5312, #35375 ) ;
#26674 = ADVANCED_FACE ( 'NONE', ( #16359, #19241, #525, #16548, #13508, #13857 ), #8265, .F. ) ;
#26675 = CARTESIAN_POINT ( 'NONE',  ( 50.00000000000000000, 20.00000000000001776, 120.0000000000000000 ) ) ;
#26676 = ADVANCED_FACE ( 'NONE', ( #30247 ), #17499, .T. ) ;
#26677 = EDGE_CURVE ( 'NONE', #33126, #5490, #3066, .T. ) ;
#26678 = ORIENTED_EDGE ( 'NONE', *, *, #8352, .T. ) ;
#26679 = CARTESIAN_POINT ( 'NONE',  ( -39.07941549657748936, -111.8367748094582055, 3.941024454178448710 ) ) ;
#26680 = CARTESIAN_POINT ( 'NONE',  ( 7.999999999999992895, 13.85708833600033074, -45.43276465116652219 ) ) ;
#26681 = CIRCLE ( 'NONE', #32989, 20.00000000000000711 ) ;
#26682 = DIRECTION ( 'NONE',  ( 0.000000000000000000, 0.8660254037844350439, 0.5000000000000061062 ) ) ;
#26683 = CIRCLE ( 'NONE', #17444, 8.000000000000015987 ) ;
#26684 = ORIENTED_EDGE ( 'NONE', *, *, #27912, .T. ) ;
#26685 = ORIENTED_EDGE ( 'NONE', *, *, #18288, .T. ) ;
#26686 = DIRECTION ( 'NONE',  ( 1.000000000000000000, 0.000000000000000000, 0.000000000000000000 ) ) ;
#26687 = ADVANCED_FACE ( 'NONE', ( #30071 ), #24666, .T. ) ;
#26688 = EDGE_CURVE ( 'NONE', #5984, #26597, #30174, .T. ) ;
#26689 = DIRECTION ( 'NONE',  ( -1.783119874454246424E-31, -1.187911941725854497E-31, 1.000000000000000000 ) ) ;
#26690 = ORIENTED_EDGE ( 'NONE', *, *, #24708, .F. ) ;
#26691 = ORIENTED_EDGE ( 'NONE', *, *, #30376, .T. ) ;
#26692 = CARTESIAN_POINT ( 'NONE',  ( -34.50000000000000000, -112.4957190293567066, -2.560864217808777266 ) ) ;
#26693 = CARTESIAN_POINT ( 'NONE',  ( -9.999999999999994671, 0.000000000000000000, 0.000000000000000000 ) ) ;
#26694 = VERTEX_POINT ( 'NONE', #19430 ) ;
#26695 = EDGE_LOOP ( 'NONE', ( #25818, #15843, #7892, #3031 ) ) ;
#26696 = CARTESIAN_POINT ( 'NONE',  ( 0.000000000000000000, 0.000000000000000000, -1.200000000000006617 ) ) ;
#26697 = CARTESIAN_POINT ( 'NONE',  ( -38.00000000000000711, -113.9929510916434339, 12.57451923796417681 ) ) ;
#26698 = FACE_OUTER_BOUND ( 'NONE', #27827, .T. ) ;
#26699 = CARTESIAN_POINT ( 'NONE',  ( -3.413765605486555721, -14.29811891091961584, -1.200000000000006617 ) ) ;
#26700 = CARTESIAN_POINT ( 'NONE',  ( -34.50000000000000000, -113.9697269463297431, 10.50348536859153370 ) ) ;
#26701 = EDGE_CURVE ( 'NONE', #22664, #8972, #18663, .T. ) ;
#26702 = CARTESIAN_POINT ( 'NONE',  ( -37.75185693410092824, -115.9929510916434481, 13.05539834812634759 ) ) ;
#26703 = CARTESIAN_POINT ( 'NONE',  ( 3.799999999999999822, 4.382607293638566128E-16, 45.00000000000000000 ) ) ;
#26705 = AXIS2_PLACEMENT_3D ( 'NONE', #6285, #19759, #28256 ) ;
#26704 = DIRECTION ( 'NONE',  ( 0.000000000000000000, 1.000000000000000000, 0.000000000000000000 ) ) ;
#26706 = VECTOR ( 'NONE', #21943, 1000.000000000000000 ) ;
#26707 = EDGE_CURVE ( 'NONE', #18809, #16586, #27726, .T. ) ;
#26708 = ORIENTED_EDGE ( 'NONE', *, *, #3146, .F. ) ;
#26709 = DIRECTION ( 'NONE',  ( -1.000000000000000000, 0.000000000000000000, 0.000000000000000000 ) ) ;
#26710 = CARTESIAN_POINT ( 'NONE',  ( 27.00000000000001066, 1.304248841091931379E-14, 0.000000000000000000 ) ) ;
#26711 = LINE ( 'NONE', #18937, #1347 ) ;
#26712 = ORIENTED_EDGE ( 'NONE', *, *, #20613, .T. ) ;
#26713 = CARTESIAN_POINT ( 'NONE',  ( 8.000000000000007105, -1.111908866155156161, 9.433698091065117808 ) ) ;
#26714 = CARTESIAN_POINT ( 'NONE',  ( -35.50000000000000711, -112.0414288467712112, 1.115164475686276191 ) ) ;
#26715 = DIRECTION ( 'NONE',  ( -1.000000000000000000, 0.000000000000000000, 0.000000000000000000 ) ) ;
#26716 = ADVANCED_FACE ( 'NONE', ( #5586 ), #30766, .T. ) ;
#26717 = EDGE_CURVE ( 'NONE', #16271, #9394, #8381, .T. ) ;
#26718 = CARTESIAN_POINT ( 'NONE',  ( -35.50000000000000711, -114.1068310684433129, 9.512752019463897923 ) ) ;
#26719 = CARTESIAN_POINT ( 'NONE',  ( 4.000000000000003553, -36.06787431788650622, -37.45808914225528952 ) ) ;
#26720 = ORIENTED_EDGE ( 'NONE', *, *, #30376, .F. ) ;
#26721 = DIRECTION ( 'NONE',  ( 1.226634733346697831E-16, -0.7071067811865466846, -0.7071067811865483499 ) ) ;
#26722 = CARTESIAN_POINT ( 'NONE',  ( -35.50000000000000000, -111.0140978167138570, 0.0002176474015660057743 ) ) ;
#26723 = CARTESIAN_POINT ( 'NONE',  ( -1.479000000000008530, 9.623377526722998283E-16, 5.016000000000010672 ) ) ;
#26724 = ORIENTED_EDGE ( 'NONE', *, *, #15574, .T. ) ;
#26725 = VERTEX_POINT ( 'NONE', #35479 ) ;
#26726 = CARTESIAN_POINT ( 'NONE',  ( -36.94073759706866156, -113.0000000000000000, 7.128524454178450043 ) ) ;
#26727 = LINE ( 'NONE', #27255, #33074 ) ;
#26728 = ORIENTED_EDGE ( 'NONE', *, *, #27311, .T. ) ;
#26729 = EDGE_LOOP ( 'NONE', ( #31884, #8442, #27761, #23545, #11468, #27733, #1701, #25414, #24503, #8184, #24887, #9926, #9952, #12999, #23696, #18061, #29409, #5558, #2633, #14865, #15313, #23115, #14258, #9829, #18289, #20335, #34860, #11894, #8234, #8596, #356, #2378, #24292, #4551, #24352, #27114, #32200, #11827, #29332, #5022, #37, #14511, #18558, #27174, #24938, #20299, #19001, #11393, #12312, #25948, #13781, #15140, #2297, #34589, #25692, #33054, #11571, #27130, #20419, #23460, #11118, #17738, #4696, #16623, #20734, #11757, #18282, #33797, #760, #1025, #26772, #28672, #6505, #33443, #32458, #15609, #31043, #31493, #10, #10302, #30089, #25968, #13693, #9923, #3835 ) ) ;
#26730 = CARTESIAN_POINT ( 'NONE',  ( -34.50000000000000000, -115.0140978167138712, -0.6247823525984418369 ) ) ;
#26731 = AXIS2_PLACEMENT_3D ( 'NONE', #6949, #23151, #12539 ) ;
#26732 = CIRCLE ( 'NONE', #23258, 7.200000000000000178 ) ;
#26733 = DIRECTION ( 'NONE',  ( -1.000000000000000000, -1.836970198721029934E-16, -0.000000000000000000 ) ) ;
#26734 = AXIS2_PLACEMENT_3D ( 'NONE', #9510, #23010, #20470 ) ;
#26735 = CARTESIAN_POINT ( 'NONE',  ( 7.999999999999992895, 32.00046193115196758, -34.40241257139653186 ) ) ;
#26736 = CARTESIAN_POINT ( 'NONE',  ( -37.50818044754229419, -114.9929510916434339, 13.11847460610629668 ) ) ;
#26737 = DIRECTION ( 'NONE',  ( 0.000000000000000000, 0.000000000000000000, 1.000000000000000000 ) ) ;
#26738 = LINE ( 'NONE', #16073, #19373 ) ;
#26739 = CARTESIAN_POINT ( 'NONE',  ( -34.50000000000000000, -112.0140978167138712, 0.7502176474015694874 ) ) ;
#26740 = EDGE_CURVE ( 'NONE', #11716, #24732, #27874, .T. ) ;
#26741 = CARTESIAN_POINT ( 'NONE',  ( -34.50015059926905536, -114.9929510916434339, 12.64306614848962695 ) ) ;
#26742 = DIRECTION ( 'NONE',  ( 1.000000000000000000, -0.000000000000000000, 0.000000000000000000 ) ) ;
#26743 = EDGE_CURVE ( 'NONE', #19072, #542, #2582, .T. ) ;
#26744 = DIRECTION ( 'NONE',  ( -1.000000000000000000, 0.000000000000000000, -0.000000000000000000 ) ) ;
#26745 = VERTEX_POINT ( 'NONE', #26083 ) ;
#26746 = CARTESIAN_POINT ( 'NONE',  ( -35.50100302244945993, -115.9929510916434481, 12.65121853911337446 ) ) ;
#26747 = CARTESIAN_POINT ( 'NONE',  ( -35.50000000000000711, -114.9307644833806137, -1.624782352598427959 ) ) ;
#26748 = CARTESIAN_POINT ( 'NONE',  ( 7.999999999999992895, -42.60732521687585006, 19.80331771201643321 ) ) ;
#26749 = DIRECTION ( 'NONE',  ( 1.000000000000000000, -0.000000000000000000, -0.000000000000000000 ) ) ;
#26750 = DIRECTION ( 'NONE',  ( 0.000000000000000000, 0.000000000000000000, 1.000000000000000000 ) ) ;
#26751 = EDGE_LOOP ( 'NONE', ( #26221, #12988 ) ) ;
#26752 = DIRECTION ( 'NONE',  ( 0.000000000000000000, 4.163336342344333240E-14, -1.000000000000000000 ) ) ;
#26753 = CARTESIAN_POINT ( 'NONE',  ( 0.2142857142857085284, -10.49781318335649161, 0.000000000000000000 ) ) ;
#26754 = AXIS2_PLACEMENT_3D ( 'NONE', #34904, #21722, #29663 ) ;
#26755 = FACE_OUTER_BOUND ( 'NONE', #10449, .T. ) ;
#26756 = CARTESIAN_POINT ( 'NONE',  ( -34.49999999999998579, -25.98076211353322051, 84.99999999999992895 ) ) ;
#26757 = CARTESIAN_POINT ( 'NONE',  ( -37.05926240293133134, -115.0000000000000000, 7.878524454178450043 ) ) ;
#26758 = DIRECTION ( 'NONE',  ( -1.000000000000000000, -0.000000000000000000, -0.000000000000000000 ) ) ;
#26759 = CYLINDRICAL_SURFACE ( 'NONE', #29149, 15.49899999999998457 ) ;
#26760 = VERTEX_POINT ( 'NONE', #9334 ) ;
#26761 = ORIENTED_EDGE ( 'NONE', *, *, #9286, .T. ) ;
#26762 = AXIS2_PLACEMENT_3D ( 'NONE', #7447, #19901, #31268 ) ;
#26763 = FACE_OUTER_BOUND ( 'NONE', #4148, .T. ) ;
#26764 = FACE_OUTER_BOUND ( 'NONE', #8144, .T. ) ;
#26765 = DIRECTION ( 'NONE',  ( 0.000000000000000000, -0.8443279255020087470, -0.5358267949790065376 ) ) ;
#26766 = VERTEX_POINT ( 'NONE', #14372 ) ;
#26767 = CARTESIAN_POINT ( 'NONE',  ( -38.37230871539094323, -115.4561184093552413, 4.558975545821550845 ) ) ;
#26768 = ORIENTED_EDGE ( 'NONE', *, *, #5148, .T. ) ;
#26769 = SURFACE_STYLE_USAGE ( .BOTH. , #8365 ) ;
#26770 = VECTOR ( 'NONE', #34218, 1000.000000000000000 ) ;
#26771 = VERTEX_POINT ( 'NONE', #12216 ) ;
#26772 = ORIENTED_EDGE ( 'NONE', *, *, #16990, .F. ) ;
#26773 = CARTESIAN_POINT ( 'NONE',  ( 8.000000000000007105, -7.613867765417476008, -5.679790370316101011 ) ) ;
#26774 = CARTESIAN_POINT ( 'NONE',  ( 0.000000000000000000, 0.000000000000000000, 0.000000000000000000 ) ) ;
#26775 = ORIENTED_EDGE ( 'NONE', *, *, #2696, .F. ) ;
#26776 = ORIENTED_EDGE ( 'NONE', *, *, #17452, .F. ) ;
#26777 = VECTOR ( 'NONE', #14821, 1000.000000000000000 ) ;
#26778 = DIRECTION ( 'NONE',  ( -1.000000000000000000, 0.000000000000000000, 0.000000000000000000 ) ) ;
#26779 = DIRECTION ( 'NONE',  ( 1.000000000000000000, 0.000000000000000000, 0.000000000000000000 ) ) ;
#26780 = VERTEX_POINT ( 'NONE', #17422 ) ;
#26781 = DIRECTION ( 'NONE',  ( -1.000000000000000000, 0.000000000000000000, 0.000000000000000000 ) ) ;
#26782 = DIRECTION ( 'NONE',  ( 0.000000000000000000, 0.000000000000000000, 1.000000000000000000 ) ) ;
#26783 = CARTESIAN_POINT ( 'NONE',  ( 50.00000000000000711, -2.775557561562891351E-14, 110.0000000000000000 ) ) ;
#26784 = EDGE_CURVE ( 'NONE', #21338, #1167, #8301, .T. ) ;
#26785 = CARTESIAN_POINT ( 'NONE',  ( -4.000000000000000000, 0.000000000000000000, -34.40000000000000568 ) ) ;
#26786 = CARTESIAN_POINT ( 'NONE',  ( -36.11231047232249836, -112.0245472910329880, 5.722274454178448266 ) ) ;
#26787 = CARTESIAN_POINT ( 'NONE',  ( -34.50000306791346816, -115.9929510916434481, 12.62875129555796150 ) ) ;
#26788 = DIRECTION ( 'NONE',  ( 1.000000000000000000, 0.000000000000000000, 0.000000000000000000 ) ) ;
#26789 = PLANE ( 'NONE',  #12117 ) ;
#26790 = CIRCLE ( 'NONE', #11255, 0.6000000000000028644 ) ;
#26791 = CARTESIAN_POINT ( 'NONE',  ( 8.000000000000000000, -6.860320204751237938, 13.89802171851381551 ) ) ;
#26792 = DIRECTION ( 'NONE',  ( 0.000000000000000000, -1.000000000000000000, -1.040834085586082363E-14 ) ) ;
#26793 = CARTESIAN_POINT ( 'NONE',  ( -50.00000000000000000, 0.000000000000000000, 81.00000000000001421 ) ) ;
#26794 = CARTESIAN_POINT ( 'NONE',  ( -34.49999999999998579, -24.48076211353304998, 71.08058909292489602 ) ) ;
#26795 = VERTEX_POINT ( 'NONE', #33828 ) ;
#26796 = EDGE_CURVE ( 'NONE', #8680, #10339, #34774, .T. ) ;
#26797 = CARTESIAN_POINT ( 'NONE',  ( -39.16322519054178741, -111.9205845034225177, 9.433975545821549957 ) ) ;
#26798 = CARTESIAN_POINT ( 'NONE',  ( -39.49999999999999289, -12.31102132296306451, 91.23752798680880005 ) ) ;
#26799 = CARTESIAN_POINT ( 'NONE',  ( 4.000000000000000000, 19.60123832284017453, 3.973846525876501889 ) ) ;
#26800 = ORIENTED_EDGE ( 'NONE', *, *, #20212, .T. ) ;
#26801 = VERTEX_POINT ( 'NONE', #17070 ) ;
#26802 = DIRECTION ( 'NONE',  ( -1.000000000000000000, 0.000000000000000000, 0.000000000000000000 ) ) ;
#26803 = VECTOR ( 'NONE', #969, 1000.000000000000000 ) ;
#26804 = CARTESIAN_POINT ( 'NONE',  ( 0.000000000000000000, 46.77034588191304465, 22.72740077717245910 ) ) ;
#26805 = ORIENTED_EDGE ( 'NONE', *, *, #16599, .T. ) ;
#26806 = EDGE_LOOP ( 'NONE', ( #31254, #22917, #13409, #29519 ) ) ;
#26807 = ORIENTED_EDGE ( 'NONE', *, *, #17134, .F. ) ;
#26808 = VECTOR ( 'NONE', #14109, 1000.000000000000000 ) ;
#26809 = VECTOR ( 'NONE', #31436, 1000.000000000000114 ) ;
#26810 = CARTESIAN_POINT ( 'NONE',  ( 0.000000000000000000, -51.19683565102439360, -9.104066087303991139 ) ) ;
#26811 = CARTESIAN_POINT ( 'NONE',  ( 0.000000000000000000, 10.58300524425836109, -3.000000000000002665 ) ) ;
#26812 = CIRCLE ( 'NONE', #7266, 20.00000000000000355 ) ;
#26813 = DIRECTION ( 'NONE',  ( -6.852157730108388023E-17, 0.9999951783811291683, 0.003105352555455980282 ) ) ;
#26814 = DIRECTION ( 'NONE',  ( 0.000000000000000000, 0.000000000000000000, -1.000000000000000000 ) ) ;
#26815 = EDGE_CURVE ( 'NONE', #13426, #22165, #9691, .T. ) ;
#26817 = ORIENTED_EDGE ( 'NONE', *, *, #9918, .F. ) ;
#26816 = CIRCLE ( 'NONE', #25083, 4.800000000000006040 ) ;
#26818 = ORIENTED_EDGE ( 'NONE', *, *, #31954, .F. ) ;
#26819 = CARTESIAN_POINT ( 'NONE',  ( -35.50000000000000711, -112.0414288467712112, 1.115164475686276191 ) ) ;
#26820 = CARTESIAN_POINT ( 'NONE',  ( 0.000000000000000000, -2.710505431213761085E-17, -30.90000000000000568 ) ) ;
#26821 = DIRECTION ( 'NONE',  ( 0.000000000000000000, 1.000000000000000000, 0.000000000000000000 ) ) ;
#26822 = VERTEX_POINT ( 'NONE', #9152 ) ;
#26823 = CARTESIAN_POINT ( 'NONE',  ( 8.000000000000000000, -16.59870953437682672, 3.253005020243791456 ) ) ;
#26824 = DIRECTION ( 'NONE',  ( -1.000000000000000000, 0.000000000000000000, 0.000000000000000000 ) ) ;
#26825 = EDGE_CURVE ( 'NONE', #19482, #23782, #19223, .T. ) ;
#26826 = CARTESIAN_POINT ( 'NONE',  ( -34.68937937320795584, -114.9929510916434339, 13.37409560816408671 ) ) ;
#26827 = EDGE_CURVE ( 'NONE', #14470, #10703, #30251, .T. ) ;
#26828 = DIRECTION ( 'NONE',  ( -1.000000000000000000, -0.000000000000000000, 0.000000000000000000 ) ) ;
#26829 = CARTESIAN_POINT ( 'NONE',  ( -37.99899697755054717, -114.9929510916434339, 12.65121853911336736 ) ) ;
#26830 = DIRECTION ( 'NONE',  ( 0.000000000000000000, 0.000000000000000000, 1.000000000000000000 ) ) ;
#26831 = CARTESIAN_POINT ( 'NONE',  ( -34.50000000000000000, -114.1091535596544873, 9.513028657562415447 ) ) ;
#26832 = DIRECTION ( 'NONE',  ( 0.000000000000000000, 0.000000000000000000, 1.000000000000000000 ) ) ;
#26833 = AXIS2_PLACEMENT_3D ( 'NONE', #11185, #3274, #554 ) ;
#26834 = CARTESIAN_POINT ( 'NONE',  ( -37.62959469683911351, -114.9929510916434339, 13.10254527216511633 ) ) ;
#26835 = CARTESIAN_POINT ( 'NONE',  ( -42.49999999999999289, -35.77980021920998155, 98.97243186433534845 ) ) ;
#26836 = ORIENTED_EDGE ( 'NONE', *, *, #31724, .T. ) ;
#26837 = AXIS2_PLACEMENT_3D ( 'NONE', #25290, #11765, #11592 ) ;
#26838 = CARTESIAN_POINT ( 'NONE',  ( 0.000000000000000000, -2.710505431213761085E-17, -45.89999999999999858 ) ) ;
#26839 = DIRECTION ( 'NONE',  ( -1.000000000000000000, 0.000000000000000000, -0.000000000000000000 ) ) ;
#26840 = ORIENTED_EDGE ( 'NONE', *, *, #15896, .T. ) ;
#26841 = CIRCLE ( 'NONE', #19902, 15.49899999999998279 ) ;
#26842 = CARTESIAN_POINT ( 'NONE',  ( -37.75185693410092824, -114.9929510916434339, 13.05539834812634581 ) ) ;
#26843 = VERTEX_POINT ( 'NONE', #23369 ) ;
#26844 = EDGE_CURVE ( 'NONE', #15127, #21342, #2013, .T. ) ;
#26845 = CARTESIAN_POINT ( 'NONE',  ( -40.02454729103296671, -115.1833782841879525, 2.159774454178448710 ) ) ;
#26846 = COLOUR_RGB ( '', 0.72549020, 0.75294118, 0.79215686) ;
#26847 = CARTESIAN_POINT ( 'NONE',  ( -37.49999999999999289, -10.15468310254180651, 112.5137715831613008 ) ) ;
#26848 = AXIS2_PLACEMENT_3D ( 'NONE', #25500, #33583, #815 ) ;
#26849 = VERTEX_POINT ( 'NONE', #28423 ) ;
#26850 = VERTEX_POINT ( 'NONE', #3422 ) ;
#26851 = CARTESIAN_POINT ( 'NONE',  ( 0.000000000000000000, -8.605879768205133118, -12.89022243466717299 ) ) ;
#26852 = ORIENTED_EDGE ( 'NONE', *, *, #9094, .F. ) ;
#26853 = CARTESIAN_POINT ( 'NONE',  ( -34.00000000000000000, -114.0592624029313242, 4.503524454178447378 ) ) ;
#26854 = AXIS2_PLACEMENT_3D ( 'NONE', #22114, #2881, #13845 ) ;
#26855 = DIRECTION ( 'NONE',  ( -1.000000000000000000, 0.000000000000000000, 0.000000000000000000 ) ) ;
#26856 = CIRCLE ( 'NONE', #19349, 20.00000000000000711 ) ;
#26857 = CARTESIAN_POINT ( 'NONE',  ( 1.498621416870293821, 0.000000000000000000, 0.000000000000000000 ) ) ;
#26858 = VERTEX_POINT ( 'NONE', #25736 ) ;
#26859 = ORIENTED_EDGE ( 'NONE', *, *, #22905, .F. ) ;
#26860 = DIRECTION ( 'NONE',  ( -1.000000000000000000, -0.000000000000000000, -0.000000000000000000 ) ) ;
#26861 = EDGE_CURVE ( 'NONE', #17954, #2086, #7154, .T. ) ;
#26862 = AXIS2_PLACEMENT_3D ( 'NONE', #34858, #24059, #9998 ) ;
#26863 = SURFACE_STYLE_USAGE ( .BOTH. , #4898 ) ;
#26864 = DIRECTION ( 'NONE',  ( -1.000000000000000000, 5.339440136655834244E-16, 0.000000000000000000 ) ) ;
#26865 = ORIENTED_EDGE ( 'NONE', *, *, #28230, .F. ) ;
#26866 = ORIENTED_EDGE ( 'NONE', *, *, #30407, .F. ) ;
#26867 = CARTESIAN_POINT ( 'NONE',  ( -34.50000000000000000, -112.8230659962028994, 2.866612799894348029 ) ) ;
#26868 = AXIS2_PLACEMENT_3D ( 'NONE', #23247, #31544, #25797 ) ;
#26869 = AXIS2_PLACEMENT_3D ( 'NONE', #24277, #15969, #21201 ) ;
#26870 = VECTOR ( 'NONE', #12178, 1000.000000000000000 ) ;
#26871 = PLANE ( 'NONE',  #20782 ) ;
#26872 = ORIENTED_EDGE ( 'NONE', *, *, #28690, .T. ) ;
#26873 = AXIS2_PLACEMENT_3D ( 'NONE', #7404, #2208, #4725 ) ;
#26874 = CARTESIAN_POINT ( 'NONE',  ( -35.50000000000000711, -114.1302255537607095, 9.515717283514957714 ) ) ;
#26875 = EDGE_CURVE ( 'NONE', #5458, #192, #11748, .T. ) ;
#26876 = CARTESIAN_POINT ( 'NONE',  ( -34.50000000000000000, -113.9929510916434339, 10.53376102667243508 ) ) ;
#26877 = EDGE_CURVE ( 'NONE', #19237, #33648, #30944, .T. ) ;
#26878 = DIRECTION ( 'NONE',  ( 0.000000000000000000, 0.000000000000000000, 1.000000000000000000 ) ) ;
#26879 = CARTESIAN_POINT ( 'NONE',  ( 0.000000000000000000, -2.710505431213761085E-17, 29.09999999999999787 ) ) ;
#26880 = EDGE_CURVE ( 'NONE', #14579, #4101, #12923, .T. ) ;
#26881 = CARTESIAN_POINT ( 'NONE',  ( -37.50613590685470911, -113.9929510916434339, 13.11852378322482515 ) ) ;
#26882 = CARTESIAN_POINT ( 'NONE',  ( -35.95915003344518368, -115.9929510916434481, 13.11692036158763308 ) ) ;
#26883 = AXIS2_PLACEMENT_3D ( 'NONE', #24576, #13242, #16084 ) ;
#26884 = DIRECTION ( 'NONE',  ( 0.000000000000000000, 0.000000000000000000, 1.000000000000000000 ) ) ;
#26885 = DIRECTION ( 'NONE',  ( -1.000000000000000000, 0.000000000000000000, 0.000000000000000000 ) ) ;
#26886 = VECTOR ( 'NONE', #952, 1000.000000000000000 ) ;
#26887 = VERTEX_POINT ( 'NONE', #866 ) ;
#26888 = EDGE_CURVE ( 'NONE', #23561, #29894, #23929, .T. ) ;
#26889 = CARTESIAN_POINT ( 'NONE',  ( -1.519999999999993578, 0.000000000000000000, 0.000000000000000000 ) ) ;
#26890 = CARTESIAN_POINT ( 'NONE',  ( 1.799999999999996492, -2.914335439641035426E-16, -4.200000000000014388 ) ) ;
#26891 = DIRECTION ( 'NONE',  ( 0.000000000000000000, 0.000000000000000000, -1.000000000000000000 ) ) ;
#26892 = AXIS2_PLACEMENT_3D ( 'NONE', #2310, #35242, #2130 ) ;
#26893 = VECTOR ( 'NONE', #30342, 1000.000000000000000 ) ;
#26894 = EDGE_CURVE ( 'NONE', #33119, #29210, #25571, .T. ) ;
#26895 = ORIENTED_EDGE ( 'NONE', *, *, #35529, .T. ) ;
#26896 = CARTESIAN_POINT ( 'NONE',  ( 1.599999999999986766, -5.408326913195883989, -0.7999999999999944933 ) ) ;
#26897 = CARTESIAN_POINT ( 'NONE',  ( -35.50000000000000711, -112.0209493036498287, 0.9959249592223760050 ) ) ;
#26898 = CARTESIAN_POINT ( 'NONE',  ( 7.999999999999992895, 0.000000000000000000, 0.000000000000000000 ) ) ;
#26899 = AXIS2_PLACEMENT_3D ( 'NONE', #21157, #26581, #18633 ) ;
#26900 = CIRCLE ( 'NONE', #31483, 47.49900000000001654 ) ;
#26901 = CARTESIAN_POINT ( 'NONE',  ( -35.50000000000000711, -114.9929510916434339, 11.38636890470581164 ) ) ;
#26902 = DIRECTION ( 'NONE',  ( -1.000000000000000000, 0.000000000000000000, 0.000000000000000000 ) ) ;
#26903 = EDGE_LOOP ( 'NONE', ( #5990, #6156, #13262, #4716 ) ) ;
#26904 = LINE ( 'NONE', #18598, #946 ) ;
#26905 = CARTESIAN_POINT ( 'NONE',  ( -35.50000000000000000, -113.0071371610607684, 2.888584676720006961 ) ) ;
#26906 = ORIENTED_EDGE ( 'NONE', *, *, #14923, .T. ) ;
#26907 = EDGE_LOOP ( 'NONE', ( #2168, #29340, #15749, #13554 ) ) ;
#26908 = CARTESIAN_POINT ( 'NONE',  ( -38.37230871539094323, -112.5438815906447729, 2.441024454178448710 ) ) ;
#26909 = EDGE_CURVE ( 'NONE', #1552, #17434, #9467, .T. ) ;
#26910 = VECTOR ( 'NONE', #6530, 1000.000000000000000 ) ;
#26911 = DIRECTION ( 'NONE',  ( 0.000000000000000000, 0.3090169943749412895, 0.9510565162951555296 ) ) ;
#26912 = ORIENTED_EDGE ( 'NONE', *, *, #25082, .F. ) ;
#26913 = EDGE_LOOP ( 'NONE', ( #18505, #19300 ) ) ;
#26914 = CARTESIAN_POINT ( 'NONE',  ( -34.50000000000000000, -113.0140978167138996, -0.6247823525984306237 ) ) ;
#26915 = AXIS2_PLACEMENT_3D ( 'NONE', #31631, #6966, #31811 ) ;
#26916 = ADVANCED_FACE ( 'NONE', ( #14538 ), #17596, .T. ) ;
#26917 = VECTOR ( 'NONE', #11534, 1000.000000000000000 ) ;
#26918 = EDGE_CURVE ( 'NONE', #16800, #19176, #14901, .T. ) ;
#26919 = DIRECTION ( 'NONE',  ( 1.000000000000000000, -0.000000000000000000, 0.000000000000000000 ) ) ;
#26920 = DIRECTION ( 'NONE',  ( 0.000000000000000000, 0.000000000000000000, 1.000000000000000000 ) ) ;
#26921 = CARTESIAN_POINT ( 'NONE',  ( -37.48437500000004263, -114.9929510916434339, 13.11852480586264669 ) ) ;
#26922 = CARTESIAN_POINT ( 'NONE',  ( -0.2000000000000612399, -6.997142273814382030, 0.000000000000000000 ) ) ;
#26923 = ADVANCED_FACE ( 'NONE', ( #31484, #28782 ), #4132, .F. ) ;
#26924 = DIRECTION ( 'NONE',  ( -1.000000000000000000, -0.000000000000000000, 0.000000000000000000 ) ) ;
#26925 = EDGE_CURVE ( 'NONE', #27973, #4339, #19250, .T. ) ;
#26926 = CIRCLE ( 'NONE', #15967, 4.800000000000001599 ) ;
#26927 = CARTESIAN_POINT ( 'NONE',  ( -34.50000000000000000, -112.9813730236132585, -1.624774171495860786 ) ) ;
#26928 = CARTESIAN_POINT ( 'NONE',  ( 4.000000000000003553, 5.871425383721550872, 51.66745943012285380 ) ) ;
#26929 = CYLINDRICAL_SURFACE ( 'NONE', #28978, 10.99999999999999289 ) ;
#26930 = ORIENTED_EDGE ( 'NONE', *, *, #14825, .T. ) ;
#26931 = CARTESIAN_POINT ( 'NONE',  ( -37.50818044754229419, -115.9929510916434481, 13.11847460610629845 ) ) ;
#26932 = DIRECTION ( 'NONE',  ( 0.000000000000000000, 1.000000000000000000, 0.000000000000000000 ) ) ;
#26933 =( NAMED_UNIT ( * ) PLANE_ANGLE_UNIT ( ) SI_UNIT ( $, .RADIAN. ) );
#26934 = DIRECTION ( 'NONE',  ( 1.000000000000000000, -5.339440136655842133E-16, -1.047965281155519420E-16 ) ) ;
#26935 = CARTESIAN_POINT ( 'NONE',  ( -21.15833593587365513, -34.27980021920977549, 73.62564434701768334 ) ) ;
#26936 = EDGE_CURVE ( 'NONE', #9715, #19677, #6984, .T. ) ;
#26937 = VERTEX_POINT ( 'NONE', #26798 ) ;
#26938 = DIRECTION ( 'NONE',  ( -1.000000000000000000, 0.000000000000000000, 0.000000000000000000 ) ) ;
#26939 = CARTESIAN_POINT ( 'NONE',  ( 0.000000000000000000, -46.87740477351719193, 3.172455868805032608 ) ) ;
#26940 = DIRECTION ( 'NONE',  ( 0.000000000000000000, -0.6427876096865456912, 0.7660444431189726844 ) ) ;
#26941 = DIRECTION ( 'NONE',  ( 0.000000000000000000, -0.7705132427757949154, 0.6374239897486828621 ) ) ;
#26942 = CIRCLE ( 'NONE', #9080, 6.000000000000005329 ) ;
#26943 = CARTESIAN_POINT ( 'NONE',  ( 8.000000000000000000, -15.17386234660370015, -15.92965478239635679 ) ) ;
#26944 = CARTESIAN_POINT ( 'NONE',  ( 0.000000000000000000, 3.975523202428013381, 13.42368113696675103 ) ) ;
#26945 = ORIENTED_EDGE ( 'NONE', *, *, #4635, .T. ) ;
#26946 = VERTEX_POINT ( 'NONE', #24275 ) ;
#26947 = AXIS2_PLACEMENT_3D ( 'NONE', #8150, #19132, #27955 ) ;
#26948 = DIRECTION ( 'NONE',  ( 0.000000000000000000, 0.000000000000000000, 1.000000000000000000 ) ) ;
#26949 = DIRECTION ( 'NONE',  ( -1.000000000000000000, 0.000000000000000000, 0.000000000000000000 ) ) ;
#26950 = DIRECTION ( 'NONE',  ( 0.000000000000000000, 0.000000000000000000, 1.000000000000000000 ) ) ;
#26951 = EDGE_LOOP ( 'NONE', ( #5372, #34021 ) ) ;
#26952 = CARTESIAN_POINT ( 'NONE',  ( -34.97545270896703329, -114.7691647218148745, 4.090225545821551734 ) ) ;
#26953 = VERTEX_POINT ( 'NONE', #15779 ) ;
#26954 = AXIS2_PLACEMENT_3D ( 'NONE', #25162, #33598, #12003 ) ;
#26955 = EDGE_CURVE ( 'NONE', #17882, #6879, #1776, .T. ) ;
#26956 = ORIENTED_EDGE ( 'NONE', *, *, #878, .F. ) ;
#26957 = VERTEX_POINT ( 'NONE', #1956 ) ;
#26958 = CARTESIAN_POINT ( 'NONE',  ( 0.000000000000000000, -16.31134495048486954, 6.336799421339753380 ) ) ;
#26959 = EDGE_CURVE ( 'NONE', #20133, #20788, #18136, .T. ) ;
#26960 = EDGE_CURVE ( 'NONE', #9557, #2406, #29144, .T. ) ;
#26961 = DIRECTION ( 'NONE',  ( 0.000000000000000000, 0.6845471059286899473, -0.7289686274214103312 ) ) ;
#26962 = ORIENTED_EDGE ( 'NONE', *, *, #17253, .T. ) ;
#26963 = VERTEX_POINT ( 'NONE', #7687 ) ;
#26964 = LINE ( 'NONE', #2306, #26577 ) ;
#26965 = DIRECTION ( 'NONE',  ( 0.000000000000000000, 0.000000000000000000, 1.000000000000000000 ) ) ;
#26966 = EDGE_CURVE ( 'NONE', #6240, #26262, #29634, .T. ) ;
#26967 = LINE ( 'NONE', #13106, #31473 ) ;
#26968 = ADVANCED_FACE ( 'NONE', ( #12754 ), #29322, .F. ) ;
#26969 = VECTOR ( 'NONE', #16033, 1000.000000000000000 ) ;
#26970 = LINE ( 'NONE', #30016, #26311 ) ;
#26971 = CARTESIAN_POINT ( 'NONE',  ( -27.00000000000000000, 45.00000000000000000, 5.510910596163089556E-15 ) ) ;
#26972 = AXIS2_PLACEMENT_3D ( 'NONE', #1128, #17489, #11924 ) ;
#26973 = CARTESIAN_POINT ( 'NONE',  ( -35.02454729103298092, -114.8876895276775087, 3.097274454178448710 ) ) ;
#26974 = CARTESIAN_POINT ( 'NONE',  ( -34.50000000000000000, -115.9929510916434481, 10.52826033068511435 ) ) ;
#26975 = DIRECTION ( 'NONE',  ( 0.000000000000000000, 0.3090169943749477288, -0.9510565162951535312 ) ) ;
#26976 = CYLINDRICAL_SURFACE ( 'NONE', #32811, 3.799999999999999822 ) ;
#26977 = CARTESIAN_POINT ( 'NONE',  ( 0.000000000000000000, 0.000000000000000000, 0.000000000000000000 ) ) ;
#26978 = DIRECTION ( 'NONE',  ( 0.000000000000000000, 0.000000000000000000, 1.000000000000000000 ) ) ;
#26979 = DIRECTION ( 'NONE',  ( 1.000000000000000000, -0.000000000000000000, -0.000000000000000000 ) ) ;
#26980 = DIRECTION ( 'NONE',  ( -1.000000000000000000, 0.000000000000000000, -0.000000000000000000 ) ) ;
#26981 = VERTEX_POINT ( 'NONE', #2325 ) ;
#26982 = CARTESIAN_POINT ( 'NONE',  ( -34.02454729103297382, -112.6980969099494132, 8.402725545821549957 ) ) ;
#26983 = CARTESIAN_POINT ( 'NONE',  ( 70.00000000000001421, 55.12602127901489268, 78.31438535856030114 ) ) ;
#26984 = CARTESIAN_POINT ( 'NONE',  ( 8.000000000000007105, 0.000000000000000000, 0.000000000000000000 ) ) ;
#26985 = ORIENTED_EDGE ( 'NONE', *, *, #34608, .F. ) ;
#26986 = ORIENTED_EDGE ( 'NONE', *, *, #10820, .F. ) ;
#26987 = DIRECTION ( 'NONE',  ( 0.000000000000000000, 0.2486898871648552389, -0.9685831611286309650 ) ) ;
#26988 = CARTESIAN_POINT ( 'NONE',  ( 7.999999999999992895, -22.82995208772716467, 41.06517797613655318 ) ) ;
#26989 = ORIENTED_EDGE ( 'NONE', *, *, #32627, .F. ) ;
#26990 = ORIENTED_EDGE ( 'NONE', *, *, #9939, .T. ) ;
#26991 = VECTOR ( 'NONE', #33188, 1000.000000000000000 ) ;
#26992 = EDGE_CURVE ( 'NONE', #15707, #20157, #12577, .T. ) ;
#26993 = FACE_OUTER_BOUND ( 'NONE', #29265, .T. ) ;
#26994 = DIRECTION ( 'NONE',  ( -1.000000000000000000, -0.000000000000000000, -0.000000000000000000 ) ) ;
#26995 = DIRECTION ( 'NONE',  ( -1.000000000000000000, 4.770489558936248013E-18, -1.848543147300120115E-33 ) ) ;
#26996 = DIRECTION ( 'NONE',  ( 1.000000000000000000, 0.000000000000000000, 0.000000000000000000 ) ) ;
#26997 = ORIENTED_EDGE ( 'NONE', *, *, #34625, .T. ) ;
#26998 = VERTEX_POINT ( 'NONE', #4305 ) ;
#26999 = CARTESIAN_POINT ( 'NONE',  ( -35.50000000000000711, -112.0140978167138712, 0.5627176474015717078 ) ) ;
#27000 = DIRECTION ( 'NONE',  ( -1.000000000000000000, -0.000000000000000000, 0.000000000000000000 ) ) ;
#27001 = CARTESIAN_POINT ( 'NONE',  ( 0.000000000000000000, -35.20873326984104068, 31.88259874184018372 ) ) ;
#27002 = ORIENTED_EDGE ( 'NONE', *, *, #27776, .F. ) ;
#27003 = LINE ( 'NONE', #4697, #15494 ) ;
#27004 = CARTESIAN_POINT ( 'NONE',  ( -34.50000000000000000, -115.9821387493194891, -0.8839717462762166633 ) ) ;
#27005 = CARTESIAN_POINT ( 'NONE',  ( -39.00000000000000711, -114.9929510916434339, 12.57451923796417503 ) ) ;
#27006 = DIRECTION ( 'NONE',  ( 1.000000000000000000, -4.607758420995284547E-15, -1.196244974681468202E-15 ) ) ;
#27007 = AXIS2_PLACEMENT_3D ( 'NONE', #17937, #28937, #1391 ) ;
#27008 = CARTESIAN_POINT ( 'NONE',  ( -38.00000000000000711, -114.9929510916434339, 12.39849696637031151 ) ) ;
#27009 = DIRECTION ( 'NONE',  ( -1.000000000000000000, 0.000000000000000000, 0.000000000000000000 ) ) ;
#27010 = CARTESIAN_POINT ( 'NONE',  ( -34.50000000000000000, -114.9929510916434339, 10.56126450660895699 ) ) ;
#27011 = DIRECTION ( 'NONE',  ( 0.000000000000000000, 0.000000000000000000, 1.000000000000000000 ) ) ;
#27012 = CARTESIAN_POINT ( 'NONE',  ( -37.56526046546250086, -114.9929510916434339, 13.11451721564129258 ) ) ;
#27013 = DIRECTION ( 'NONE',  ( -1.174092375852890260E-15, 4.222049128630259891E-16, 1.000000000000000000 ) ) ;
#27014 = ORIENTED_EDGE ( 'NONE', *, *, #13687, .F. ) ;
#27015 = VECTOR ( 'NONE', #10262, 1000.000000000000000 ) ;
#27016 = CARTESIAN_POINT ( 'NONE',  ( 8.000000000000007105, 11.27190672109280811, 4.484851126495202678 ) ) ;
#27017 = CARTESIAN_POINT ( 'NONE',  ( 55.00000000000000000, 20.00000000000001776, -25.00000000000000000 ) ) ;
#27018 = EDGE_LOOP ( 'NONE', ( #7309, #2834, #3277, #24078 ) ) ;
#27019 = CARTESIAN_POINT ( 'NONE',  ( -38.00000000000000711, -114.9929510916434339, 12.39849696637031151 ) ) ;
#27020 = ORIENTED_EDGE ( 'NONE', *, *, #31604, .T. ) ;
#27021 = PRESENTATION_LAYER_ASSIGNMENT (  '', '', ( #20061 ) ) ;
#27022 = AXIS2_PLACEMENT_3D ( 'NONE', #13310, #2165, #4684 ) ;
#27023 = CARTESIAN_POINT ( 'NONE',  ( -37.05926240293131713, -115.9999999999999858, 7.878524454178450043 ) ) ;
#27024 = AXIS2_PLACEMENT_3D ( 'NONE', #34567, #29169, #1434 ) ;
#27025 = DIRECTION ( 'NONE',  ( 0.000000000000000000, 0.000000000000000000, -1.000000000000000000 ) ) ;
#27026 = ORIENTED_EDGE ( 'NONE', *, *, #14825, .F. ) ;
#27027 = ORIENTED_EDGE ( 'NONE', *, *, #10653, .T. ) ;
#27028 = LINE ( 'NONE', #16011, #25169 ) ;
#27029 = LINE ( 'NONE', #10461, #22626 ) ;
#27030 = ORIENTED_EDGE ( 'NONE', *, *, #1143, .F. ) ;
#27031 = CARTESIAN_POINT ( 'NONE',  ( -39.99999999999999289, -113.9407375970686758, 5.253524454178449155 ) ) ;
#27032 = DIRECTION ( 'NONE',  ( 0.000000000000000000, 0.000000000000000000, -1.000000000000000000 ) ) ;
#27033 = EDGE_CURVE ( 'NONE', #20788, #19400, #3746, .T. ) ;
#27034 = CARTESIAN_POINT ( 'NONE',  ( 8.000000000000000000, -17.47118961583602470, 0.9861715913087032437 ) ) ;
#27035 = ORIENTED_EDGE ( 'NONE', *, *, #30609, .T. ) ;
#27036 = ORIENTED_EDGE ( 'NONE', *, *, #2259, .T. ) ;
#27037 = CYLINDRICAL_SURFACE ( 'NONE', #22851, 4.000000000000000000 ) ;
#27038 = AXIS2_PLACEMENT_3D ( 'NONE', #20764, #17898, #1175 ) ;
#27039 = FILL_AREA_STYLE ('',( #15667 ) ) ;
#27040 = LINE ( 'NONE', #2214, #25933 ) ;
#27041 = ORIENTED_EDGE ( 'NONE', *, *, #29961, .T. ) ;
#27042 = ORIENTED_EDGE ( 'NONE', *, *, #19802, .F. ) ;
#27043 = CIRCLE ( 'NONE', #22404, 3.799999999999999822 ) ;
#27044 = CARTESIAN_POINT ( 'NONE',  ( -34.50000000000000000, -111.0140978167138570, 0.6252176474015680441 ) ) ;
#27045 = ADVANCED_FACE ( 'NONE', ( #35261 ), #32012, .T. ) ;
#27046 = DIRECTION ( 'NONE',  ( 0.000000000000000000, 0.000000000000000000, 1.000000000000000000 ) ) ;
#27047 = AXIS2_PLACEMENT_3D ( 'NONE', #17851, #31896, #23450 ) ;
#27048 = ORIENTED_EDGE ( 'NONE', *, *, #16775, .T. ) ;
#27049 = CIRCLE ( 'NONE', #21833, 20.00000000000000355 ) ;
#27050 = DIRECTION ( 'NONE',  ( -1.000000000000000000, 0.000000000000000000, 0.000000000000000000 ) ) ;
#27051 = CARTESIAN_POINT ( 'NONE',  ( -38.00000000000000711, -113.9929510916434339, 11.91443571948719615 ) ) ;
#27052 = DIRECTION ( 'NONE',  ( 1.000000000000000000, -0.000000000000000000, -0.000000000000000000 ) ) ;
#27053 = DIRECTION ( 'NONE',  ( -1.000000000000000000, 0.000000000000000000, 0.000000000000000000 ) ) ;
#27054 = CARTESIAN_POINT ( 'NONE',  ( -34.50000000000000000, -113.9929510916434339, 10.50625754673586876 ) ) ;
#27055 = CARTESIAN_POINT ( 'NONE',  ( -37.99974912065192001, -115.9929510916434481, 12.63488142334838749 ) ) ;
#27056 = FACE_OUTER_BOUND ( 'NONE', #15389, .T. ) ;
#27057 = DIRECTION ( 'NONE',  ( 0.000000000000000000, -9.406921877466749789E-15, 1.000000000000000000 ) ) ;
#27058 = ORIENTED_EDGE ( 'NONE', *, *, #31259, .F. ) ;
#27059 = DIRECTION ( 'NONE',  ( -1.000000000000000000, -0.000000000000000000, -0.000000000000000000 ) ) ;
#27060 = DIRECTION ( 'NONE',  ( -5.339440136655842133E-16, -1.000000000000000000, 6.938893903907197563E-17 ) ) ;
#27061 = DIRECTION ( 'NONE',  ( 8.708451184622495809E-17, -6.938893903907203726E-17, -1.000000000000000000 ) ) ;
#27062 = ADVANCED_FACE ( 'NONE', ( #10583 ), #5014, .T. ) ;
#27063 = EDGE_LOOP ( 'NONE', ( #5889, #13949, #30912, #26506 ) ) ;
#27064 = AXIS2_PLACEMENT_3D ( 'NONE', #18664, #15959, #4486 ) ;
#27065 = LINE ( 'NONE', #13732, #930 ) ;
#27066 = CARTESIAN_POINT ( 'NONE',  ( -35.50000000000000711, -115.8137639216009234, -1.239329810084483841 ) ) ;
#27067 = CARTESIAN_POINT ( 'NONE',  ( -4.121423858225413461, -12.61643262889540473, -1.200000000000006617 ) ) ;
#27068 = CIRCLE ( 'NONE', #17840, 7.199999999999993072 ) ;
#27069 = CARTESIAN_POINT ( 'NONE',  ( -35.50000000000000711, -114.9929510916434339, 10.51725893871048889 ) ) ;
#27070 = DIRECTION ( 'NONE',  ( -0.000000000000000000, -1.000000000000000000, 0.000000000000000000 ) ) ;
#27071 = VERTEX_POINT ( 'NONE', #29498 ) ;
#27072 = CARTESIAN_POINT ( 'NONE',  ( 1.479000000000008086, 0.000000000000000000, 0.000000000000000000 ) ) ;
#27073 = EDGE_CURVE ( 'NONE', #26937, #34424, #15600, .T. ) ;
#27074 = CARTESIAN_POINT ( 'NONE',  ( -35.50000000000000000, -111.3577635893106361, 2.022004269840791402 ) ) ;
#27075 = ORIENTED_EDGE ( 'NONE', *, *, #26507, .F. ) ;
#27076 = EDGE_LOOP ( 'NONE', ( #6344, #27767, #29164, #34227 ) ) ;
#27077 = EDGE_CURVE ( 'NONE', #656, #21748, #20388, .T. ) ;
#27078 = CARTESIAN_POINT ( 'NONE',  ( -37.97545270896701908, -113.5265240346955977, 8.347274454178448266 ) ) ;
#27079 = SURFACE_SIDE_STYLE ('',( #30127 ) ) ;
#27080 = LINE ( 'NONE', #30128, #23879 ) ;
#27081 = VERTEX_POINT ( 'NONE', #13297 ) ;
#27082 = ORIENTED_EDGE ( 'NONE', *, *, #6170, .F. ) ;
#27083 = CARTESIAN_POINT ( 'NONE',  ( -34.50000000000000000, -113.0140978167129617, -0.6247823525984270709 ) ) ;
#27084 = DIRECTION ( 'NONE',  ( 0.000000000000000000, 0.000000000000000000, 1.000000000000000000 ) ) ;
#27085 = AXIS2_PLACEMENT_3D ( 'NONE', #33714, #19493, #27627 ) ;
#27086 = EDGE_CURVE ( 'NONE', #34424, #30962, #3186, .T. ) ;
#27087 = DIRECTION ( 'NONE',  ( 0.000000000000000000, 0.000000000000000000, -1.000000000000000000 ) ) ;
#27088 = EDGE_CURVE ( 'NONE', #14794, #16713, #8896, .T. ) ;
#27089 = CARTESIAN_POINT ( 'NONE',  ( 8.000000000000000000, -9.471478019455027209, -14.71414642875966017 ) ) ;
#27090 = CARTESIAN_POINT ( 'NONE',  ( -37.49414064056234253, -114.9929510916434339, 13.11852578240983291 ) ) ;
#27091 = CYLINDRICAL_SURFACE ( 'NONE', #14384, 4.000000000000000000 ) ;
#27092 = LINE ( 'NONE', #30139, #29167 ) ;
#27093 = CIRCLE ( 'NONE', #10971, 4.000000000000000000 ) ;
#27094 = AXIS2_PLACEMENT_3D ( 'NONE', #20714, #23069, #4016 ) ;
#27095 = CARTESIAN_POINT ( 'NONE',  ( -34.50000000000000000, -113.3474311500483935, -1.624782352598427959 ) ) ;
#27096 = AXIS2_PLACEMENT_3D ( 'NONE', #23932, #29516, #7702 ) ;
#27097 = CARTESIAN_POINT ( 'NONE',  ( 0.000000000000000000, 0.000000000000000000, 0.000000000000000000 ) ) ;
#27098 = FACE_OUTER_BOUND ( 'NONE', #9933, .T. ) ;
#27099 = ORIENTED_EDGE ( 'NONE', *, *, #18052, .T. ) ;
#27100 = CARTESIAN_POINT ( 'NONE',  ( -38.00000000000000711, -115.9929510916434481, 12.56351784598954779 ) ) ;
#27101 = CARTESIAN_POINT ( 'NONE',  ( 4.000000000000003553, -3.975523202428068892, 13.42368113696675103 ) ) ;
#27102 =( LENGTH_UNIT ( ) NAMED_UNIT ( * ) SI_UNIT ( .MILLI., .METRE. ) );
#27103 = CARTESIAN_POINT ( 'NONE',  ( 8.000000000000000000, 12.96676809804150565, 13.60411018104323411 ) ) ;
#27104 = ADVANCED_FACE ( 'NONE', ( #9862 ), #16315, .T. ) ;
#27105 = FACE_OUTER_BOUND ( 'NONE', #28257, .T. ) ;
#27106 = ORIENTED_EDGE ( 'NONE', *, *, #14000, .F. ) ;
#27107 = DIRECTION ( 'NONE',  ( -1.000000000000000000, 0.000000000000000000, 0.000000000000000000 ) ) ;
#27108 = FACE_OUTER_BOUND ( 'NONE', #18516, .T. ) ;
#27109 = CYLINDRICAL_SURFACE ( 'NONE', #22262, 47.49900000000001654 ) ;
#27110 = LINE ( 'NONE', #21866, #19554 ) ;
#27111 = AXIS2_PLACEMENT_3D ( 'NONE', #29126, #31466, #32176 ) ;
#27112 = DIRECTION ( 'NONE',  ( -1.000000000000000000, 0.000000000000000000, 0.000000000000000000 ) ) ;
#27113 = DIRECTION ( 'NONE',  ( 0.000000000000000000, 1.000000000000000000, 0.000000000000000000 ) ) ;
#27114 = ORIENTED_EDGE ( 'NONE', *, *, #7507, .T. ) ;
#27115 = ORIENTED_EDGE ( 'NONE', *, *, #16996, .F. ) ;
#27116 = CARTESIAN_POINT ( 'NONE',  ( 8.000000000000000000, 0.000000000000000000, 0.000000000000000000 ) ) ;
#27117 = EDGE_CURVE ( 'NONE', #25259, #10473, #35612, .T. ) ;
#27118 = DIRECTION ( 'NONE',  ( 1.000000000000000000, 0.000000000000000000, 0.000000000000000000 ) ) ;
#27119 = LINE ( 'NONE', #7483, #31308 ) ;
#27120 = ORIENTED_EDGE ( 'NONE', *, *, #29066, .T. ) ;
#27121 = EDGE_CURVE ( 'NONE', #26795, #8310, #13982, .T. ) ;
#27122 = CARTESIAN_POINT ( 'NONE',  ( -37.88768952767750875, -112.0245472910329880, 5.027725545821550845 ) ) ;
#27123 = ADVANCED_FACE ( 'NONE', ( #10761 ), #13464, .T. ) ;
#27124 = EDGE_LOOP ( 'NONE', ( #30952, #27207, #30520, #26852 ) ) ;
#27125 = VECTOR ( 'NONE', #14415, 999.9999999999998863 ) ;
#27126 =( GEOMETRIC_REPRESENTATION_CONTEXT ( 3 ) GLOBAL_UNCERTAINTY_ASSIGNED_CONTEXT ( ( #28687 ) ) GLOBAL_UNIT_ASSIGNED_CONTEXT ( ( #10148, #15712, #753 ) ) REPRESENTATION_CONTEXT ( 'NONE', 'WORKASPACE' ) );
#27127 = AXIS2_PLACEMENT_3D ( 'NONE', #10598, #32030, #13139 ) ;
#27128 = SURFACE_STYLE_FILL_AREA ( #16108 ) ;
#27129 = ORIENTED_EDGE ( 'NONE', *, *, #32174, .F. ) ;
#27130 = ORIENTED_EDGE ( 'NONE', *, *, #1659, .T. ) ;
#27131 = DIRECTION ( 'NONE',  ( -1.000000000000000000, 0.000000000000000000, 0.000000000000000000 ) ) ;
#27132 = EDGE_CURVE ( 'NONE', #31502, #31127, #24626, .T. ) ;
#27133 = CARTESIAN_POINT ( 'NONE',  ( 5.639656061357293915, -10.48075544252193048, 0.000000000000000000 ) ) ;
#27134 = ORIENTED_EDGE ( 'NONE', *, *, #5536, .F. ) ;
#27135 = VERTEX_POINT ( 'NONE', #482 ) ;
#27136 = DIRECTION ( 'NONE',  ( -1.000000000000000000, 0.000000000000000000, 0.000000000000000000 ) ) ;
#27137 = DIRECTION ( 'NONE',  ( -1.000000000000000000, 0.000000000000000000, -0.000000000000000000 ) ) ;
#27138 = CARTESIAN_POINT ( 'NONE',  ( 8.000000000000000000, -9.508666619816786181, 19.83898331853681896 ) ) ;
#27139 = DIRECTION ( 'NONE',  ( 1.000000000000000000, 0.000000000000000000, 0.000000000000000000 ) ) ;
#27140 = DIRECTION ( 'NONE',  ( -1.000000000000000000, 0.000000000000000000, 0.000000000000000000 ) ) ;
#27141 = CARTESIAN_POINT ( 'NONE',  ( -35.00000000000000000, -114.0592624029313242, 6.003524454178450043 ) ) ;
#27142 = CIRCLE ( 'NONE', #17343, 20.00000000000000355 ) ;
#27143 = CARTESIAN_POINT ( 'NONE',  ( -36.62499999999902656, -115.9929510916434481, 14.11852480586265024 ) ) ;
#27145 = DIRECTION ( 'NONE',  ( 0.000000000000000000, 0.000000000000000000, -1.000000000000000000 ) ) ;
#27144 = AXIS2_PLACEMENT_3D ( 'NONE', #8588, #11131, #22616 ) ;
#27146 = EDGE_CURVE ( 'NONE', #29572, #20307, #30192, .T. ) ;
#27147 = DIRECTION ( 'NONE',  ( 0.000000000000000000, -0.3420201433256564449, -0.9396926207859127578 ) ) ;
#27148 = DIRECTION ( 'NONE',  ( -1.000000000000000000, 0.000000000000000000, 0.000000000000000000 ) ) ;
#27149 = DIRECTION ( 'NONE',  ( 0.9995917534020517525, -0.02857142857142376188, -1.185676054145132037E-15 ) ) ;
#27150 = ADVANCED_FACE ( 'NONE', ( #297 ), #19202, .F. ) ;
#27151 = CARTESIAN_POINT ( 'NONE',  ( 0.000000000000000000, -18.53613841426824038, 48.58406706613897796 ) ) ;
#27152 = DIRECTION ( 'NONE',  ( 0.000000000000000000, 0.000000000000000000, 1.000000000000000000 ) ) ;
#27153 = ORIENTED_EDGE ( 'NONE', *, *, #1064, .F. ) ;
#27154 = CARTESIAN_POINT ( 'NONE',  ( -34.97545270896703329, -114.7691647218148745, 4.090225545821551734 ) ) ;
#27155 = DIRECTION ( 'NONE',  ( 0.000000000000000000, 0.000000000000000000, 1.000000000000000000 ) ) ;
#27156 = CARTESIAN_POINT ( 'NONE',  ( -42.49999999999999289, -33.18172400785640264, 69.52756813566438154 ) ) ;
#27157 = FACE_OUTER_BOUND ( 'NONE', #34476, .T. ) ;
#27158 = ORIENTED_EDGE ( 'NONE', *, *, #15431, .F. ) ;
#27159 = AXIS2_PLACEMENT_3D ( 'NONE', #26661, #12967, #1814 ) ;
#27160 = VERTEX_POINT ( 'NONE', #21909 ) ;
#27161 = DIRECTION ( 'NONE',  ( -1.000000000000000000, -1.836970198721029934E-16, -0.000000000000000000 ) ) ;
#27162 = DIRECTION ( 'NONE',  ( 0.000000000000000000, 0.3681245526846720906, 0.9297764858882537897 ) ) ;
#27163 = ORIENTED_EDGE ( 'NONE', *, *, #9775, .F. ) ;
#27164 = EDGE_CURVE ( 'NONE', #33309, #19887, #30550, .T. ) ;
#27165 = VERTEX_POINT ( 'NONE', #2851 ) ;
#27166 = EDGE_CURVE ( 'NONE', #20656, #10643, #29032, .T. ) ;
#27167 = DIRECTION ( 'NONE',  ( 1.000000000000000000, -4.528031003192420052E-15, -1.179290629824070178E-15 ) ) ;
#27168 = DIRECTION ( 'NONE',  ( 1.000000000000000000, 0.000000000000000000, 0.000000000000000000 ) ) ;
#27169 = AXIS2_PLACEMENT_3D ( 'NONE', #29837, #21178, #12910 ) ;
#27170 = AXIS2_PLACEMENT_3D ( 'NONE', #28534, #33572, #28716 ) ;
#27171 = CARTESIAN_POINT ( 'NONE',  ( -30.00000000000001421, 0.000000000000000000, 70.00000000000000000 ) ) ;
#27172 = DIRECTION ( 'NONE',  ( -1.000000000000000000, -1.836970198721029934E-16, -0.000000000000000000 ) ) ;
#27173 = ORIENTED_EDGE ( 'NONE', *, *, #6378, .F. ) ;
#27174 = ORIENTED_EDGE ( 'NONE', *, *, #4006, .T. ) ;
#27175 = CARTESIAN_POINT ( 'NONE',  ( -35.50000000000000711, -112.3465879560236687, 1.629585756119413364 ) ) ;
#27176 =( REPRESENTATION_RELATIONSHIP ('NONE','NONE', #26607, #2005 ) REPRESENTATION_RELATIONSHIP_WITH_TRANSFORMATION ( #3517 )SHAPE_REPRESENTATION_RELATIONSHIP( ) );
#27177 = FACE_OUTER_BOUND ( 'NONE', #15319, .T. ) ;
#27178 = DIRECTION ( 'NONE',  ( -1.000000000000000000, -0.000000000000000000, 0.000000000000000000 ) ) ;
#27179 = ORIENTED_EDGE ( 'NONE', *, *, #3496, .F. ) ;
#27180 = CARTESIAN_POINT ( 'NONE',  ( 8.000000000000000000, -18.62763138773852134, 2.494040418455287345 ) ) ;
#27181 = AXIS2_PLACEMENT_3D ( 'NONE', #15025, #6934, #17907 ) ;
#27182 = CARTESIAN_POINT ( 'NONE',  ( -34.50000000000000000, -112.0651520602111191, -0.9469505670458575608 ) ) ;
#27183 = CARTESIAN_POINT ( 'NONE',  ( -37.43749999999998579, -114.9929510916434339, 14.11852480586264846 ) ) ;
#27184 = CARTESIAN_POINT ( 'NONE',  ( 7.999999999999992895, 0.000000000000000000, -3.000000000000002665 ) ) ;
#27185 = CIRCLE ( 'NONE', #16224, 47.49900000000001654 ) ;
#27186 = CARTESIAN_POINT ( 'NONE',  ( -35.50000000000000000, -113.9929510916435049, 10.50625754673586876 ) ) ;
#27187 = CARTESIAN_POINT ( 'NONE',  ( 46.00000000000000000, 0.000000000000000000, 0.000000000000000000 ) ) ;
#27188 = CARTESIAN_POINT ( 'NONE',  ( -34.50000000000000000, -114.9929510916434339, 11.73841344789270202 ) ) ;
#27189 = DIRECTION ( 'NONE',  ( 0.1305261922200566249, -0.9914448613738097160, -5.718426984394921662E-16 ) ) ;
#27190 = EDGE_CURVE ( 'NONE', #1275, #1779, #33070, .T. ) ;
#27191 = CARTESIAN_POINT ( 'NONE',  ( 0.000000000000000000, -2.710505431213761085E-17, -21.89999999999999858 ) ) ;
#27192 = FACE_OUTER_BOUND ( 'NONE', #30288, .T. ) ;
#27193 = EDGE_LOOP ( 'NONE', ( #1606, #30773, #32010, #25744 ) ) ;
#27194 = CARTESIAN_POINT ( 'NONE',  ( -42.49999999999999289, -24.48076211353304288, 71.08058909292489602 ) ) ;
#27195 = CARTESIAN_POINT ( 'NONE',  ( 8.000000000000000000, 6.860320204751148232, 13.89802171851385459 ) ) ;
#27196 = ADVANCED_FACE ( 'NONE', ( #125 ), #19031, .T. ) ;
#27197 = VERTEX_POINT ( 'NONE', #29855 ) ;
#27198 = VECTOR ( 'NONE', #9403, 1000.000000000000000 ) ;
#27199 = CARTESIAN_POINT ( 'NONE',  ( -37.93687354226506869, -114.9929510916434339, 12.87038173996323565 ) ) ;
#27200 = VERTEX_POINT ( 'NONE', #8398 ) ;
#27201 = CARTESIAN_POINT ( 'NONE',  ( -38.99999999999999289, -113.9407375970686900, 5.253524454178449155 ) ) ;
#27202 = DIRECTION ( 'NONE',  ( -1.000000000000000000, 0.000000000000000000, 0.000000000000000000 ) ) ;
#27203 = VERTEX_POINT ( 'NONE', #22260 ) ;
#27204 = ORIENTED_EDGE ( 'NONE', *, *, #904, .T. ) ;
#27205 = CARTESIAN_POINT ( 'NONE',  ( 7.999999999999992895, 0.000000000000000000, 0.000000000000000000 ) ) ;
#27206 = DIRECTION ( 'NONE',  ( -1.000000000000000000, 0.000000000000000000, 0.000000000000000000 ) ) ;
#27207 = ORIENTED_EDGE ( 'NONE', *, *, #32220, .T. ) ;
#27208 = CARTESIAN_POINT ( 'NONE',  ( -39.99999999999999289, -113.9407375970686758, 6.753524454178450043 ) ) ;
#27209 = AXIS2_PLACEMENT_3D ( 'NONE', #24007, #13201, #18585 ) ;
#27210 = AXIS2_PLACEMENT_3D ( 'NONE', #1352, #28723, #28896 ) ;
#27211 = LINE ( 'NONE', #21251, #21105 ) ;
#27212 = CARTESIAN_POINT ( 'NONE',  ( 0.000000000000000000, -2.710505431213761085E-17, 55.00000000000000000 ) ) ;
#27213 = ORIENTED_EDGE ( 'NONE', *, *, #30690, .T. ) ;
#27214 = VERTEX_POINT ( 'NONE', #14151 ) ;
#27215 = DIRECTION ( 'NONE',  ( 0.000000000000000000, 0.000000000000000000, -1.000000000000000000 ) ) ;
#27216 = ADVANCED_FACE ( 'NONE', ( #16671 ), #5197, .T. ) ;
#27217 = DIRECTION ( 'NONE',  ( 0.000000000000000000, 0.000000000000000000, -1.000000000000000000 ) ) ;
#27218 = ORIENTED_EDGE ( 'NONE', *, *, #28894, .F. ) ;
#27219 = ORIENTED_EDGE ( 'NONE', *, *, #23139, .T. ) ;
#27220 = CARTESIAN_POINT ( 'NONE',  ( -34.50000000000000000, -113.0765974847181781, -2.624803185604914102 ) ) ;
#27221 = VECTOR ( 'NONE', #15335, 1000.000000000000000 ) ;
#27222 = AXIS2_PLACEMENT_3D ( 'NONE', #5617, #11012, #6304 ) ;
#27223 = DIRECTION ( 'NONE',  ( -1.783119874454246424E-31, -1.187911941725854497E-31, 1.000000000000000000 ) ) ;
#27224 = VERTEX_POINT ( 'NONE', #27685 ) ;
#27225 = CARTESIAN_POINT ( 'NONE',  ( -35.50000000000000711, -114.9929510916434339, 10.68227981832981044 ) ) ;
#27226 = CARTESIAN_POINT ( 'NONE',  ( -34.50000000000000000, -113.9929510916434339, 12.59102132592610346 ) ) ;
#27227 = CARTESIAN_POINT ( 'NONE',  ( 0.000000000000000000, -25.61928775981012762, -45.25098998563503727 ) ) ;
#27228 = CARTESIAN_POINT ( 'NONE',  ( 4.000000000000003553, 43.55304910509448035, -28.41006711799937179 ) ) ;
#27229 = CARTESIAN_POINT ( 'NONE',  ( -38.00000000000000711, -113.9929510916434339, 12.56351784598954779 ) ) ;
#27230 = CARTESIAN_POINT ( 'NONE',  ( -35.50000000000000711, -114.9929510916434339, 10.52000928670414126 ) ) ;
#27231 = CYLINDRICAL_SURFACE ( 'NONE', #10137, 7.199999999999994849 ) ;
#27232 = VECTOR ( 'NONE', #25179, 1000.000000000000000 ) ;
#27233 = DIRECTION ( 'NONE',  ( -1.734723475976807094E-16, 9.406921877466749789E-15, -1.000000000000000000 ) ) ;
#27234 = ADVANCED_FACE ( 'NONE', ( #3023 ), #8574, .T. ) ;
#27235 = ORIENTED_EDGE ( 'NONE', *, *, #19805, .T. ) ;
#27236 = DIRECTION ( 'NONE',  ( 0.000000000000000000, 0.000000000000000000, 1.000000000000000000 ) ) ;
#27237 = CARTESIAN_POINT ( 'NONE',  ( 0.000000000000000000, 0.000000000000000000, -65.00000000000000000 ) ) ;
#27238 = CARTESIAN_POINT ( 'NONE',  ( 0.000000000000000000, -13.24207120356975587, 14.98824707027438485 ) ) ;
#27239 = ORIENTED_EDGE ( 'NONE', *, *, #23549, .F. ) ;
#27240 = LINE ( 'NONE', #35347, #5544 ) ;
#27241 = ORIENTED_EDGE ( 'NONE', *, *, #34853, .T. ) ;
#27242 = AXIS2_PLACEMENT_3D ( 'NONE', #28292, #13896, #6144 ) ;
#27243 = AXIS2_PLACEMENT_3D ( 'NONE', #19742, #513, #3225 ) ;
#27244 = CARTESIAN_POINT ( 'NONE',  ( -35.50000000000000711, -116.0140978167138712, -0.3747823525984422255 ) ) ;
#27245 = DIRECTION ( 'NONE',  ( -1.000000000000000000, 0.000000000000000000, 0.000000000000000000 ) ) ;
#27246 = EDGE_CURVE ( 'NONE', #23706, #7811, #15794, .T. ) ;
#27247 = CARTESIAN_POINT ( 'NONE',  ( -35.50000000000000711, -114.9929510916434339, 11.91443571948719971 ) ) ;
#27248 = LINE ( 'NONE', #24019, #27430 ) ;
#27249 = EDGE_LOOP ( 'NONE', ( #25428, #2249, #19821, #10275 ) ) ;
#27250 = FACE_BOUND ( 'NONE', #29561, .T. ) ;
#27251 = CARTESIAN_POINT ( 'NONE',  ( -35.50000000000000000, -111.0140978167138570, -0.1247823525984260717 ) ) ;
#27252 = VERTEX_POINT ( 'NONE', #16847 ) ;
#27253 = ORIENTED_EDGE ( 'NONE', *, *, #7274, .T. ) ;
#27254 = CARTESIAN_POINT ( 'NONE',  ( -37.99999999999998579, -113.9407375970686758, 6.753524454178450043 ) ) ;
#27255 = CARTESIAN_POINT ( 'NONE',  ( -34.49999999999998579, -28.31857036507959791, 80.03062855292519373 ) ) ;
#27257 = ORIENTED_EDGE ( 'NONE', *, *, #5727, .T. ) ;
#27256 = AXIS2_PLACEMENT_3D ( 'NONE', #23717, #4825, #4294 ) ;
#27258 = VERTEX_POINT ( 'NONE', #5368 ) ;
#27259 = CARTESIAN_POINT ( 'NONE',  ( -34.50000000000000000, -113.0140978167138712, -0.6247823525983134951 ) ) ;
#27260 = DIRECTION ( 'NONE',  ( -1.000000000000000000, 0.000000000000000000, 0.000000000000000000 ) ) ;
#27261 = FACE_OUTER_BOUND ( 'NONE', #9198, .T. ) ;
#27262 = CARTESIAN_POINT ( 'NONE',  ( 7.999999999999992895, -0.2227391519113268437, -46.98410307550732057 ) ) ;
#27263 = AXIS2_PLACEMENT_3D ( 'NONE', #22309, #27731, #8975 ) ;
#27264 = CARTESIAN_POINT ( 'NONE',  ( -35.50000000000000000, -113.9929510916434339, 12.17846912687782712 ) ) ;
#27265 = CIRCLE ( 'NONE', #19740, 4.800000000000002487 ) ;
#27266 = DIRECTION ( 'NONE',  ( -1.000000000000000000, -0.000000000000000000, 0.000000000000000000 ) ) ;
#27267 = CARTESIAN_POINT ( 'NONE',  ( 8.000000000000007105, 0.000000000000000000, 0.000000000000000000 ) ) ;
#27268 = CARTESIAN_POINT ( 'NONE',  ( -34.50000000000000000, -112.2144317118258527, -1.239329810084414341 ) ) ;
#27269 = CARTESIAN_POINT ( 'NONE',  ( -36.87500000000098765, -115.9929510916434481, 14.11852480586265024 ) ) ;
#27270 = DIRECTION ( 'NONE',  ( 0.000000000000000000, 0.000000000000000000, 1.000000000000000000 ) ) ;
#27271 = EDGE_CURVE ( 'NONE', #22983, #18045, #25024, .T. ) ;
#27272 = ADVANCED_FACE ( 'NONE', ( #28741 ), #9294, .T. ) ;
#27273 = DIRECTION ( 'NONE',  ( -1.000000000000000000, -0.000000000000000000, -0.000000000000000000 ) ) ;
#27274 = ORIENTED_EDGE ( 'NONE', *, *, #26464, .T. ) ;
#27275 = CARTESIAN_POINT ( 'NONE',  ( -35.50000000000000711, -114.1091535596544873, 9.513028657562415447 ) ) ;
#27276 = CARTESIAN_POINT ( 'NONE',  ( -44.00000000000000000, -11.00000000000000000, 0.000000000000000000 ) ) ;
#27277 = DIRECTION ( 'NONE',  ( -1.000000000000000000, 0.000000000000000000, 0.000000000000000000 ) ) ;
#27278 = CARTESIAN_POINT ( 'NONE',  ( 7.999999999999992895, 0.000000000000000000, 0.000000000000000000 ) ) ;
#27279 = AXIS2_PLACEMENT_3D ( 'NONE', #7675, #18659, #4034 ) ;
#27280 = ORIENTED_EDGE ( 'NONE', *, *, #8152, .T. ) ;
#27281 = CARTESIAN_POINT ( 'NONE',  ( 8.000000000000007105, -5.363026430117032284, -9.919332006307277183 ) ) ;
#27282 = DIRECTION ( 'NONE',  ( -1.000000000000000000, -0.000000000000000000, -0.000000000000000000 ) ) ;
#27283 = CARTESIAN_POINT ( 'NONE',  ( -42.49999999999999289, -37.35511776651544125, 93.29903810567650169 ) ) ;
#27284 = CARTESIAN_POINT ( 'NONE',  ( 39.30000000000000426, 11.00000000000000533, 1.347111479062087419E-15 ) ) ;
#27285 = EDGE_CURVE ( 'NONE', #2557, #6413, #17199, .T. ) ;
#27286 = DIRECTION ( 'NONE',  ( 1.000000000000000000, -0.000000000000000000, -0.000000000000000000 ) ) ;
#27287 = CYLINDRICAL_SURFACE ( 'NONE', #21613, 13.99999999999999822 ) ;
#27288 = ORIENTED_EDGE ( 'NONE', *, *, #23117, .F. ) ;
#27289 = ORIENTED_EDGE ( 'NONE', *, *, #22461, .F. ) ;
#27290 = VECTOR ( 'NONE', #7693, 1000.000000000000000 ) ;
#27291 = DIRECTION ( 'NONE',  ( 0.000000000000000000, 0.000000000000000000, 1.000000000000000000 ) ) ;
#27292 = CARTESIAN_POINT ( 'NONE',  ( 0.000000000000000000, 12.30077720129168384, -50.52416135122070528 ) ) ;
#27293 = DIRECTION ( 'NONE',  ( -1.000000000000000000, 0.000000000000000000, 0.000000000000000000 ) ) ;
#27294 = ORIENTED_EDGE ( 'NONE', *, *, #16924, .T. ) ;
#27295 = CARTESIAN_POINT ( 'NONE',  ( -36.23083527818512550, -111.9754527089670404, 8.215225545821549957 ) ) ;
#27296 = VERTEX_POINT ( 'NONE', #1023 ) ;
#27297 = AXIS2_PLACEMENT_3D ( 'NONE', #20116, #34370, #3590 ) ;
#27298 = VERTEX_POINT ( 'NONE', #28032 ) ;
#27299 = VERTEX_POINT ( 'NONE', #3548 ) ;
#27300 = FACE_OUTER_BOUND ( 'NONE', #3825, .T. ) ;
#27301 = EDGE_CURVE ( 'NONE', #19623, #31746, #31435, .T. ) ;
#27302 = DIRECTION ( 'NONE',  ( 0.000000000000000000, 0.000000000000000000, 1.000000000000000000 ) ) ;
#27303 = ORIENTED_EDGE ( 'NONE', *, *, #15541, .T. ) ;
#27304 = ORIENTED_EDGE ( 'NONE', *, *, #7733, .F. ) ;
#27305 = CYLINDRICAL_SURFACE ( 'NONE', #3469, 20.00000000000000711 ) ;
#27306 = CARTESIAN_POINT ( 'NONE',  ( 7.999999999999992895, -32.32520163883607722, 34.09746168776025854 ) ) ;
#27307 = CARTESIAN_POINT ( 'NONE',  ( 0.000000000000000000, 0.000000000000000000, 0.000000000000000000 ) ) ;
#27308 = LINE ( 'NONE', #2478, #20555 ) ;
#27309 = FACE_OUTER_BOUND ( 'NONE', #25843, .T. ) ;
#27310 = VECTOR ( 'NONE', #15040, 1000.000000000000000 ) ;
#27311 = EDGE_CURVE ( 'NONE', #26552, #5886, #20071, .T. ) ;
#27312 = AXIS2_PLACEMENT_3D ( 'NONE', #27549, #30423, #25010 ) ;
#27313 = ADVANCED_FACE ( 'NONE', ( #28377 ), #11999, .T. ) ;
#27314 = LINE ( 'NONE', #8212, #26653 ) ;
#27315 = EDGE_CURVE ( 'NONE', #27252, #24147, #15229, .T. ) ;
#27316 = CARTESIAN_POINT ( 'NONE',  ( -38.69949915733018742, -115.9929510916434481, 13.54034599209165890 ) ) ;
#27317 = CARTESIAN_POINT ( 'NONE',  ( -34.49999999999998579, -12.06135120645816983, 86.49999999999994316 ) ) ;
#27318 = AXIS2_PLACEMENT_3D ( 'NONE', #8049, #30385, #24802 ) ;
#27319 = CARTESIAN_POINT ( 'NONE',  ( 0.000000000000000000, 18.48663108841359559, -3.384281271887881637 ) ) ;
#27320 = CARTESIAN_POINT ( 'NONE',  ( 7.999999999999992895, -46.87740477351715640, -3.172455868805712509 ) ) ;
#27321 = LINE ( 'NONE', #30195, #22151 ) ;
#27322 = DIRECTION ( 'NONE',  ( -1.000000000000000000, 0.000000000000000000, 0.000000000000000000 ) ) ;
#27323 = ORIENTED_EDGE ( 'NONE', *, *, #15367, .F. ) ;
#27324 = EDGE_CURVE ( 'NONE', #7481, #779, #4094, .T. ) ;
#27325 = CARTESIAN_POINT ( 'NONE',  ( -35.97545270896705460, -114.3549511594417680, 4.090225545821551734 ) ) ;
#27326 = CARTESIAN_POINT ( 'NONE',  ( 0.000000000000000000, 46.11014828289831513, 9.022736828081523441 ) ) ;
#27327 = DIRECTION ( 'NONE',  ( -1.000000000000000000, 0.000000000000000000, 0.000000000000000000 ) ) ;
#27328 = DIRECTION ( 'NONE',  ( 1.000000000000000000, -0.000000000000000000, -0.000000000000000000 ) ) ;
#27329 = EDGE_CURVE ( 'NONE', #17430, #23884, #22964, .T. ) ;
#27330 = ORIENTED_EDGE ( 'NONE', *, *, #17864, .F. ) ;
#27331 = AXIS2_PLACEMENT_3D ( 'NONE', #18401, #29581, #32272 ) ;
#27332 = EDGE_LOOP ( 'NONE', ( #22397, #12980, #9257, #17426, #11690, #22486, #16023, #22865, #3587, #29909, #19264, #13133, #34153, #15350, #10600, #29446, #31541, #26807, #32074, #28430, #16495, #31829, #1534, #27564, #5429, #35435, #9668, #2830, #2255, #11340, #34367, #21829, #18892, #10867, #19714, #7217, #26648, #21203, #14999, #10837, #16690, #5408, #16201, #19468, #27609, #11925, #24390, #3329, #271, #9461, #31778, #16550, #7363 ) ) ;
#27333 = DIRECTION ( 'NONE',  ( 0.000000000000000000, 0.000000000000000000, 1.000000000000000000 ) ) ;
#27334 = DIRECTION ( 'NONE',  ( 0.000000000000000000, -0.9822872507286865007, -0.1873813145857355644 ) ) ;
#27335 = EDGE_LOOP ( 'NONE', ( #6331, #23465, #15032, #25237 ) ) ;
#27336 = ORIENTED_EDGE ( 'NONE', *, *, #15343, .T. ) ;
#27337 = CLOSED_SHELL ( 'NONE', ( #29307, #31936, #5559, #33201, #13203, #18552, #9083, #13305, #4069, #23683, #25153, #2286, #30156, #21076, #3328, #20046, #15201, #17358, #18555, #4852, #8391, #16806, #21683, #21168, #6520, #1386, #5695, #3818, #1792, #4736, #18649, #5108, #21886, #6589, #1627, #14040, #10642, #16066, #28235, #926, #14791, #10382, #681, #24746, #4884, #32591, #17579, #13530, #11520, #9036, #16650, #20202, #19546, #14039, #33713, #12103, #19211 ) ) ;
#27338 = DIRECTION ( 'NONE',  ( -1.783119874454246424E-31, -1.187911941725854497E-31, 1.000000000000000000 ) ) ;
#27339 = CIRCLE ( 'NONE', #30215, 52.00000000000000711 ) ;
#27340 = DIRECTION ( 'NONE',  ( 1.000000000000000000, 0.000000000000000000, 0.000000000000000000 ) ) ;
#27341 = APPLICATION_PROTOCOL_DEFINITION ( 'draft international standard', 'automotive_design', 1998, #18376 ) ;
#27342 = ADVANCED_FACE ( 'NONE', ( #33420 ), #15036, .F. ) ;
#27343 = VECTOR ( 'NONE', #12347, 1000.000000000000000 ) ;
#27344 = CARTESIAN_POINT ( 'NONE',  ( 8.000000000000000000, 18.48663108841356717, 3.384281271888136988 ) ) ;
#27345 = ORIENTED_EDGE ( 'NONE', *, *, #24020, .T. ) ;
#27346 = VERTEX_POINT ( 'NONE', #14494 ) ;
#27347 = EDGE_CURVE ( 'NONE', #15054, #2693, #11805, .T. ) ;
#27348 = DIRECTION ( 'NONE',  ( 1.000000000000000000, -5.339440136655842133E-16, -1.047965281155519420E-16 ) ) ;
#27349 = LINE ( 'NONE', #32559, #2337 ) ;
#27350 = EDGE_CURVE ( 'NONE', #21603, #33166, #15826, .T. ) ;
#27351 = ORIENTED_EDGE ( 'NONE', *, *, #33890, .F. ) ;
#27352 = CARTESIAN_POINT ( 'NONE',  ( -4.000000000000000000, 0.000000000000000000, -31.10000000000000142 ) ) ;
#27353 = AXIS2_PLACEMENT_3D ( 'NONE', #17641, #28644, #14935 ) ;
#27354 = CARTESIAN_POINT ( 'NONE',  ( -34.50000000000000000, -113.3474311500483935, -1.624782352598427959 ) ) ;
#27355 = CARTESIAN_POINT ( 'NONE',  ( -35.97545865737298953, -114.9929510916434339, 14.11837420659365705 ) ) ;
#27356 = ADVANCED_FACE ( 'NONE', ( #22784 ), #34142, .T. ) ;
#27357 = CARTESIAN_POINT ( 'NONE',  ( -35.50000000000000000, -113.9929510916434339, 10.50625754673586876 ) ) ;
#27358 = LINE ( 'NONE', #33285, #34717 ) ;
#27359 = ADVANCED_FACE ( 'NONE', ( #25873 ), #33787, .T. ) ;
#27360 = CARTESIAN_POINT ( 'NONE',  ( -34.50000000000000000, -114.9929510916434339, 12.56351784598954424 ) ) ;
#27361 = DIRECTION ( 'NONE',  ( -1.174092375852890260E-15, 4.222049128630259891E-16, 1.000000000000000000 ) ) ;
#27362 = DIRECTION ( 'NONE',  ( 0.000000000000000000, 0.000000000000000000, 1.000000000000000000 ) ) ;
#27363 = FILL_AREA_STYLE_COLOUR ( '', #17929 ) ;
#27364 = CARTESIAN_POINT ( 'NONE',  ( 8.000000000000000000, 0.000000000000000000, 0.000000000000000000 ) ) ;
#27365 = CARTESIAN_POINT ( 'NONE',  ( 7.999999999999992895, -22.43957647427188817, 41.27978878573619426 ) ) ;
#27366 = LINE ( 'NONE', #2717, #22655 ) ;
#27367 = AXIS2_PLACEMENT_3D ( 'NONE', #33211, #13774, #8533 ) ;
#27368 = ORIENTED_EDGE ( 'NONE', *, *, #13134, .T. ) ;
#27369 = CARTESIAN_POINT ( 'NONE',  ( -38.00000000000000711, -114.9929510916434339, 11.21034663311206181 ) ) ;
#27370 = VERTEX_POINT ( 'NONE', #3381 ) ;
#27371 = CARTESIAN_POINT ( 'NONE',  ( -34.92058450342251064, -116.1632251905417945, 1.691024454178448932 ) ) ;
#27372 = VECTOR ( 'NONE', #23085, 1000.000000000000000 ) ;
#27373 = CARTESIAN_POINT ( 'NONE',  ( 7.999999999999992895, 0.000000000000000000, 0.000000000000000000 ) ) ;
#27374 = AXIS2_PLACEMENT_3D ( 'NONE', #20920, #1874, #7076 ) ;
#27375 = EDGE_CURVE ( 'NONE', #15703, #27617, #20421, .T. ) ;
#27376 = VERTEX_POINT ( 'NONE', #22427 ) ;
#27377 = EDGE_LOOP ( 'NONE', ( #30034, #30509, #23892, #2328 ) ) ;
#27378 = AXIS2_PLACEMENT_3D ( 'NONE', #11565, #25256, #22533 ) ;
#27379 = CARTESIAN_POINT ( 'NONE',  ( -42.49999999999999289, -29.27980021920993536, 87.71410161513767889 ) ) ;
#27380 = DIRECTION ( 'NONE',  ( -0.000000000000000000, 0.000000000000000000, -1.000000000000000000 ) ) ;
#27381 = ORIENTED_EDGE ( 'NONE', *, *, #16571, .F. ) ;
#27382 = CARTESIAN_POINT ( 'NONE',  ( -35.69809690994938478, -111.0245472910330022, 8.722274454178450043 ) ) ;
#27383 = VECTOR ( 'NONE', #24660, 1000.000000000000000 ) ;
#27384 = DIRECTION ( 'NONE',  ( -1.000000000000000000, 0.000000000000000000, 0.000000000000000000 ) ) ;
#27385 = LINE ( 'NONE', #11683, #35523 ) ;
#27386 = VERTEX_POINT ( 'NONE', #8741 ) ;
#27387 = ORIENTED_EDGE ( 'NONE', *, *, #15383, .F. ) ;
#27388 = DIRECTION ( 'NONE',  ( -1.000000000000000000, 0.000000000000000000, 0.000000000000000000 ) ) ;
#27389 = EDGE_CURVE ( 'NONE', #8849, #19072, #19711, .T. ) ;
#27390 = DIRECTION ( 'NONE',  ( 1.000000000000000000, 0.000000000000000000, 0.000000000000000000 ) ) ;
#27391 = ORIENTED_EDGE ( 'NONE', *, *, #9301, .T. ) ;
#27392 = ORIENTED_EDGE ( 'NONE', *, *, #6242, .F. ) ;
#27393 = CARTESIAN_POINT ( 'NONE',  ( -34.50000000000000000, -115.3399256288223569, -2.599147725881697291 ) ) ;
#27394 = ADVANCED_FACE ( 'NONE', ( #12713 ), #34321, .T. ) ;
#27395 = PRODUCT_DEFINITION_SHAPE ( 'NONE', 'NONE',  #35653 ) ;
#27396 = VECTOR ( 'NONE', #12843, 1000.000000000000000 ) ;
#27397 = CARTESIAN_POINT ( 'NONE',  ( -50.00000000000000000, 0.000000000000000000, 78.00000000000001421 ) ) ;
#27398 = ORIENTED_EDGE ( 'NONE', *, *, #34385, .T. ) ;
#27399 = CARTESIAN_POINT ( 'NONE',  ( -35.50000000000000711, -114.9929510916434339, 10.72628538622835670 ) ) ;
#27400 = CIRCLE ( 'NONE', #26833, 8.000000000000007105 ) ;
#27401 = AXIS2_PLACEMENT_3D ( 'NONE', #12213, #28603, #31296 ) ;
#27402 = CIRCLE ( 'NONE', #21641, 4.000000000000000000 ) ;
#27403 = CARTESIAN_POINT ( 'NONE',  ( -36.06250000000000711, -113.9929510916434339, 14.11852480586265024 ) ) ;
#27404 = CARTESIAN_POINT ( 'NONE',  ( 0.000000000000000000, 9.604183132802424083, -1.108880290975567950 ) ) ;
#27405 = ADVANCED_FACE ( 'NONE', ( #7644 ), #4263, .T. ) ;
#27406 = DIRECTION ( 'NONE',  ( -1.000000000000000000, 0.000000000000000000, -0.000000000000000000 ) ) ;
#27407 = EDGE_CURVE ( 'NONE', #15604, #12176, #24459, .T. ) ;
#27408 = CARTESIAN_POINT ( 'NONE',  ( -34.50000000000000000, -113.9929510916434339, 12.56351784598954424 ) ) ;
#27409 = CARTESIAN_POINT ( 'NONE',  ( -39.00000000000000711, -114.9929510916434339, 12.59652202191340820 ) ) ;
#27410 = CARTESIAN_POINT ( 'NONE',  ( -35.50000000000000711, -114.0185793162512908, 9.502217742515812304 ) ) ;
#27411 = VECTOR ( 'NONE', #23137, 1000.000000000000000 ) ;
#27412 = FACE_OUTER_BOUND ( 'NONE', #14379, .T. ) ;
#27413 = DIRECTION ( 'NONE',  ( -1.000000000000000000, -0.000000000000000000, 0.000000000000000000 ) ) ;
#27414 = VERTEX_POINT ( 'NONE', #34680 ) ;
#27415 = DIRECTION ( 'NONE',  ( -1.000000000000000000, 4.524158825347490025E-15, 1.174092375852883357E-15 ) ) ;
#27416 = DIRECTION ( 'NONE',  ( -1.000000000000000000, 0.000000000000000000, 0.000000000000000000 ) ) ;
#27417 = LINE ( 'NONE', #24710, #18012 ) ;
#27418 = AXIS2_PLACEMENT_3D ( 'NONE', #18532, #12786, #23951 ) ;
#27419 = VERTEX_POINT ( 'NONE', #4797 ) ;
#27420 = CARTESIAN_POINT ( 'NONE',  ( 0.000000000000000000, -44.47301969247457976, 16.68249143361895293 ) ) ;
#27421 = ORIENTED_EDGE ( 'NONE', *, *, #23187, .T. ) ;
#27422 = CIRCLE ( 'NONE', #9567, 10.99999999999999645 ) ;
#27423 = CARTESIAN_POINT ( 'NONE',  ( -35.50000000000000000, -113.0140978167142833, 0.8752176474019800478 ) ) ;
#27424 = CARTESIAN_POINT ( 'NONE',  ( 0.000000000000000000, 0.000000000000000000, -49.10000000000000142 ) ) ;
#27425 = CARTESIAN_POINT ( 'NONE',  ( -37.35495115944176092, -112.9754527089670688, 4.034774454178449155 ) ) ;
#27426 = CARTESIAN_POINT ( 'NONE',  ( -35.50040135968785648, -114.9929510916434339, 12.63896776382214071 ) ) ;
#27427 = FACE_OUTER_BOUND ( 'NONE', #24296, .T. ) ;
#27428 = AXIS2_PLACEMENT_3D ( 'NONE', #34497, #2627, #27470 ) ;
#27429 = ORIENTED_EDGE ( 'NONE', *, *, #20539, .F. ) ;
#27430 = VECTOR ( 'NONE', #24363, 1000.000000000000000 ) ;
#27431 = SURFACE_STYLE_FILL_AREA ( #33176 ) ;
#27432 = CARTESIAN_POINT ( 'NONE',  ( -35.50000000000000000, -111.8727710936879589, 2.535339294948415922 ) ) ;
#27433 = EDGE_LOOP ( 'NONE', ( #11572, #23277, #11634, #12948, #30921, #11380, #20042, #19789, #6668, #32863, #20391, #6029, #30287, #9033, #23513, #7915 ) ) ;
#27434 = ORIENTED_EDGE ( 'NONE', *, *, #18468, .T. ) ;
#27435 = CARTESIAN_POINT ( 'NONE',  ( -35.00000000000000000, -114.0592624029313242, 7.503524454178449155 ) ) ;
#27436 = CIRCLE ( 'NONE', #19904, 10.99999999999999289 ) ;
#27437 =( NAMED_UNIT ( * ) PLANE_ANGLE_UNIT ( ) SI_UNIT ( $, .RADIAN. ) );
#27438 = CIRCLE ( 'NONE', #13620, 20.00000000000000355 ) ;
#27439 = CARTESIAN_POINT ( 'NONE',  ( 8.000000000000000000, 12.96676809804168862, -13.60411018104304048 ) ) ;
#27440 = VERTEX_POINT ( 'NONE', #1917 ) ;
#27441 = ORIENTED_EDGE ( 'NONE', *, *, #16474, .T. ) ;
#27442 = CARTESIAN_POINT ( 'NONE',  ( -34.50000000000000000, -113.0140978167138712, 0.2502176474015764263 ) ) ;
#27443 = DIRECTION ( 'NONE',  ( 0.000000000000000000, 0.000000000000000000, 1.000000000000000000 ) ) ;
#27444 = ADVANCED_FACE ( 'NONE', ( #31785 ), #15203, .T. ) ;
#27445 = CYLINDRICAL_SURFACE ( 'NONE', #9131, 4.000000000000000000 ) ;
#27446 = CARTESIAN_POINT ( 'NONE',  ( 50.00000000000000000, 0.000000000000000000, -8.000000000000000000 ) ) ;
#27447 = VECTOR ( 'NONE', #15957, 1000.000000000000000 ) ;
#27448 = VECTOR ( 'NONE', #7626, 1000.000000000000227 ) ;
#27449 = CARTESIAN_POINT ( 'NONE',  ( -35.50000000000000000, -113.9929510916436470, 10.50625754673581724 ) ) ;
#27450 = CARTESIAN_POINT ( 'NONE',  ( -42.49999999999999289, -23.26666049839539951, 81.70096189432331357 ) ) ;
#27451 = CARTESIAN_POINT ( 'NONE',  ( 7.999999999999992895, -51.85248208264520997, 3.914090171286008335 ) ) ;
#27452 = CARTESIAN_POINT ( 'NONE',  ( -34.50000000000000000, -111.0140978167138570, -0.3747823525984258497 ) ) ;
#27453 = CARTESIAN_POINT ( 'NONE',  ( -35.50000000000000000, -114.1371041221139109, 8.509266650872710613 ) ) ;
#27454 = DIRECTION ( 'NONE',  ( 0.000000000000000000, 0.000000000000000000, 1.000000000000000000 ) ) ;
#27455 = AXIS2_PLACEMENT_3D ( 'NONE', #19812, #20347, #17481 ) ;
#27456 = DIRECTION ( 'NONE',  ( -1.000000000000000000, 0.000000000000000000, 0.000000000000000000 ) ) ;
#27457 = AXIS2_PLACEMENT_3D ( 'NONE', #7689, #16317, #18500 ) ;
#27458 = DIRECTION ( 'NONE',  ( 0.000000000000000000, 0.000000000000000000, 1.000000000000000000 ) ) ;
#27460 = VERTEX_POINT ( 'NONE', #26943 ) ;
#27459 = MECHANICAL_DESIGN_GEOMETRIC_PRESENTATION_REPRESENTATION (  '', ( #30331 ), #10207 ) ;
#27461 = CARTESIAN_POINT ( 'NONE',  ( -38.00000000000000711, -115.9929510916434481, 12.59652202191340820 ) ) ;
#27462 = DIRECTION ( 'NONE',  ( 1.000000000000000000, -0.000000000000000000, -0.000000000000000000 ) ) ;
#27463 = FILL_AREA_STYLE ('',( #2619 ) ) ;
#27464 = VECTOR ( 'NONE', #13175, 1000.000000000000000 ) ;
#27465 = CARTESIAN_POINT ( 'NONE',  ( 65.00000000000001421, -28.31857036507964764, 80.03062855292515110 ) ) ;
#27466 = DIRECTION ( 'NONE',  ( 0.000000000000000000, -0.5000000000000001110, 0.8660254037844385966 ) ) ;
#27467 = VERTEX_POINT ( 'NONE', #21328 ) ;
#27468 = DIRECTION ( 'NONE',  ( -0.000000000000000000, 0.000000000000000000, -1.000000000000000000 ) ) ;
#27469 = DIRECTION ( 'NONE',  ( 0.000000000000000000, 0.000000000000000000, 1.000000000000000000 ) ) ;
#27470 = DIRECTION ( 'NONE',  ( 0.000000000000000000, 0.000000000000000000, -1.000000000000000000 ) ) ;
#27471 = DIRECTION ( 'NONE',  ( -1.000000000000000000, 0.000000000000000000, 0.000000000000000000 ) ) ;
#27472 = ITEM_DEFINED_TRANSFORMATION ( 'NONE', 'NONE', #6956,  #21307 ) ;
#27473 = LINE ( 'NONE', #10904, #12402 ) ;
#27474 = DIRECTION ( 'NONE',  ( 0.000000000000000000, 0.000000000000000000, 1.000000000000000000 ) ) ;
#27475 = AXIS2_PLACEMENT_3D ( 'NONE', #25676, #9451, #6397 ) ;
#27476 = ORIENTED_EDGE ( 'NONE', *, *, #7341, .T. ) ;
#27477 = CARTESIAN_POINT ( 'NONE',  ( 0.000000000000000000, 0.000000000000000000, 30.00000000000000000 ) ) ;
#27478 = CARTESIAN_POINT ( 'NONE',  ( 0.000000000000000000, 0.000000000000000000, 65.00000000000000000 ) ) ;
#27479 = CARTESIAN_POINT ( 'NONE',  ( 7.999999999999992895, 42.03146605346819342, -22.12489237027273603 ) ) ;
#27480 = ORIENTED_EDGE ( 'NONE', *, *, #9791, .F. ) ;
#27481 = CARTESIAN_POINT ( 'NONE',  ( -38.37230871539094323, -115.4561184093552413, 7.558975545821551734 ) ) ;
#27482 = CIRCLE ( 'NONE', #25829, 47.49900000000000944 ) ;
#27483 = ORIENTED_EDGE ( 'NONE', *, *, #33677, .T. ) ;
#27484 =( LENGTH_UNIT ( ) NAMED_UNIT ( * ) SI_UNIT ( .MILLI., .METRE. ) );
#27485 = ORIENTED_EDGE ( 'NONE', *, *, #13039, .T. ) ;
#27486 = ORIENTED_EDGE ( 'NONE', *, *, #18010, .F. ) ;
#27487 = CIRCLE ( 'NONE', #11941, 11.00000000000000000 ) ;
#27488 = FACE_OUTER_BOUND ( 'NONE', #28113, .T. ) ;
#27489 = EDGE_CURVE ( 'NONE', #5287, #29235, #29455, .T. ) ;
#27490 = AXIS2_PLACEMENT_3D ( 'NONE', #18720, #171, #32947 ) ;
#27491 = CARTESIAN_POINT ( 'NONE',  ( 7.999999999999992895, 46.87740477351717061, -3.172455868805379442 ) ) ;
#27492 = ORIENTED_EDGE ( 'NONE', *, *, #3623, .T. ) ;
#27493 = DIRECTION ( 'NONE',  ( 1.000000000000000000, 0.000000000000000000, -0.000000000000000000 ) ) ;
#27494 = DIRECTION ( 'NONE',  ( 0.000000000000000000, 0.000000000000000000, 1.000000000000000000 ) ) ;
#27495 = EDGE_CURVE ( 'NONE', #28348, #13216, #8355, .T. ) ;
#27496 = DIRECTION ( 'NONE',  ( 0.000000000000000000, -0.8090169943749534465, 0.5877852522924650325 ) ) ;
#27497 = VECTOR ( 'NONE', #15154, 1000.000000000000000 ) ;
#27498 = CARTESIAN_POINT ( 'NONE',  ( 0.000000000000000000, -19.60123832284014611, -3.973846525876633340 ) ) ;
#27499 = CARTESIAN_POINT ( 'NONE',  ( -9.999999999999994671, 0.000000000000000000, 0.000000000000000000 ) ) ;
#27500 = EDGE_CURVE ( 'NONE', #17844, #8765, #28494, .T. ) ;
#27501 = CYLINDRICAL_SURFACE ( 'NONE', #24359, 20.00000000000000355 ) ;
#27502 = AXIS2_PLACEMENT_3D ( 'NONE', #12246, #14926, #23219 ) ;
#27503 = CARTESIAN_POINT ( 'NONE',  ( -38.99924736195577424, -115.9929510916434481, 12.66759465831984599 ) ) ;
#27504 = DIRECTION ( 'NONE',  ( 0.000000000000000000, 0.3420201433256695456, -0.9396926207859079838 ) ) ;
#27505 = DIRECTION ( 'NONE',  ( -1.783119874454246424E-31, -1.187911941725854497E-31, 1.000000000000000000 ) ) ;
#27506 = LINE ( 'NONE', #2845, #23349 ) ;
#27507 = DIRECTION ( 'NONE',  ( 0.000000000000000000, 0.000000000000000000, 1.000000000000000000 ) ) ;
#27508 = CARTESIAN_POINT ( 'NONE',  ( 0.000000000000000000, -2.710505431213761085E-17, -45.00000000000000000 ) ) ;
#27509 = FACE_OUTER_BOUND ( 'NONE', #30630, .T. ) ;
#27510 = ORIENTED_EDGE ( 'NONE', *, *, #11507, .F. ) ;
#27511 = CARTESIAN_POINT ( 'NONE',  ( -36.52652403469559061, -114.9754527089670262, 2.777725545821551734 ) ) ;
#27512 = VECTOR ( 'NONE', #7357, 1000.000000000000000 ) ;
#27513 = CARTESIAN_POINT ( 'NONE',  ( 0.000000000000000000, 0.000000000000000000, 0.000000000000000000 ) ) ;
#27514 = CARTESIAN_POINT ( 'NONE',  ( 7.999999999999992895, 30.93515269692114344, 36.04401931830264516 ) ) ;
#27515 = EDGE_CURVE ( 'NONE', #2191, #128, #20413, .T. ) ;
#27516 = PLANE ( 'NONE',  #14197 ) ;
#27517 = EDGE_LOOP ( 'NONE', ( #1919, #7735, #7143, #26368 ) ) ;
#27518 = ORIENTED_EDGE ( 'NONE', *, *, #17854, .T. ) ;
#27519 = DIRECTION ( 'NONE',  ( -1.000000000000000000, 0.000000000000000000, 0.000000000000000000 ) ) ;
#27520 = LINE ( 'NONE', #27858, #27867 ) ;
#27521 = VERTEX_POINT ( 'NONE', #31965 ) ;
#27522 = ORIENTED_EDGE ( 'NONE', *, *, #24499, .F. ) ;
#27523 = EDGE_CURVE ( 'NONE', #21923, #16080, #14666, .T. ) ;
#27524 = DIRECTION ( 'NONE',  ( 0.000000000000000000, 0.000000000000000000, 1.000000000000000000 ) ) ;
#27525 = ADVANCED_FACE ( 'NONE', ( #17919 ), #15740, .F. ) ;
#27526 = DIRECTION ( 'NONE',  ( 0.000000000000000000, 0.000000000000000000, -1.000000000000000000 ) ) ;
#27527 = EDGE_CURVE ( 'NONE', #8147, #9312, #1549, .T. ) ;
#27528 = AXIS2_PLACEMENT_3D ( 'NONE', #21975, #2922, #10307 ) ;
#27529 = CARTESIAN_POINT ( 'NONE',  ( 45.10000000000000142, -2.710505431213722566E-17, -2.106485876673539214E-31 ) ) ;
#27530 = DIRECTION ( 'NONE',  ( -1.000000000000000000, 0.000000000000000000, 0.000000000000000000 ) ) ;
#27531 = ORIENTED_EDGE ( 'NONE', *, *, #10440, .F. ) ;
#27532 = ORIENTED_EDGE ( 'NONE', *, *, #2477, .T. ) ;
#27533 = AXIS2_PLACEMENT_3D ( 'NONE', #20435, #6780, #17752 ) ;
#27534 = DIRECTION ( 'NONE',  ( 1.000000000000000000, -0.000000000000000000, -0.000000000000000000 ) ) ;
#27535 = ADVANCED_FACE ( 'NONE', ( #12532 ), #23508, .T. ) ;
#27536 = LINE ( 'NONE', #2873, #13244 ) ;
#27537 = ORIENTED_EDGE ( 'NONE', *, *, #23187, .F. ) ;
#27538 = CARTESIAN_POINT ( 'NONE',  ( -9.999999999999994671, 0.000000000000000000, 0.000000000000000000 ) ) ;
#27539 = EDGE_CURVE ( 'NONE', #933, #7078, #9821, .T. ) ;
#27540 = CARTESIAN_POINT ( 'NONE',  ( -34.50000000000000000, -113.1807644833805426, -1.624782352598427959 ) ) ;
#27541 = CARTESIAN_POINT ( 'NONE',  ( -36.99999999999989342, -114.9929510916434339, 14.11852480586264846 ) ) ;
#27542 = CARTESIAN_POINT ( 'NONE',  ( -35.50000000000000000, -113.9929510916434339, 10.50625754673587409 ) ) ;
#27543 = FACE_OUTER_BOUND ( 'NONE', #35107, .T. ) ;
#27544 = CARTESIAN_POINT ( 'NONE',  ( -35.87745010033553683, -114.9929510916434339, 14.11371147303761298 ) ) ;
#27545 = DIRECTION ( 'NONE',  ( 0.000000000000000000, -0.8660254037844431485, 0.4999999999999921729 ) ) ;
#27546 = CARTESIAN_POINT ( 'NONE',  ( -50.00000000000000000, 10.00000000000000888, -15.00000000000000178 ) ) ;
#27547 = FACE_BOUND ( 'NONE', #31844, .T. ) ;
#27548 = CARTESIAN_POINT ( 'NONE',  ( -1.599999999999989653, -4.579597227308187024E-14, 6.765000000000020997 ) ) ;
#27549 = CARTESIAN_POINT ( 'NONE',  ( 115.0000000000000000, 81.48267994499606459, 30.15054357219658954 ) ) ;
#27550 = ORIENTED_EDGE ( 'NONE', *, *, #16095, .F. ) ;
#27551 = FACE_OUTER_BOUND ( 'NONE', #4400, .T. ) ;
#27552 = ORIENTED_EDGE ( 'NONE', *, *, #27641, .T. ) ;
#27553 = VECTOR ( 'NONE', #9488, 1000.000000000000227 ) ;
#27554 = CARTESIAN_POINT ( 'NONE',  ( -35.69809690994938478, -111.0245472910330022, 5.722274454178450043 ) ) ;
#27555 = DIRECTION ( 'NONE',  ( -1.000000000000000000, 0.000000000000000000, 0.000000000000000000 ) ) ;
#27556 = EDGE_CURVE ( 'NONE', #14069, #29093, #21587, .T. ) ;
#27557 = VERTEX_POINT ( 'NONE', #10369 ) ;
#27558 = AXIS2_PLACEMENT_3D ( 'NONE', #29790, #2262, #13228 ) ;
#27559 = ORIENTED_EDGE ( 'NONE', *, *, #21852, .T. ) ;
#27560 = DIRECTION ( 'NONE',  ( -1.226634733346697831E-16, -0.2588190451025240701, 0.9659258262890673130 ) ) ;
#27561 = PRODUCT_DEFINITION ( 'UNKNOWN', '', #1152, #21541 ) ;
#27562 = CARTESIAN_POINT ( 'NONE',  ( 8.000000000000000000, 17.56975900509174693, 9.555290079479316745 ) ) ;
#27563 = SHAPE_REPRESENTATION ( 'winch drum', ( #21307 ), #35148 ) ;
#27564 = ORIENTED_EDGE ( 'NONE', *, *, #9342, .F. ) ;
#27565 = CARTESIAN_POINT ( 'NONE',  ( -40.02454729103296671, -112.8166217158120332, 3.340225545821551290 ) ) ;
#27566 = DIRECTION ( 'NONE',  ( 0.000000000000000000, 0.6427876096865403621, -0.7660444431189771253 ) ) ;
#27567 = EDGE_CURVE ( 'NONE', #251, #17877, #15263, .T. ) ;
#27568 = DIRECTION ( 'NONE',  ( 0.000000000000000000, 0.000000000000000000, -1.000000000000000000 ) ) ;
#27569 = ORIENTED_EDGE ( 'NONE', *, *, #26992, .F. ) ;
#27570 = EDGE_LOOP ( 'NONE', ( #33348, #18672, #6946, #22602 ) ) ;
#27571 = ADVANCED_FACE ( 'NONE', ( #7477 ), #18456, .F. ) ;
#27572 = CARTESIAN_POINT ( 'NONE',  ( 7.999999999999992895, -30.03615769709705319, -42.44795908869020451 ) ) ;
#27573 = EDGE_CURVE ( 'NONE', #2870, #30988, #2284, .T. ) ;
#27574 = DIRECTION ( 'NONE',  ( 1.000000000000000000, 0.000000000000000000, 0.000000000000000000 ) ) ;
#27575 = VERTEX_POINT ( 'NONE', #13254 ) ;
#27576 = VERTEX_POINT ( 'NONE', #30161 ) ;
#27577 = CARTESIAN_POINT ( 'NONE',  ( -34.50000000000000000, -117.0140978167138854, -0.5622823525984408377 ) ) ;
#27578 = CIRCLE ( 'NONE', #10890, 52.00000000000000711 ) ;
#27579 = CYLINDRICAL_SURFACE ( 'NONE', #6428, 20.00000000000000355 ) ;
#27580 = ORIENTED_EDGE ( 'NONE', *, *, #8829, .F. ) ;
#27581 = CARTESIAN_POINT ( 'NONE',  ( -37.49414064056234253, -114.9929510916434339, 13.11852578240983291 ) ) ;
#27582 = ADVANCED_FACE ( 'NONE', ( #35579 ), #2818, .T. ) ;
#27583 = AXIS2_PLACEMENT_3D ( 'NONE', #26696, #5087, #21972 ) ;
#27584 = CARTESIAN_POINT ( 'NONE',  ( -34.51202277066418844, -113.9929510916434339, 12.81430620224972294 ) ) ;
#27585 = DIRECTION ( 'NONE',  ( 0.000000000000000000, 0.000000000000000000, 1.000000000000000000 ) ) ;
#27586 = DIRECTION ( 'NONE',  ( 0.000000000000000000, -0.6845471059286950544, 0.7289686274214053352 ) ) ;
#27587 = AXIS2_PLACEMENT_3D ( 'NONE', #8490, #25594, #207 ) ;
#27588 = CARTESIAN_POINT ( 'NONE',  ( -34.50000000000000000, -113.9929510916434339, 10.94631322572069365 ) ) ;
#27590 = CARTESIAN_POINT ( 'NONE',  ( -39.00000000000000711, -114.9929510916434339, 12.57451923796417503 ) ) ;
#27589 = VECTOR ( 'NONE', #26282, 1000.000000000000000 ) ;
#27591 = EDGE_CURVE ( 'NONE', #15523, #3873, #7827, .T. ) ;
#27592 = CARTESIAN_POINT ( 'NONE',  ( -35.50000000000000711, -114.0000000000003411, 9.500000000000035527 ) ) ;
#27593 = DIRECTION ( 'NONE',  ( -1.000000000000000000, -1.836970198721029934E-16, -0.000000000000000000 ) ) ;
#27594 = CARTESIAN_POINT ( 'NONE',  ( 0.000000000000000000, 0.000000000000000000, -43.60000000000000142 ) ) ;
#27595 = ORIENTED_EDGE ( 'NONE', *, *, #4931, .T. ) ;
#27596 = ORIENTED_EDGE ( 'NONE', *, *, #18972, .T. ) ;
#27597 = DIRECTION ( 'NONE',  ( -1.000000000000000000, 0.000000000000000000, 0.000000000000000000 ) ) ;
#27598 = CARTESIAN_POINT ( 'NONE',  ( -10.00000000000000178, 0.000000000000000000, 0.000000000000000000 ) ) ;
#27599 = EDGE_CURVE ( 'NONE', #14563, #31368, #27473, .T. ) ;
#27600 = ORIENTED_EDGE ( 'NONE', *, *, #6840, .T. ) ;
#27601 = DIRECTION ( 'NONE',  ( -1.000000000000000000, 0.000000000000000000, 0.000000000000000000 ) ) ;
#27602 = ORIENTED_EDGE ( 'NONE', *, *, #1521, .T. ) ;
#27603 = ADVANCED_FACE ( 'NONE', ( #257, #24230 ), #32861, .F. ) ;
#27604 = CARTESIAN_POINT ( 'NONE',  ( -35.50000000000000711, -116.0141056290913610, -0.5935324770972248976 ) ) ;
#27605 = LINE ( 'NONE', #21818, #24778 ) ;
#27606 = EDGE_CURVE ( 'NONE', #16063, #6941, #18814, .T. ) ;
#27607 = CARTESIAN_POINT ( 'NONE',  ( -36.52652403469556930, -113.0245472910329880, 5.722274454178450043 ) ) ;
#27608 = CARTESIAN_POINT ( 'NONE',  ( 1.566204647097418912, -6.822536405429468154, 0.000000000000000000 ) ) ;
#27609 = ORIENTED_EDGE ( 'NONE', *, *, #5011, .F. ) ;
#27610 = VECTOR ( 'NONE', #14004, 1000.000000000000000 ) ;
#27611 = DIRECTION ( 'NONE',  ( 0.000000000000000000, -0.5000000000000068834, 0.8660254037844347108 ) ) ;
#27612 = CARTESIAN_POINT ( 'NONE',  ( -35.50000000000000000, -115.1449503510569059, -2.621568770093253953 ) ) ;
#27613 = ORIENTED_EDGE ( 'NONE', *, *, #1964, .F. ) ;
#27614 = VERTEX_POINT ( 'NONE', #8353 ) ;
#27615 = EDGE_CURVE ( 'NONE', #35403, #30561, #29989, .T. ) ;
#27616 = CARTESIAN_POINT ( 'NONE',  ( -38.99999999999999289, -113.9407375970686900, 8.253524454178448266 ) ) ;
#27617 = VERTEX_POINT ( 'NONE', #4276 ) ;
#27618 = EDGE_CURVE ( 'NONE', #28712, #21743, #29817, .T. ) ;
#27619 = CIRCLE ( 'NONE', #5756, 20.00000000000000355 ) ;
#27620 = DIRECTION ( 'NONE',  ( -1.000000000000000000, 0.000000000000000000, 0.000000000000000000 ) ) ;
#27621 = EDGE_LOOP ( 'NONE', ( #27510, #23918, #15251, #32971 ) ) ;
#27622 = ORIENTED_EDGE ( 'NONE', *, *, #30527, .T. ) ;
#27623 = CARTESIAN_POINT ( 'NONE',  ( -34.50000000000000000, -112.0577668799241309, 1.173706424699810569 ) ) ;
#27624 = FACE_OUTER_BOUND ( 'NONE', #20890, .T. ) ;
#27625 = DIRECTION ( 'NONE',  ( -1.000000000000000000, 0.000000000000000000, 0.000000000000000000 ) ) ;
#27626 = CARTESIAN_POINT ( 'NONE',  ( -35.50000000000000000, -113.9929510916434339, 10.50625754673588474 ) ) ;
#27627 = DIRECTION ( 'NONE',  ( 1.000000000000000000, -0.000000000000000000, 0.000000000000000000 ) ) ;
#27628 = VECTOR ( 'NONE', #17720, 1000.000000000000000 ) ;
#27629 = CARTESIAN_POINT ( 'NONE',  ( -4.000000000000000000, 0.000000000000000000, -52.50000000000000000 ) ) ;
#27630 = CARTESIAN_POINT ( 'NONE',  ( -34.50000000000000000, -116.0060826362711595, -0.7553032835231661135 ) ) ;
#27631 = CARTESIAN_POINT ( 'NONE',  ( -38.42182118622945808, -115.9929510916434481, 13.81802396319329773 ) ) ;
#27632 = CARTESIAN_POINT ( 'NONE',  ( 7.999999999999992895, 0.000000000000000000, 0.000000000000000000 ) ) ;
#27633 = VECTOR ( 'NONE', #5914, 1000.000000000000000 ) ;
#27634 = DIRECTION ( 'NONE',  ( -1.000000000000000000, -0.000000000000000000, 0.000000000000000000 ) ) ;
#27635 = LINE ( 'NONE', #5314, #28434 ) ;
#27636 = EDGE_LOOP ( 'NONE', ( #3385, #4846, #11866, #14213, #30661 ) ) ;
#27637 = VECTOR ( 'NONE', #11590, 1000.000000000000000 ) ;
#27638 = CARTESIAN_POINT ( 'NONE',  ( -35.50000000000000711, -114.2305202833893816, 9.534416457224700991 ) ) ;
#27639 = DIRECTION ( 'NONE',  ( -1.000000000000000000, -1.387778780781445922E-16, -0.000000000000000000 ) ) ;
#27640 = CARTESIAN_POINT ( 'NONE',  ( -90.00000000000002842, 9.554310223899640008E-16, 4.980000000000024407 ) ) ;
#27641 = EDGE_CURVE ( 'NONE', #18294, #20350, #25047, .T. ) ;
#27642 = ORIENTED_EDGE ( 'NONE', *, *, #30440, .F. ) ;
#27643 = FACE_OUTER_BOUND ( 'NONE', #16273, .T. ) ;
#27644 = CARTESIAN_POINT ( 'NONE',  ( -42.49999999999999289, -20.32009476567239048, 97.80456345124112261 ) ) ;
#27645 = EDGE_CURVE ( 'NONE', #24892, #10989, #22719, .T. ) ;
#27646 = DIRECTION ( 'NONE',  ( 1.000000000000000000, 0.000000000000000000, 0.000000000000000000 ) ) ;
#27647 = DIRECTION ( 'NONE',  ( -1.000000000000000000, 0.000000000000000000, 0.000000000000000000 ) ) ;
#27648 = ITEM_DEFINED_TRANSFORMATION ( 'NONE', 'NONE', #6877,  #21307 ) ;
#27649 = CARTESIAN_POINT ( 'NONE',  ( 0.000000000000000000, 0.000000000000000000, 0.000000000000000000 ) ) ;
#27650 = DIRECTION ( 'NONE',  ( -1.000000000000000000, 0.000000000000000000, 0.000000000000000000 ) ) ;
#27651 = ORIENTED_EDGE ( 'NONE', *, *, #7360, .T. ) ;
#27652 = CARTESIAN_POINT ( 'NONE',  ( -4.000000000000000000, 0.000000000000000000, -65.00000000000000000 ) ) ;
#27653 = CARTESIAN_POINT ( 'NONE',  ( 8.000000000000000000, 14.80634052301623171, 8.177498406287277533 ) ) ;
#27654 = ORIENTED_EDGE ( 'NONE', *, *, #17897, .T. ) ;
#27655 = AXIS2_PLACEMENT_3D ( 'NONE', #19570, #14184, #19737 ) ;
#27656 = CARTESIAN_POINT ( 'NONE',  ( -36.94073759706868287, -115.0000000000000000, 5.871475545821551734 ) ) ;
#27657 = ORIENTED_EDGE ( 'NONE', *, *, #15880, .T. ) ;
#27658 =( NAMED_UNIT ( * ) PLANE_ANGLE_UNIT ( ) SI_UNIT ( $, .RADIAN. ) );
#27659 = ORIENTED_EDGE ( 'NONE', *, *, #26406, .T. ) ;
#27660 = AXIS2_PLACEMENT_3D ( 'NONE', #27674, #27505, #32525 ) ;
#27661 = VERTEX_POINT ( 'NONE', #18992 ) ;
#27662 = CARTESIAN_POINT ( 'NONE',  ( 50.00005079999998969, 14.30000000000000071, 3.000000000000002665 ) ) ;
#27663 = VECTOR ( 'NONE', #8136, 1000.000000000000114 ) ;
#27664 = LINE ( 'NONE', #105, #24288 ) ;
#27665 = AXIS2_PLACEMENT_3D ( 'NONE', #28051, #16327, #2868 ) ;
#27666 = FACE_OUTER_BOUND ( 'NONE', #16674, .T. ) ;
#27667 = DIRECTION ( 'NONE',  ( -1.174092375852890260E-15, 4.222049128630259891E-16, 1.000000000000000000 ) ) ;
#27668 = CARTESIAN_POINT ( 'NONE',  ( 50.00005079999998969, 1.347111479062088405E-15, -11.00000000000000000 ) ) ;
#27669 = DIRECTION ( 'NONE',  ( 0.000000000000000000, 0.000000000000000000, 1.000000000000000000 ) ) ;
#27670 = DIRECTION ( 'NONE',  ( -1.000000000000000000, 0.000000000000000000, 0.000000000000000000 ) ) ;
#27671 = DIRECTION ( 'NONE',  ( 1.000000000000000000, 5.551115123125782702E-16, 0.000000000000000000 ) ) ;
#27672 = CARTESIAN_POINT ( 'NONE',  ( -39.00000000000000000, -115.9929510916434481, 12.53051367006571937 ) ) ;
#27673 = LINE ( 'NONE', #19023, #28023 ) ;
#27674 = CARTESIAN_POINT ( 'NONE',  ( -6.938893903907228378E-15, 0.7408941433508786645, 0.000000000000000000 ) ) ;
#27675 = CARTESIAN_POINT ( 'NONE',  ( 70.00000000000001421, 46.40248769959372055, 64.62118051744215563 ) ) ;
#27676 = CARTESIAN_POINT ( 'NONE',  ( 70.00000000000001421, 81.48267994499606459, 30.15054357219658954 ) ) ;
#27677 = EDGE_CURVE ( 'NONE', #9355, #8056, #10717, .T. ) ;
#27678 = CARTESIAN_POINT ( 'NONE',  ( -90.00000000000002842, 0.000000000000000000, 6.938893903907228378E-15 ) ) ;
#27679 = CARTESIAN_POINT ( 'NONE',  ( -90.00000000000002842, 0.000000000000000000, 6.938893903907228378E-15 ) ) ;
#27680 = ORIENTED_EDGE ( 'NONE', *, *, #274, .T. ) ;
#27681 = AXIS2_PLACEMENT_3D ( 'NONE', #12442, #15118, #31348 ) ;
#27682 =( GEOMETRIC_REPRESENTATION_CONTEXT ( 3 ) GLOBAL_UNCERTAINTY_ASSIGNED_CONTEXT ( ( #12115 ) ) GLOBAL_UNIT_ASSIGNED_CONTEXT ( ( #4060, #4410, #28528 ) ) REPRESENTATION_CONTEXT ( 'NONE', 'WORKASPACE' ) );
#27683 = CARTESIAN_POINT ( 'NONE',  ( -35.00000000000000000, -113.9407375970686900, 6.996475545821551734 ) ) ;
#27684 = CIRCLE ( 'NONE', #2967, 8.000000000000001776 ) ;
#27685 = CARTESIAN_POINT ( 'NONE',  ( 7.999999999999992895, -31.08872492059985149, 41.68322423723089543 ) ) ;
#27686 = CARTESIAN_POINT ( 'NONE',  ( 8.000000000000000000, 11.06713717293261467, -13.55483219355716606 ) ) ;
#27687 = LINE ( 'NONE', #19890, #1508 ) ;
#27688 = ORIENTED_EDGE ( 'NONE', *, *, #6696, .F. ) ;
#27689 = ORIENTED_EDGE ( 'NONE', *, *, #10106, .F. ) ;
#27691 = DIRECTION ( 'NONE',  ( 1.000000000000000000, 0.000000000000000000, 0.000000000000000000 ) ) ;
#27690 = PRODUCT_DEFINITION_SHAPE ( 'NONE', 'NONE',  #35655 ) ;
#27692 = CYLINDRICAL_SURFACE ( 'NONE', #14053, 15.49899999999998457 ) ;
#27693 = VERTEX_POINT ( 'NONE', #21686 ) ;
#27694 = ADVANCED_FACE ( 'NONE', ( #8009 ), #5499, .T. ) ;
#27695 = EDGE_LOOP ( 'NONE', ( #32172, #13915, #539, #20703 ) ) ;
#27696 = DIRECTION ( 'NONE',  ( -1.000000000000000000, -0.000000000000000000, 0.000000000000000000 ) ) ;
#27697 = CARTESIAN_POINT ( 'NONE',  ( 3.799999999999999822, 0.000000000000000000, -44.50000000000000000 ) ) ;
#27698 = AXIS2_PLACEMENT_3D ( 'NONE', #21521, #13448, #29655 ) ;
#27699 = DIRECTION ( 'NONE',  ( -1.000000000000000000, 7.806255641895633157E-17, -2.465190328815661892E-32 ) ) ;
#27700 = CYLINDRICAL_SURFACE ( 'NONE', #30573, 15.49899999999998457 ) ;
#27701 = VERTEX_POINT ( 'NONE', #24764 ) ;
#27702 = EDGE_LOOP ( 'NONE', ( #20926, #20826, #1662, #33927 ) ) ;
#27703 = PLANE ( 'NONE',  #26065 ) ;
#27704 = FACE_OUTER_BOUND ( 'NONE', #17934, .T. ) ;
#27705 = CIRCLE ( 'NONE', #1856, 8.000000000000005329 ) ;
#27706 = ORIENTED_EDGE ( 'NONE', *, *, #17350, .T. ) ;
#27707 = AXIS2_PLACEMENT_3D ( 'NONE', #26774, #7324, #20981 ) ;
#27708 = DIRECTION ( 'NONE',  ( 0.000000000000000000, 0.000000000000000000, -1.000000000000000000 ) ) ;
#27709 = CARTESIAN_POINT ( 'NONE',  ( -34.50000000000000000, -115.6286452741999113, -1.424448457485488095 ) ) ;
#27710 = CARTESIAN_POINT ( 'NONE',  ( -37.46874999999996447, -114.9929510916434339, 14.11852480586264846 ) ) ;
#27711 = CARTESIAN_POINT ( 'NONE',  ( -35.50000000000000000, -113.9929510916434339, 10.50625754673586876 ) ) ;
#27712 = CARTESIAN_POINT ( 'NONE',  ( 7.999999999999992895, 46.87740477351717061, -3.172455868805379442 ) ) ;
#27713 = CARTESIAN_POINT ( 'NONE',  ( -36.24999999999983658, -114.9929510916434339, 14.11852480586264846 ) ) ;
#27714 = CARTESIAN_POINT ( 'NONE',  ( 4.872650870659763989, 0.4273491293402877367, -0.8000000000000009326 ) ) ;
#27715 = ORIENTED_EDGE ( 'NONE', *, *, #8066, .T. ) ;
#27716 = CARTESIAN_POINT ( 'NONE',  ( 8.000000000000000000, 15.46619997295642079, 1.007799283846740002 ) ) ;
#27717 = DIRECTION ( 'NONE',  ( 2.668805347656626185E-16, -1.000000000000000000, 0.000000000000000000 ) ) ;
#27718 = DIRECTION ( 'NONE',  ( 0.000000000000000000, 0.000000000000000000, -1.000000000000000000 ) ) ;
#27719 = LINE ( 'NONE', #27887, #2007 ) ;
#27720 = ADVANCED_FACE ( 'NONE', ( #2987 ), #88, .T. ) ;
#27721 = ORIENTED_EDGE ( 'NONE', *, *, #13924, .F. ) ;
#27722 = ADVANCED_FACE ( 'NONE', ( #33038, #13947 ), #24935, .F. ) ;
#27723 = CARTESIAN_POINT ( 'NONE',  ( -38.00000000000000711, -114.9929510916434339, 11.73841344789285657 ) ) ;
#27724 = ORIENTED_EDGE ( 'NONE', *, *, #26717, .F. ) ;
#27725 = CARTESIAN_POINT ( 'NONE',  ( -39.99999999999999289, -113.9407375970686758, 6.753524454178450043 ) ) ;
#27726 = LINE ( 'NONE', #19754, #28518 ) ;
#27727 = CARTESIAN_POINT ( 'NONE',  ( -35.50000000000000711, -116.0060826362711595, -0.7553032835231661135 ) ) ;
#27728 = ORIENTED_EDGE ( 'NONE', *, *, #31287, .T. ) ;
#27729 = EDGE_LOOP ( 'NONE', ( #797, #15838, #32849, #12167 ) ) ;
#27730 = DIRECTION ( 'NONE',  ( -1.000000000000000000, 0.000000000000000000, 0.000000000000000000 ) ) ;
#27731 = DIRECTION ( 'NONE',  ( 0.000000000000000000, 0.000000000000000000, -1.000000000000000000 ) ) ;
#27732 = EDGE_CURVE ( 'NONE', #18475, #35360, #29061, .T. ) ;
#27733 = ORIENTED_EDGE ( 'NONE', *, *, #30436, .T. ) ;
#27734 = CIRCLE ( 'NONE', #9906, 22.00000000000000000 ) ;
#27735 = EDGE_CURVE ( 'NONE', #21409, #31574, #9071, .T. ) ;
#27736 = FACE_OUTER_BOUND ( 'NONE', #16885, .T. ) ;
#27737 = DIRECTION ( 'NONE',  ( -1.000000000000000000, 0.000000000000000000, 0.000000000000000000 ) ) ;
#27738 = ORIENTED_EDGE ( 'NONE', *, *, #2245, .T. ) ;
#27739 = ORIENTED_EDGE ( 'NONE', *, *, #25596, .T. ) ;
#27740 = DIRECTION ( 'NONE',  ( 1.000000000000000000, -5.339440136655842133E-16, -1.047965281155519420E-16 ) ) ;
#27741 = DIRECTION ( 'NONE',  ( 0.000000000000000000, -6.938893903907202493E-17, -1.000000000000000000 ) ) ;
#27742 = EDGE_LOOP ( 'NONE', ( #4801, #15200, #18828, #27303 ) ) ;
#27743 = EDGE_LOOP ( 'NONE', ( #26643, #33261, #10390, #9529 ) ) ;
#27744 = CIRCLE ( 'NONE', #30613, 8.000000000000014211 ) ;
#27745 = CARTESIAN_POINT ( 'NONE',  ( -35.50000000000000000, -113.5133328644208746, 2.949007337991939259 ) ) ;
#27746 = CARTESIAN_POINT ( 'NONE',  ( 8.000000000000000000, -8.605879768205326741, 12.89022243466705930 ) ) ;
#27747 = ORIENTED_EDGE ( 'NONE', *, *, #34331, .T. ) ;
#27748 = CARTESIAN_POINT ( 'NONE',  ( -35.96730626674924025, -114.9929510916434339, 13.11752178341330044 ) ) ;
#27749 = ADVANCED_FACE ( 'NONE', ( #19847 ), #31212, .F. ) ;
#27750 = CARTESIAN_POINT ( 'NONE',  ( -36.24999999999983658, -113.9929510916434339, 14.11852480586265024 ) ) ;
#27751 = AXIS2_PLACEMENT_3D ( 'NONE', #5787, #25406, #16744 ) ;
#27752 = DIRECTION ( 'NONE',  ( 0.02857142857143298714, -0.9995917534020514195, -4.555780455966493806E-16 ) ) ;
#27753 = CYLINDRICAL_SURFACE ( 'NONE', #2473, 1.000000000000000888 ) ;
#27754 = VECTOR ( 'NONE', #24378, 1000.000000000000000 ) ;
#27755 = CARTESIAN_POINT ( 'NONE',  ( -34.50000000000000000, -113.9929510916434339, 10.50625754673588474 ) ) ;
#27756 = CARTESIAN_POINT ( 'NONE',  ( -39.00000000000000711, -114.9929510916434339, 12.26648026267477043 ) ) ;
#27757 = CARTESIAN_POINT ( 'NONE',  ( -35.50000000000000711, -114.9929510916434339, 10.52826033068511435 ) ) ;
#27758 = CARTESIAN_POINT ( 'NONE',  ( 0.000000000000000000, 0.000000000000000000, 55.00000000000000000 ) ) ;
#27759 = FACE_OUTER_BOUND ( 'NONE', #14149, .T. ) ;
#27760 = ADVANCED_FACE ( 'NONE', ( #17157 ), #33737, .T. ) ;
#27761 = ORIENTED_EDGE ( 'NONE', *, *, #23845, .F. ) ;
#27762 = EDGE_CURVE ( 'NONE', #33416, #2210, #18119, .T. ) ;
#27763 = ORIENTED_EDGE ( 'NONE', *, *, #1409, .T. ) ;
#27764 = EDGE_CURVE ( 'NONE', #9689, #30873, #8969, .T. ) ;
#27765 = LINE ( 'NONE', #3105, #1699 ) ;
#27766 = CARTESIAN_POINT ( 'NONE',  ( 46.00000000000000000, 0.000000000000000000, 0.000000000000000000 ) ) ;
#27767 = ORIENTED_EDGE ( 'NONE', *, *, #11957, .T. ) ;
#27768 = CIRCLE ( 'NONE', #23749, 4.000000000000000000 ) ;
#27769 = CARTESIAN_POINT ( 'NONE',  ( 0.000000000000000000, 0.000000000000000000, 0.000000000000000000 ) ) ;
#27770 = ORIENTED_EDGE ( 'NONE', *, *, #24081, .T. ) ;
#27771 = VECTOR ( 'NONE', #22414, 1000.000000000000000 ) ;
#27772 = AXIS2_PLACEMENT_3D ( 'NONE', #30510, #8702, #429 ) ;
#27773 = CARTESIAN_POINT ( 'NONE',  ( -35.50000000000000000, -113.0256022645180707, 0.8765908897032291813 ) ) ;
#27774 = CARTESIAN_POINT ( 'NONE',  ( 46.00000000000000000, -25.98076211353320275, 84.99999999999992895 ) ) ;
#27775 = CARTESIAN_POINT ( 'NONE',  ( -39.02454729103295961, -114.7691647218148745, 2.159774454178448710 ) ) ;
#27776 = EDGE_CURVE ( 'NONE', #24590, #18097, #28166, .T. ) ;
#27777 = CARTESIAN_POINT ( 'NONE',  ( 8.000000000000000000, -14.87816164169111310, -4.342730381190021305 ) ) ;
#27778 = EDGE_CURVE ( 'NONE', #35237, #5386, #25289, .T. ) ;
#27779 = EDGE_LOOP ( 'NONE', ( #19069, #1513, #5924, #22894 ) ) ;
#27780 = CIRCLE ( 'NONE', #7630, 3.799999999999999822 ) ;
#27781 = CARTESIAN_POINT ( 'NONE',  ( -35.50000000000000711, -112.8655373925166572, 1.864575885149403423 ) ) ;
#27782 = CIRCLE ( 'NONE', #4219, 47.49900000000000944 ) ;
#27783 = ORIENTED_EDGE ( 'NONE', *, *, #7362, .F. ) ;
#27784 = ORIENTED_EDGE ( 'NONE', *, *, #66, .F. ) ;
#27785 = CARTESIAN_POINT ( 'NONE',  ( -37.05926240293131713, -115.9999999999999858, 6.378524454178448266 ) ) ;
#27786 = AXIS2_PLACEMENT_3D ( 'NONE', #22749, #34103, #22928 ) ;
#27787 =( LENGTH_UNIT ( ) NAMED_UNIT ( * ) SI_UNIT ( .MILLI., .METRE. ) );
#27788 = CARTESIAN_POINT ( 'NONE',  ( 0.000000000000000000, 0.000000000000000000, -31.10000000000000142 ) ) ;
#27789 = ORIENTED_EDGE ( 'NONE', *, *, #21313, .F. ) ;
#27790 = ORIENTED_EDGE ( 'NONE', *, *, #4310, .T. ) ;
#27791 = CARTESIAN_POINT ( 'NONE',  ( -34.50000000000000000, -112.3465879560236687, 1.629585756119413364 ) ) ;
#27792 = CYLINDRICAL_SURFACE ( 'NONE', #32691, 7.199999999999993960 ) ;
#27793 = DIRECTION ( 'NONE',  ( 1.000000000000000000, 1.836970198721029934E-16, 0.000000000000000000 ) ) ;
#27794 = EDGE_CURVE ( 'NONE', #11433, #15563, #7817, .T. ) ;
#27795 = CARTESIAN_POINT ( 'NONE',  ( -35.50000000000000000, -113.9929510916434339, 10.59426868253284226 ) ) ;
#27796 = AXIS2_PLACEMENT_3D ( 'NONE', #24658, #25321, #17543 ) ;
#27797 = EDGE_CURVE ( 'NONE', #21788, #32680, #14135, .T. ) ;
#27798 = LINE ( 'NONE', #3134, #21876 ) ;
#27799 = DIRECTION ( 'NONE',  ( 0.000000000000000000, -0.1253332335642905193, -0.9921147013144796523 ) ) ;
#27800 = ADVANCED_FACE ( 'NONE', ( #22743 ), #3153, .F. ) ;
#27801 = CARTESIAN_POINT ( 'NONE',  ( -34.50000000000000000, -115.6286452741999113, -1.424448457485488095 ) ) ;
#27802 = CARTESIAN_POINT ( 'NONE',  ( -39.00000000000000000, -115.9929510916434481, 12.60752341388803721 ) ) ;
#27803 = CARTESIAN_POINT ( 'NONE',  ( 7.999999999999992895, 46.19362259308845609, -8.585149169757999132 ) ) ;
#27805 = AXIS2_PLACEMENT_3D ( 'NONE', #21279, #29408, #21453 ) ;
#27804 = CARTESIAN_POINT ( 'NONE',  ( -90.00000000000002842, -5.551115123125799465E-16, -8.000000000000044409 ) ) ;
#27806 = CIRCLE ( 'NONE', #13438, 3.799999999999999822 ) ;
#27807 = ADVANCED_FACE ( 'NONE', ( #22389, #22922 ), #8706, .F. ) ;
#27808 = ORIENTED_EDGE ( 'NONE', *, *, #24591, .F. ) ;
#27809 = CARTESIAN_POINT ( 'NONE',  ( -34.49999999999998579, 0.4463568765849662556, 113.0433323525902125 ) ) ;
#27810 = EDGE_CURVE ( 'NONE', #27376, #584, #21019, .T. ) ;
#27811 = CARTESIAN_POINT ( 'NONE',  ( -4.000000000000000000, 0.000000000000000000, 55.00000000000000000 ) ) ;
#27812 = ORIENTED_EDGE ( 'NONE', *, *, #15864, .F. ) ;
#27813 = CARTESIAN_POINT ( 'NONE',  ( -34.49999999999998579, -12.00833024919777081, 94.79903810567661537 ) ) ;
#27814 = CARTESIAN_POINT ( 'NONE',  ( 7.999999999999992895, 46.87740477351717061, -3.172455868805379442 ) ) ;
#27815 = DIRECTION ( 'NONE',  ( -0.000000000000000000, 0.000000000000000000, -1.000000000000000000 ) ) ;
#27816 = FACE_OUTER_BOUND ( 'NONE', #10541, .T. ) ;
#27817 = DIRECTION ( 'NONE',  ( 0.000000000000000000, -1.000000000000000000, 0.000000000000000000 ) ) ;
#27818 = CARTESIAN_POINT ( 'NONE',  ( 7.999999999999992895, -35.20873326984104068, 31.88259874184018372 ) ) ;
#27819 = CIRCLE ( 'NONE', #13446, 7.800000000000051337 ) ;
#27820 = EDGE_LOOP ( 'NONE', ( #30523, #655, #396, #12575 ) ) ;
#27821 = AXIS2_PLACEMENT_3D ( 'NONE', #32846, #35563, #10886 ) ;
#27822 = FACE_OUTER_BOUND ( 'NONE', #13442, .T. ) ;
#27823 = LINE ( 'NONE', #16641, #16537 ) ;
#27824 = LINE ( 'NONE', #3160, #24339 ) ;
#27825 = EDGE_LOOP ( 'NONE', ( #11081, #5849, #4565, #14056 ) ) ;
#27826 = CARTESIAN_POINT ( 'NONE',  ( -36.33479806579560289, -113.2509883718313262, 3.808975545821551734 ) ) ;
#27827 = EDGE_LOOP ( 'NONE', ( #33830, #6810, #895, #10782 ) ) ;
#27828 = ORIENTED_EDGE ( 'NONE', *, *, #3793, .F. ) ;
#27829 = VERTEX_POINT ( 'NONE', #31388 ) ;
#27830 = FACE_OUTER_BOUND ( 'NONE', #34145, .T. ) ;
#27831 = AXIS2_PLACEMENT_3D ( 'NONE', #19941, #30597, #27899 ) ;
#27832 = CARTESIAN_POINT ( 'NONE',  ( 0.000000000000000000, -2.912696353505970226, 21.80633394113446499 ) ) ;
#27833 = EDGE_CURVE ( 'NONE', #15509, #9289, #13562, .T. ) ;
#27834 = DIRECTION ( 'NONE',  ( -1.000000000000000000, 0.000000000000000000, -0.000000000000000000 ) ) ;
#27835 = ADVANCED_FACE ( 'NONE', ( #20203 ), #6196, .T. ) ;
#27836 = CARTESIAN_POINT ( 'NONE',  ( -35.50000000000000711, -114.1189822439768449, 9.514224058074130852 ) ) ;
#27837 = DIRECTION ( 'NONE',  ( -1.174092375852890260E-15, 4.222049128630259891E-16, 1.000000000000000000 ) ) ;
#27838 = LINE ( 'NONE', #24959, #17711 ) ;
#27839 = CARTESIAN_POINT ( 'NONE',  ( -34.50000000000000000, -114.0371586325023117, 9.504435485030890973 ) ) ;
#27840 = DIRECTION ( 'NONE',  ( -1.836970198721029934E-16, 1.000000000000000000, 0.000000000000000000 ) ) ;
#27841 = CARTESIAN_POINT ( 'NONE',  ( -3.799999999999999822, 4.382607293638566128E-16, 30.00000000000000000 ) ) ;
#27842 = CARTESIAN_POINT ( 'NONE',  ( -36.99999999999988631, -115.9929510916434481, 14.11852480586265024 ) ) ;
#27843 = DIRECTION ( 'NONE',  ( 1.000000000000000000, 0.000000000000000000, 0.000000000000000000 ) ) ;
#27844 = CARTESIAN_POINT ( 'NONE',  ( 8.000000000000007105, 0.000000000000000000, 0.000000000000000000 ) ) ;
#27845 = FACE_OUTER_BOUND ( 'NONE', #33839, .T. ) ;
#27846 = LINE ( 'NONE', #13977, #18114 ) ;
#27847 = AXIS2_PLACEMENT_3D ( 'NONE', #30146, #5483, #13763 ) ;
#27848 = DIRECTION ( 'NONE',  ( 1.000000000000000000, 0.000000000000000000, 0.000000000000000000 ) ) ;
#27849 = DIRECTION ( 'NONE',  ( -1.000000000000000000, 0.000000000000000000, 0.000000000000000000 ) ) ;
#27850 = EDGE_LOOP ( 'NONE', ( #22755, #23510, #30409, #11401 ) ) ;
#27851 = CARTESIAN_POINT ( 'NONE',  ( -36.23083527818512550, -111.9754527089670404, 9.715225545821551734 ) ) ;
#27852 = DIRECTION ( 'NONE',  ( -1.000000000000000000, 0.000000000000000000, 0.000000000000000000 ) ) ;
#27853 = DIRECTION ( 'NONE',  ( 0.000000000000000000, 0.9672551082808337197, -0.2538061376417689030 ) ) ;
#27854 = DIRECTION ( 'NONE',  ( 0.000000000000000000, 0.000000000000000000, 1.000000000000000000 ) ) ;
#27855 = ORIENTED_EDGE ( 'NONE', *, *, #29106, .T. ) ;
#27856 = ORIENTED_EDGE ( 'NONE', *, *, #25997, .F. ) ;
#27857 = LINE ( 'NONE', #305, #3300 ) ;
#27858 = CARTESIAN_POINT ( 'NONE',  ( -42.49999999999999289, -25.01350700525237514, 84.74619386235816876 ) ) ;
#27859 = VERTEX_POINT ( 'NONE', #30691 ) ;
#27860 = ORIENTED_EDGE ( 'NONE', *, *, #7714, .F. ) ;
#27861 = DIRECTION ( 'NONE',  ( 0.000000000000000000, 0.000000000000000000, 1.000000000000000000 ) ) ;
#27862 = CYLINDRICAL_SURFACE ( 'NONE', #5073, 17.49900000000000233 ) ;
#27863 = PRODUCT_CONTEXT ( 'NONE', #3200, 'mechanical' ) ;
#27864 = CARTESIAN_POINT ( 'NONE',  ( -39.49999999999999289, -11.24969279549607748, 111.5585998451919778 ) ) ;
#27865 = VERTEX_POINT ( 'NONE', #6722 ) ;
#27866 = ORIENTED_EDGE ( 'NONE', *, *, #28201, .T. ) ;
#27867 = VECTOR ( 'NONE', #2858, 1000.000000000000114 ) ;
#27868 = EDGE_CURVE ( 'NONE', #31582, #17845, #6538, .T. ) ;
#27869 = AXIS2_PLACEMENT_3D ( 'NONE', #13850, #33116, #19928 ) ;
#27870 = CARTESIAN_POINT ( 'NONE',  ( 0.000000000000000000, -2.710505431213761085E-17, -30.90000000000000568 ) ) ;
#27871 = DIRECTION ( 'NONE',  ( -1.000000000000000000, 0.000000000000000000, 0.000000000000000000 ) ) ;
#27872 = VERTEX_POINT ( 'NONE', #6019 ) ;
#27873 = CARTESIAN_POINT ( 'NONE',  ( 8.000000000000007105, -13.42368113696662490, -3.975523202428152381 ) ) ;
#27874 = CIRCLE ( 'NONE', #5448, 6.984000000000015085 ) ;
#27875 = DIRECTION ( 'NONE',  ( -1.000000000000000000, 0.000000000000000000, 0.000000000000000000 ) ) ;
#27876 = CYLINDRICAL_SURFACE ( 'NONE', #23632, 22.00000000000000000 ) ;
#27877 = CARTESIAN_POINT ( 'NONE',  ( -34.50000000000000000, -114.1835524127412924, 8.514811007161055656 ) ) ;
#27878 = DIRECTION ( 'NONE',  ( 0.000000000000000000, 0.000000000000000000, -1.000000000000000000 ) ) ;
#27879 = DIRECTION ( 'NONE',  ( 0.000000000000000000, 0.000000000000000000, 1.000000000000000000 ) ) ;
#27880 = EDGE_CURVE ( 'NONE', #4678, #34729, #3335, .T. ) ;
#27881 = CARTESIAN_POINT ( 'NONE',  ( -36.87500000000098055, -114.9929510916434339, 14.11852480586264846 ) ) ;
#27882 = DIRECTION ( 'NONE',  ( -1.000000000000000000, 0.000000000000000000, 0.000000000000000000 ) ) ;
#27883 = DIRECTION ( 'NONE',  ( 0.000000000000000000, -0.9980267284282722251, 0.06279051952930256308 ) ) ;
#27884 = AXIS2_PLACEMENT_3D ( 'NONE', #34262, #28689, #34453 ) ;
#27885 = LINE ( 'NONE', #3229, #33064 ) ;
#27886 = CARTESIAN_POINT ( 'NONE',  ( 4.000000000000003553, -43.55304910509426009, 28.41006711799970574 ) ) ;
#27887 = CARTESIAN_POINT ( 'NONE',  ( 4.000000000000003553, -13.56094713063606072, 50.20060470671736397 ) ) ;
#27888 = ORIENTED_EDGE ( 'NONE', *, *, #2228, .T. ) ;
#27889 = DIRECTION ( 'NONE',  ( -1.000000000000000000, 0.000000000000000000, 0.000000000000000000 ) ) ;
#27890 = ORIENTED_EDGE ( 'NONE', *, *, #7670, .F. ) ;
#27891 = CARTESIAN_POINT ( 'NONE',  ( -33.97545270896702618, -112.8166217158120475, 7.409774454178449155 ) ) ;
#27892 = DIRECTION ( 'NONE',  ( 1.000000000000000000, -5.339440136655842133E-16, -1.047965281155519420E-16 ) ) ;
#27893 = CARTESIAN_POINT ( 'NONE',  ( -35.50000000000000711, -112.7549084230351752, -1.592823285203595285 ) ) ;
#27894 = VERTEX_POINT ( 'NONE', #28701 ) ;
#27895 = ORIENTED_EDGE ( 'NONE', *, *, #27190, .F. ) ;
#27896 = CIRCLE ( 'NONE', #3739, 4.872650870659778199 ) ;
#27897 = LINE ( 'NONE', #12040, #23463 ) ;
#27898 = AXIS2_PLACEMENT_3D ( 'NONE', #33780, #34134, #14669 ) ;
#27899 = DIRECTION ( 'NONE',  ( 0.000000000000000000, 0.000000000000000000, 1.000000000000000000 ) ) ;
#27900 = EDGE_LOOP ( 'NONE', ( #4097, #26945, #29388, #23739 ) ) ;
#27901 = VECTOR ( 'NONE', #17376, 1000.000000000000000 ) ;
#27902 = CYLINDRICAL_SURFACE ( 'NONE', #10951, 17.49900000000000233 ) ;
#27903 = DIRECTION ( 'NONE',  ( 1.000000000000000000, 0.000000000000000000, 0.000000000000000000 ) ) ;
#27904 = VERTEX_POINT ( 'NONE', #9607 ) ;
#27905 = ORIENTED_EDGE ( 'NONE', *, *, #15901, .T. ) ;
#27906 = CARTESIAN_POINT ( 'NONE',  ( 7.999999999999992895, 0.000000000000000000, 0.000000000000000000 ) ) ;
#27907 = DIRECTION ( 'NONE',  ( -0.000000000000000000, 0.000000000000000000, -1.000000000000000000 ) ) ;
#27909 = ORIENTED_EDGE ( 'NONE', *, *, #7312, .T. ) ;
#27908 = CIRCLE ( 'NONE', #28500, 7.199999999999998401 ) ;
#27910 = ORIENTED_EDGE ( 'NONE', *, *, #28625, .F. ) ;
#27911 = CARTESIAN_POINT ( 'NONE',  ( -34.50000000000000000, -117.0140978167138854, -0.4997823525984417259 ) ) ;
#27912 = EDGE_CURVE ( 'NONE', #8310, #32263, #19297, .T. ) ;
#27913 = EDGE_CURVE ( 'NONE', #24278, #1617, #4049, .T. ) ;
#27914 = VERTEX_POINT ( 'NONE', #34814 ) ;
#27915 = CARTESIAN_POINT ( 'NONE',  ( -35.98364338251434447, -114.9929510916434339, 13.11827392651456314 ) ) ;
#27916 = CARTESIAN_POINT ( 'NONE',  ( -36.99999999999988631, -113.9929510916434339, 14.11852480586265024 ) ) ;
#27917 = VECTOR ( 'NONE', #10714, 1000.000000000000114 ) ;
#27918 = DIRECTION ( 'NONE',  ( -1.000000000000000000, 0.000000000000000000, -0.000000000000000000 ) ) ;
#27919 = DIRECTION ( 'NONE',  ( 1.000000000000000000, -4.524158825347490025E-15, -1.174092375852883357E-15 ) ) ;
#27920 = EDGE_CURVE ( 'NONE', #24278, #9536, #34276, .T. ) ;
#27921 = CARTESIAN_POINT ( 'NONE',  ( -34.50000000000000000, -113.9929510916434339, 10.59426868253284226 ) ) ;
#27922 = CARTESIAN_POINT ( 'NONE',  ( 8.000000000000000000, -18.62763138773852134, 10.49404041845529001 ) ) ;
#27923 = AXIS2_PLACEMENT_3D ( 'NONE', #15149, #1489, #17501 ) ;
#27924 = AXIS2_PLACEMENT_3D ( 'NONE', #11243, #8538, #5847 ) ;
#27925 = CARTESIAN_POINT ( 'NONE',  ( -35.50000000000000711, -114.1264797827112574, 9.515205387299289441 ) ) ;
#27926 = VECTOR ( 'NONE', #22356, 1000.000000000000000 ) ;
#27927 = DIRECTION ( 'NONE',  ( -1.000000000000000000, 0.000000000000000000, -0.000000000000000000 ) ) ;
#27928 = ORIENTED_EDGE ( 'NONE', *, *, #28005, .F. ) ;
#27929 = ORIENTED_EDGE ( 'NONE', *, *, #26466, .F. ) ;
#27930 = CARTESIAN_POINT ( 'NONE',  ( 7.999999999999992895, 0.000000000000000000, 0.000000000000000000 ) ) ;
#27931 = DIRECTION ( 'NONE',  ( -1.000000000000000000, 0.000000000000000000, 0.000000000000000000 ) ) ;
#27932 = CIRCLE ( 'NONE', #7803, 3.799999999999999822 ) ;
#27933 = VERTEX_POINT ( 'NONE', #26169 ) ;
#27934 = DIRECTION ( 'NONE',  ( 0.02857142857143298367, -0.9995917534020514195, -4.555780455966494792E-16 ) ) ;
#27935 = EDGE_LOOP ( 'NONE', ( #11740, #4273, #33681, #8282 ) ) ;
#27936 = CARTESIAN_POINT ( 'NONE',  ( -35.50000000000000000, -115.0140978167138712, -0.6247823525984407267 ) ) ;
#27937 = CARTESIAN_POINT ( 'NONE',  ( 0.000000000000000000, 0.000000000000000000, 0.000000000000000000 ) ) ;
#27938 = CARTESIAN_POINT ( 'NONE',  ( -39.02454729103295961, -114.7691647218148745, 3.659774454178448710 ) ) ;
#27939 = ORIENTED_EDGE ( 'NONE', *, *, #24184, .F. ) ;
#27940 = CARTESIAN_POINT ( 'NONE',  ( 5.400000000000085620, -1.000000000000049516, -32.00000000000000000 ) ) ;
#27941 = EDGE_CURVE ( 'NONE', #28491, #403, #25995, .T. ) ;
#27942 = ORIENTED_EDGE ( 'NONE', *, *, #24682, .T. ) ;
#27943 = DIRECTION ( 'NONE',  ( -1.000000000000000000, 0.000000000000000000, 0.000000000000000000 ) ) ;
#27944 = VECTOR ( 'NONE', #16760, 1000.000000000000000 ) ;
#27945 = CARTESIAN_POINT ( 'NONE',  ( -35.50000000000000000, -117.0140978167138854, 0.3752176474015736507 ) ) ;
#27946 = ORIENTED_EDGE ( 'NONE', *, *, #9445, .T. ) ;
#27947 = ORIENTED_EDGE ( 'NONE', *, *, #17166, .T. ) ;
#27948 = CARTESIAN_POINT ( 'NONE',  ( 4.000000000000003553, -50.95304419620832448, 10.38206564895643957 ) ) ;
#27949 = VECTOR ( 'NONE', #29047, 1000.000000000000000 ) ;
#27950 = CARTESIAN_POINT ( 'NONE',  ( 8.000000000000000000, 0.000000000000000000, 17.49900000000000233 ) ) ;
#27951 = ORIENTED_EDGE ( 'NONE', *, *, #19723, .T. ) ;
#27952 = ORIENTED_EDGE ( 'NONE', *, *, #26420, .T. ) ;
#27953 = CARTESIAN_POINT ( 'NONE',  ( -34.50000000000000000, -112.9415908020655195, 1.873661708251232572 ) ) ;
#27954 = CIRCLE ( 'NONE', #34278, 4.000000000000000000 ) ;
#27955 = DIRECTION ( 'NONE',  ( 0.000000000000000000, 0.3681245526846719240, 0.9297764858882537897 ) ) ;
#27956 = EDGE_CURVE ( 'NONE', #3344, #30739, #25646, .T. ) ;
#27957 = ADVANCED_FACE ( 'NONE', ( #1503 ), #23470, .F. ) ;
#27958 = EDGE_CURVE ( 'NONE', #1241, #13855, #10709, .T. ) ;
#27959 = ORIENTED_EDGE ( 'NONE', *, *, #4952, .F. ) ;
#27960 = AXIS2_PLACEMENT_3D ( 'NONE', #31576, #11960, #15347 ) ;
#27961 = CARTESIAN_POINT ( 'NONE',  ( 0.000000000000000000, 0.000000000000000000, -40.40000000000000568 ) ) ;
#27962 = CARTESIAN_POINT ( 'NONE',  ( -35.50000000000000000, -113.9929510916434339, 12.44250253426871033 ) ) ;
#27963 = DIRECTION ( 'NONE',  ( 1.000000000000000000, 0.000000000000000000, 0.000000000000000000 ) ) ;
#27964 = LINE ( 'NONE', #33537, #20527 ) ;
#27965 = EDGE_CURVE ( 'NONE', #16096, #31067, #4584, .T. ) ;
#27966 = CARTESIAN_POINT ( 'NONE',  ( -34.50000000000000000, -115.9630435732166518, -0.9469505670456015434 ) ) ;
#27967 = ADVANCED_FACE ( 'NONE', ( #34638 ), #2960, .F. ) ;
#27968 = CARTESIAN_POINT ( 'NONE',  ( -35.50000000000000000, -114.3496480102005251, 8.538090462223289379 ) ) ;
#27969 = VECTOR ( 'NONE', #29703, 1000.000000000000000 ) ;
#27970 = DIRECTION ( 'NONE',  ( 0.000000000000000000, 0.000000000000000000, -1.000000000000000000 ) ) ;
#27971 = DIRECTION ( 'NONE',  ( 0.000000000000000000, 0.000000000000000000, -1.000000000000000000 ) ) ;
#27972 = AXIS2_PLACEMENT_3D ( 'NONE', #31529, #6319, #27934 ) ;
#27973 = VERTEX_POINT ( 'NONE', #24838 ) ;
#27974 = CARTESIAN_POINT ( 'NONE',  ( 7.999999999999992895, 32.00046193115148441, 34.40241257139697950 ) ) ;
#27975 = LINE ( 'NONE', #3326, #31173 ) ;
#27976 = DIRECTION ( 'NONE',  ( -1.000000000000000000, 0.000000000000000000, 0.000000000000000000 ) ) ;
#27977 = VECTOR ( 'NONE', #24703, 1000.000000000000000 ) ;
#27978 = CIRCLE ( 'NONE', #12452, 8.000000000000007105 ) ;
#27979 = ORIENTED_EDGE ( 'NONE', *, *, #20898, .F. ) ;
#27980 = CIRCLE ( 'NONE', #13613, 8.000000000000001776 ) ;
#27981 = CYLINDRICAL_SURFACE ( 'NONE', #18582, 4.800000000000000711 ) ;
#27982 = CARTESIAN_POINT ( 'NONE',  ( 4.000000000000003553, -10.15474465512033930, -9.637487275701225542 ) ) ;
#27983 = CARTESIAN_POINT ( 'NONE',  ( -34.49999999999998579, -11.24969279549607748, 111.5585998451919778 ) ) ;
#27984 = CARTESIAN_POINT ( 'NONE',  ( 0.000000000000000000, 17.50309955389611716, 43.60271849949368317 ) ) ;
#27985 = AXIS2_PLACEMENT_3D ( 'NONE', #20954, #1721, #31777 ) ;
#27986 = CONTEXT_DEPENDENT_SHAPE_REPRESENTATION ( #3247, #12101 ) ;
#27987 = DIRECTION ( 'NONE',  ( 0.000000000000000000, 0.9659258262890707547, -0.2588190451025116912 ) ) ;
#27988 = DIRECTION ( 'NONE',  ( -1.734723475976807094E-16, 1.000000000000000000, -0.000000000000000000 ) ) ;
#27989 = EDGE_CURVE ( 'NONE', #7837, #24291, #32941, .T. ) ;
#27990 = VECTOR ( 'NONE', #20957, 1000.000000000000000 ) ;
#27991 = ORIENTED_EDGE ( 'NONE', *, *, #29153, .T. ) ;
#27992 = CARTESIAN_POINT ( 'NONE',  ( 0.000000000000000000, 0.000000000000000000, -52.50000000000000000 ) ) ;
#27993 = CARTESIAN_POINT ( 'NONE',  ( 65.00000000000001421, -26.38406014851796400, 79.52301627764160230 ) ) ;
#27994 = ORIENTED_EDGE ( 'NONE', *, *, #13734, .F. ) ;
#27995 = CARTESIAN_POINT ( 'NONE',  ( -37.66520193420439711, -114.7490116281687023, 4.558975545821549957 ) ) ;
#27996 = VERTEX_POINT ( 'NONE', #164 ) ;
#27997 = EDGE_CURVE ( 'NONE', #16080, #12983, #19068, .T. ) ;
#27998 = SHAPE_REPRESENTATION_RELATIONSHIP ( 'NONE' , 'NONE' ,  #33958, #3950 ) ;
#27999 = CIRCLE ( 'NONE', #5004, 4.000000000000000000 ) ;
#28000 = EDGE_LOOP ( 'NONE', ( #25199, #13300 ) ) ;
#28001 = EDGE_LOOP ( 'NONE', ( #25800, #12763, #10587, #12039 ) ) ;
#28002 = DIRECTION ( 'NONE',  ( 1.000000000000000000, -0.000000000000000000, -0.000000000000000000 ) ) ;
#28003 = AXIS2_PLACEMENT_3D ( 'NONE', #33019, #4778, #35372 ) ;
#28004 = EDGE_CURVE ( 'NONE', #21050, #9746, #24519, .T. ) ;
#28005 = EDGE_CURVE ( 'NONE', #17434, #23255, #33124, .T. ) ;
#28006 = CARTESIAN_POINT ( 'NONE',  ( -35.50000000000000711, -115.0468226098135744, -1.624774171496087716 ) ) ;
#28007 = VECTOR ( 'NONE', #6402, 1000.000000000000000 ) ;
#28008 = DIRECTION ( 'NONE',  ( -1.000000000000000000, 0.000000000000000000, 0.000000000000000000 ) ) ;
#28009 = AXIS2_PLACEMENT_3D ( 'NONE', #16596, #11200, #33172 ) ;
#28010 = CARTESIAN_POINT ( 'NONE',  ( -35.50000000000000711, -114.9922651054798308, 10.46846006712531008 ) ) ;
#28011 = DIRECTION ( 'NONE',  ( 1.000000000000000000, -4.336808689941996437E-15, -1.084202172485499109E-15 ) ) ;
#28012 = VECTOR ( 'NONE', #10531, 1000.000000000000000 ) ;
#28013 = PRESENTATION_LAYER_ASSIGNMENT (  '', '', ( #29742 ) ) ;
#28014 = DIRECTION ( 'NONE',  ( 0.000000000000000000, 0.000000000000000000, 1.000000000000000000 ) ) ;
#28015 = ADVANCED_FACE ( 'NONE', ( #16884 ), #19871, .T. ) ;
#28016 = CARTESIAN_POINT ( 'NONE',  ( -34.50000000000000000, -114.9929510916434339, 10.72628538622835670 ) ) ;
#28017 = DIRECTION ( 'NONE',  ( 0.000000000000000000, 0.7705132427757903635, -0.6374239897486881912 ) ) ;
#28018 = PLANE ( 'NONE',  #15126 ) ;
#28019 = CARTESIAN_POINT ( 'NONE',  ( -35.50000000000000000, -115.9929510916434481, 10.59426868253284226 ) ) ;
#28020 = CARTESIAN_POINT ( 'NONE',  ( -35.50000000000000711, -112.0460568841087223, -0.8839717462762063382 ) ) ;
#28021 = DIRECTION ( 'NONE',  ( 1.000000000000000000, -5.339440136655842133E-16, -1.047965281155519420E-16 ) ) ;
#28022 = CARTESIAN_POINT ( 'NONE',  ( 0.000000000000000000, 0.000000000000000000, 0.000000000000000000 ) ) ;
#28023 = VECTOR ( 'NONE', #5357, 1000.000000000000000 ) ;
#28024 = DIRECTION ( 'NONE',  ( -1.000000000000000000, -0.000000000000000000, 0.000000000000000000 ) ) ;
#28025 = DIRECTION ( 'NONE',  ( 1.000000000000000000, 0.000000000000000000, 0.000000000000000000 ) ) ;
#28026 = AXIS2_PLACEMENT_3D ( 'NONE', #24090, #35075, #9676 ) ;
#28027 = DIRECTION ( 'NONE',  ( -1.174092375852890260E-15, 4.222049128630259891E-16, 1.000000000000000000 ) ) ;
#28028 = DIRECTION ( 'NONE',  ( -1.000000000000000000, 0.000000000000000000, 0.000000000000000000 ) ) ;
#28029 = EDGE_LOOP ( 'NONE', ( #16191, #30210, #31542, #16718 ) ) ;
#28030 = CARTESIAN_POINT ( 'NONE',  ( -35.02454729103298803, -113.1123104723225197, 8.402725545821549957 ) ) ;
#28031 = VECTOR ( 'NONE', #32173, 1000.000000000000000 ) ;
#28032 = CARTESIAN_POINT ( 'NONE',  ( 7.999999999999992895, -24.47917365149915270, -45.87777302070961127 ) ) ;
#28033 = DIRECTION ( 'NONE',  ( -1.000000000000000000, 0.000000000000000000, 0.000000000000000000 ) ) ;
#28034 = CARTESIAN_POINT ( 'NONE',  ( 70.00000000000001421, -32.20716221109618260, 78.48218274074299927 ) ) ;
#28035 = EDGE_CURVE ( 'NONE', #20175, #26484, #22299, .T. ) ;
#28036 = ORIENTED_EDGE ( 'NONE', *, *, #11009, .T. ) ;
#28037 = ORIENTED_EDGE ( 'NONE', *, *, #2492, .F. ) ;
#28038 = CIRCLE ( 'NONE', #15361, 3.799999999999999822 ) ;
#28039 = UNCERTAINTY_MEASURE_WITH_UNIT (LENGTH_MEASURE( 1.000000000000000082E-05 ), #17842, 'distance_accuracy_value', 'NONE');
#28040 = EDGE_CURVE ( 'NONE', #16940, #15222, #14198, .T. ) ;
#28041 = LINE ( 'NONE', #16678, #12568 ) ;
#28042 = ADVANCED_FACE ( 'NONE', ( #27551 ), #5754, .T. ) ;
#28043 = DIRECTION ( 'NONE',  ( 1.000000000000000000, -0.000000000000000000, 0.000000000000000000 ) ) ;
#28044 = ORIENTED_EDGE ( 'NONE', *, *, #17857, .T. ) ;
#28045 = ORIENTED_EDGE ( 'NONE', *, *, #29391, .T. ) ;
#28046 = AXIS2_PLACEMENT_3D ( 'NONE', #35226, #21502, #92 ) ;
#28047 = DIRECTION ( 'NONE',  ( 0.000000000000000000, -0.3420201433256564449, -0.9396926207859127578 ) ) ;
#28048 = FACE_OUTER_BOUND ( 'NONE', #17202, .T. ) ;
#28049 = EDGE_CURVE ( 'NONE', #10255, #25177, #16545, .T. ) ;
#28050 = ADVANCED_FACE ( 'NONE', ( #8443 ), #13683, .T. ) ;
#28051 = CARTESIAN_POINT ( 'NONE',  ( -33.50000000000000000, -1.396317957091941414E-14, 110.0000000000000142 ) ) ;
#28052 = DIRECTION ( 'NONE',  ( 0.000000000000000000, -0.3090169943749350723, -0.9510565162951576390 ) ) ;
#28053 = AXIS2_PLACEMENT_3D ( 'NONE', #27974, #25633, #14623 ) ;
#28054 = ORIENTED_EDGE ( 'NONE', *, *, #35575, .T. ) ;
#28055 = ORIENTED_EDGE ( 'NONE', *, *, #11688, .T. ) ;
#28056 = AXIS2_PLACEMENT_3D ( 'NONE', #17812, #28812, #4162 ) ;
#28057 = CARTESIAN_POINT ( 'NONE',  ( 0.000000000000000000, -2.710505431213761085E-17, -55.00000000000000000 ) ) ;
#28058 = CIRCLE ( 'NONE', #12530, 17.49900000000000233 ) ;
#28059 = DIRECTION ( 'NONE',  ( 0.000000000000000000, -1.000000000000000000, 0.000000000000000000 ) ) ;
#28060 = ORIENTED_EDGE ( 'NONE', *, *, #3495, .T. ) ;
#28061 = CARTESIAN_POINT ( 'NONE',  ( 4.000000000000000000, 4.627536653468036720E-16, -20.99999999999999645 ) ) ;
#28062 = VECTOR ( 'NONE', #30956, 1000.000000000000000 ) ;
#28063 = CARTESIAN_POINT ( 'NONE',  ( -34.50000000000000000, -113.0140978167138712, -0.6247823525985405357 ) ) ;
#28064 = DIRECTION ( 'NONE',  ( -1.000000000000000000, 0.000000000000000000, 0.000000000000000000 ) ) ;
#28065 = DIRECTION ( 'NONE',  ( -1.000000000000000000, 0.000000000000000000, 0.000000000000000000 ) ) ;
#28066 = CARTESIAN_POINT ( 'NONE',  ( -34.50000000000000000, -115.9929510916434481, 10.52000928670414126 ) ) ;
#28067 = DIRECTION ( 'NONE',  ( 0.000000000000000000, 0.000000000000000000, 1.000000000000000000 ) ) ;
#28068 = DIRECTION ( 'NONE',  ( 0.000000000000000000, -0.5000000000000001110, 0.8660254037844385966 ) ) ;
#28069 = CARTESIAN_POINT ( 'NONE',  ( -34.50000000000000000, -114.2265172349312508, 8.519938377296172760 ) ) ;
#28070 = CARTESIAN_POINT ( 'NONE',  ( 29.99999999999999289, 14.30000000000001315, 3.000000000000002665 ) ) ;
#28071 = VECTOR ( 'NONE', #20297, 1000.000000000000000 ) ;
#28072 = DIRECTION ( 'NONE',  ( -1.000000000000000000, 0.000000000000000000, 0.000000000000000000 ) ) ;
#28073 = DIRECTION ( 'NONE',  ( -1.000000000000000000, 0.000000000000000000, 0.000000000000000000 ) ) ;
#28074 = DIRECTION ( 'NONE',  ( -1.000000000000000000, -0.000000000000000000, -0.000000000000000000 ) ) ;
#28075 = VERTEX_POINT ( 'NONE', #11669 ) ;
#28076 = DIRECTION ( 'NONE',  ( 0.1305261922200566527, -0.9914448613738098270, -5.718426984394921662E-16 ) ) ;
#28077 = EDGE_LOOP ( 'NONE', ( #15004, #12037, #16197, #24837 ) ) ;
#28078 = CARTESIAN_POINT ( 'NONE',  ( -34.92058450342251064, -116.1632251905417945, 3.191024454178448710 ) ) ;
#28079 = DIRECTION ( 'NONE',  ( 0.000000000000000000, 0.4817536741017163782, -0.8763066800438630288 ) ) ;
#28080 = CARTESIAN_POINT ( 'NONE',  ( -35.50000000000000711, -112.0269151300720409, -0.7876962586524208776 ) ) ;
#28081 = ORIENTED_EDGE ( 'NONE', *, *, #5211, .T. ) ;
#28082 = ORIENTED_EDGE ( 'NONE', *, *, #14738, .T. ) ;
#28083 = ADVANCED_FACE ( 'NONE', ( #32760 ), #2719, .T. ) ;
#28084 = DIRECTION ( 'NONE',  ( -1.000000000000000000, 0.000000000000000000, 0.000000000000000000 ) ) ;
#28085 = LINE ( 'NONE', #3597, #14587 ) ;
#28086 = VERTEX_POINT ( 'NONE', #11153 ) ;
#28087 = CIRCLE ( 'NONE', #15411, 52.00000000000000711 ) ;
#28088 = VECTOR ( 'NONE', #33705, 1000.000000000000000 ) ;
#28089 = FACE_OUTER_BOUND ( 'NONE', #6395, .T. ) ;
#28090 = ORIENTED_EDGE ( 'NONE', *, *, #26001, .T. ) ;
#28091 = VERTEX_POINT ( 'NONE', #14019 ) ;
#28092 = CYLINDRICAL_SURFACE ( 'NONE', #19387, 20.00000000000000355 ) ;
#28093 = SURFACE_STYLE_FILL_AREA ( #8465 ) ;
#28094 = CARTESIAN_POINT ( 'NONE',  ( -29.99999999999999645, -26.99999999999999645, 113.9999999999999858 ) ) ;
#28095 = ORIENTED_EDGE ( 'NONE', *, *, #6406, .F. ) ;
#28096 = ORIENTED_EDGE ( 'NONE', *, *, #6825, .T. ) ;
#28097 = CARTESIAN_POINT ( 'NONE',  ( -34.50000000000000000, -116.9980674558286040, -0.8858242144478970514 ) ) ;
#28098 = DIRECTION ( 'NONE',  ( -1.000000000000000000, 0.000000000000000000, 0.000000000000000000 ) ) ;
#28099 = EDGE_LOOP ( 'NONE', ( #21108, #29993, #27241, #19729 ) ) ;
#28100 = CARTESIAN_POINT ( 'NONE',  ( -35.52552712174884419, -114.9929510916434339, 12.77960891308624447 ) ) ;
#28101 = CARTESIAN_POINT ( 'NONE',  ( -38.92341863475394348, -113.9929510916434339, 13.10177712753322155 ) ) ;
#28102 = CARTESIAN_POINT ( 'NONE',  ( -3.799999999999999822, 4.653657836759942730E-16, -40.89999999999999858 ) ) ;
#28103 = AXIS2_PLACEMENT_3D ( 'NONE', #25300, #11437, #19521 ) ;
#28104 = CARTESIAN_POINT ( 'NONE',  ( 4.000000000000003553, -18.53613841426824038, 48.58406706613897796 ) ) ;
#28105 = CARTESIAN_POINT ( 'NONE',  ( -34.50000000000000000, -113.9929510916434339, 10.61627146648203990 ) ) ;
#28106 = FACE_OUTER_BOUND ( 'NONE', #27695, .T. ) ;
#28107 = AXIS2_PLACEMENT_3D ( 'NONE', #8906, #1000, #20400 ) ;
#28108 = CARTESIAN_POINT ( 'NONE',  ( -37.24999999999992895, -114.9929510916434339, 13.11852480586264669 ) ) ;
#28109 = CARTESIAN_POINT ( 'NONE',  ( -34.49999999999998579, -17.72201855431888973, 73.69543654875883476 ) ) ;
#28110 = AXIS2_PLACEMENT_3D ( 'NONE', #35195, #27087, #27625 ) ;
#28111 = LINE ( 'NONE', #17815, #9504 ) ;
#28112 = VERTEX_POINT ( 'NONE', #19584 ) ;
#28113 = EDGE_LOOP ( 'NONE', ( #4096, #12005, #17113, #19052 ) ) ;
#28114 = LINE ( 'NONE', #5967, #25286 ) ;
#28115 = CARTESIAN_POINT ( 'NONE',  ( 0.000000000000000000, 7.317194182740413666, -18.61340026142641690 ) ) ;
#28116 = ORIENTED_EDGE ( 'NONE', *, *, #7540, .T. ) ;
#28117 = CARTESIAN_POINT ( 'NONE',  ( -42.49999999999999289, -39.90017302060827831, 86.49999999999991473 ) ) ;
#28118 = VERTEX_POINT ( 'NONE', #5409 ) ;
#28119 = ADVANCED_FACE ( 'NONE', ( #16712 ), #11500, .T. ) ;
#28120 = CARTESIAN_POINT ( 'NONE',  ( -35.50000000000000000, -113.0140978167138712, -0.6247823525985405357 ) ) ;
#28121 = DIRECTION ( 'NONE',  ( 0.000000000000000000, 0.000000000000000000, 1.000000000000000000 ) ) ;
#28122 = CARTESIAN_POINT ( 'NONE',  ( -35.02454729103298803, -114.8876895276775087, 4.597274454178448266 ) ) ;
#28123 = ORIENTED_EDGE ( 'NONE', *, *, #26909, .T. ) ;
#28124 = CARTESIAN_POINT ( 'NONE',  ( 70.00000000000001421, 58.94749845961094792, 75.40996905927893579 ) ) ;
#28125 = ORIENTED_EDGE ( 'NONE', *, *, #30015, .T. ) ;
#28126 = DIRECTION ( 'NONE',  ( 1.000000000000000000, -5.339440136655842133E-16, -1.047965281155519420E-16 ) ) ;
#28127 = CARTESIAN_POINT ( 'NONE',  ( -35.50000000000000000, -114.9515981487115823, -2.624803185604625000 ) ) ;
#28128 = ORIENTED_EDGE ( 'NONE', *, *, #29574, .F. ) ;
#28129 = VERTEX_POINT ( 'NONE', #30588 ) ;
#28130 = CARTESIAN_POINT ( 'NONE',  ( -39.02454729103295961, -114.7691647218148745, 6.659774454178450043 ) ) ;
#28131 = CIRCLE ( 'NONE', #20052, 4.000000000000000000 ) ;
#28132 = EDGE_CURVE ( 'NONE', #22200, #29687, #17005, .T. ) ;
#28133 = SURFACE_STYLE_FILL_AREA ( #5645 ) ;
#28134 = DIRECTION ( 'NONE',  ( -1.000000000000000000, -1.836970198721030181E-16, 0.000000000000000000 ) ) ;
#28135 = ORIENTED_EDGE ( 'NONE', *, *, #32604, .T. ) ;
#28136 = EDGE_LOOP ( 'NONE', ( #12350, #16216 ) ) ;
#28137 = CIRCLE ( 'NONE', #22359, 20.00000000000000711 ) ;
#28138 = CARTESIAN_POINT ( 'NONE',  ( -34.50000000000000000, -113.2637153405686519, 1.912112492696748989 ) ) ;
#28139 = CARTESIAN_POINT ( 'NONE',  ( -55.00000000000000000, 0.000000000000000000, 0.000000000000000000 ) ) ;
#28140 = COLOUR_RGB ( '', 0.09019608, 0.27058824, 0.51372549) ;
#28141 = ORIENTED_EDGE ( 'NONE', *, *, #21355, .T. ) ;
#28142 = PRODUCT_DEFINITION_CONTEXT ( 'detailed design', #24379, 'design' ) ;
#28143 = ORIENTED_EDGE ( 'NONE', *, *, #25173, .T. ) ;
#28144 = CARTESIAN_POINT ( 'NONE',  ( 7.999999999999992895, 0.2227391519123156360, -46.98410307550729215 ) ) ;
#28145 = CARTESIAN_POINT ( 'NONE',  ( -35.99386409314529800, -113.9929510916434339, 13.11852378322482515 ) ) ;
#28146 = CYLINDRICAL_SURFACE ( 'NONE', #32243, 8.000000000000000000 ) ;
#28147 = DIRECTION ( 'NONE',  ( -1.000000000000000000, -0.000000000000000000, 0.000000000000000000 ) ) ;
#28148 = CARTESIAN_POINT ( 'NONE',  ( -34.50000000000000000, -111.0140978167138570, 0.6252176474015680441 ) ) ;
#28149 = CARTESIAN_POINT ( 'NONE',  ( -39.00000000000000000, -115.9929510916434481, 12.39849696637031151 ) ) ;
#28150 = CARTESIAN_POINT ( 'NONE',  ( 8.000000000000000000, -12.96676809804157848, 13.60411018104313641 ) ) ;
#28151 = FACE_OUTER_BOUND ( 'NONE', #8964, .T. ) ;
#28152 = DIRECTION ( 'NONE',  ( -1.000000000000000000, 0.000000000000000000, 0.000000000000000000 ) ) ;
#28153 = DIRECTION ( 'NONE',  ( -1.174092375852890260E-15, 4.222049128630259891E-16, 1.000000000000000000 ) ) ;
#28154 = LINE ( 'NONE', #9241, #716 ) ;
#28155 = EDGE_LOOP ( 'NONE', ( #4267, #3693, #13997, #30784, #17305, #26665 ) ) ;
#28156 = CIRCLE ( 'NONE', #9755, 5.000000000000011546 ) ;
#28157 = CARTESIAN_POINT ( 'NONE',  ( 0.000000000000000000, -3.268936481846063113, -13.61301047812921183 ) ) ;
#28158 = LINE ( 'NONE', #31568, #26803 ) ;
#28159 = EDGE_CURVE ( 'NONE', #6112, #21169, #21611, .T. ) ;
#28160 = DIRECTION ( 'NONE',  ( 0.000000000000000000, -0.4817536741017036661, -0.8763066800438699122 ) ) ;
#28161 = LINE ( 'NONE', #11762, #18412 ) ;
#28162 = EDGE_CURVE ( 'NONE', #27460, #7117, #10114, .T. ) ;
#28163 = ITEM_DEFINED_TRANSFORMATION ( 'NONE', 'NONE', #27022,  #21307 ) ;
#28164 = AXIS2_PLACEMENT_3D ( 'NONE', #20243, #34318, #12166 ) ;
#28165 = EDGE_CURVE ( 'NONE', #4367, #17248, #13825, .T. ) ;
#28166 = LINE ( 'NONE', #31036, #9546 ) ;
#28167 = DIRECTION ( 'NONE',  ( 0.000000000000000000, 0.000000000000000000, 1.000000000000000000 ) ) ;
#28168 = VERTEX_POINT ( 'NONE', #1062 ) ;
#28169 = CARTESIAN_POINT ( 'NONE',  ( -46.00000000000000000, -25.98076211353320275, 84.99999999999992895 ) ) ;
#28170 = LINE ( 'NONE', #8891, #33798 ) ;
#28171 = DIRECTION ( 'NONE',  ( 0.000000000000000000, 0.000000000000000000, 1.000000000000000000 ) ) ;
#28172 = ORIENTED_EDGE ( 'NONE', *, *, #6380, .F. ) ;
#28173 = CARTESIAN_POINT ( 'NONE',  ( -36.94073759706868287, -115.0000000000000000, 4.371475545821550845 ) ) ;
#28174 = EDGE_CURVE ( 'NONE', #32022, #8923, #30248, .T. ) ;
#28175 = EDGE_LOOP ( 'NONE', ( #29148, #24340, #6204, #5731 ) ) ;
#28176 = EDGE_CURVE ( 'NONE', #18999, #8679, #14691, .T. ) ;
#28177 = CONTEXT_DEPENDENT_SHAPE_REPRESENTATION ( #25325, #32847 ) ;
#28178 = EDGE_LOOP ( 'NONE', ( #33273, #2871 ) ) ;
#28179 = ORIENTED_EDGE ( 'NONE', *, *, #15535, .F. ) ;
#28180 = CARTESIAN_POINT ( 'NONE',  ( -34.50000000000001421, -8.980762113533204527, 86.49999999999994316 ) ) ;
#28181 = CIRCLE ( 'NONE', #2323, 8.000000000000008882 ) ;
#28182 = CARTESIAN_POINT ( 'NONE',  ( -35.50000000000000711, -115.8137639216009234, -1.239329810084483841 ) ) ;
#28183 = FACE_OUTER_BOUND ( 'NONE', #24607, .T. ) ;
#28184 = AXIS2_PLACEMENT_3D ( 'NONE', #26598, #1936, #23896 ) ;
#28185 = DIRECTION ( 'NONE',  ( -1.000000000000000000, 0.000000000000000000, 0.000000000000000000 ) ) ;
#28186 = FACE_OUTER_BOUND ( 'NONE', #29900, .T. ) ;
#28187 = AXIS2_PLACEMENT_3D ( 'NONE', #32684, #33036, #3152 ) ;
#28188 = AXIS2_PLACEMENT_3D ( 'NONE', #35490, #19252, #22136 ) ;
#28189 = CARTESIAN_POINT ( 'NONE',  ( 0.000000000000000000, 0.000000000000000000, 0.000000000000000000 ) ) ;
#28190 = ADVANCED_FACE ( 'NONE', ( #23004 ), #14896, .F. ) ;
#28191 = CARTESIAN_POINT ( 'NONE',  ( -34.50000000000000000, -114.0185793162512908, 9.502217742515812304 ) ) ;
#28192 = CARTESIAN_POINT ( 'NONE',  ( -34.49999999999998579, -27.48076211353328802, 98.91941090707497608 ) ) ;
#28193 = PRODUCT_DEFINITION_SHAPE ( 'NONE', 'NONE',  #24258 ) ;
#28194 = CARTESIAN_POINT ( 'NONE',  ( -39.49999999999999289, -1.387778780781445676E-14, 106.0000000000000000 ) ) ;
#28195 = CARTESIAN_POINT ( 'NONE',  ( -35.50000000000000000, -114.2183886307118428, 8.518969274377507617 ) ) ;
#28196 = DIRECTION ( 'NONE',  ( 0.000000000000000000, 0.8660254037844362651, 0.5000000000000041078 ) ) ;
#28197 = DIRECTION ( 'NONE',  ( -1.000000000000000000, 0.000000000000000000, 0.000000000000000000 ) ) ;
#28198 = CARTESIAN_POINT ( 'NONE',  ( -35.00000000000000000, -116.0140978167138712, 0.8752176474015622709 ) ) ;
#28199 = FACE_OUTER_BOUND ( 'NONE', #10260, .T. ) ;
#28200 = DIRECTION ( 'NONE',  ( 0.000000000000000000, 0.000000000000000000, -1.000000000000000000 ) ) ;
#28201 = EDGE_CURVE ( 'NONE', #22597, #17024, #23928, .T. ) ;
#28202 = CARTESIAN_POINT ( 'NONE',  ( -42.49999999999999289, -39.90017302060827831, 83.49999999999991473 ) ) ;
#28203 = CARTESIAN_POINT ( 'NONE',  ( 0.000000000000000000, -17.08890430202718491, -43.76671000081963570 ) ) ;
#28204 = ORIENTED_EDGE ( 'NONE', *, *, #6011, .F. ) ;
#28205 = EDGE_CURVE ( 'NONE', #33795, #6545, #28515, .T. ) ;
#28206 = EDGE_CURVE ( 'NONE', #32324, #22667, #34302, .T. ) ;
#28207 = CARTESIAN_POINT ( 'NONE',  ( -35.99999999999999289, -113.9407375970686758, 9.996475545821549957 ) ) ;
#28208 = CARTESIAN_POINT ( 'NONE',  ( 5.400000000000085620, -1.000000000000049516, 45.00000000000000711 ) ) ;
#28209 = DIRECTION ( 'NONE',  ( 0.000000000000000000, -0.8660254037844433705, 0.4999999999999918954 ) ) ;
#28210 = ORIENTED_EDGE ( 'NONE', *, *, #26633, .T. ) ;
#28211 = VECTOR ( 'NONE', #31638, 1000.000000000000000 ) ;
#28212 = VERTEX_POINT ( 'NONE', #34182 ) ;
#28213 = DIRECTION ( 'NONE',  ( -1.000000000000000000, -1.734723475976807094E-16, 0.000000000000000000 ) ) ;
#28214 = VERTEX_POINT ( 'NONE', #12032 ) ;
#28215 = CARTESIAN_POINT ( 'NONE',  ( -34.83677480945819838, -111.9205845034225462, 8.816024454178446490 ) ) ;
#28216 = ORIENTED_EDGE ( 'NONE', *, *, #9935, .F. ) ;
#28217 = CIRCLE ( 'NONE', #10950, 3.799999999999999822 ) ;
#28218 = AXIS2_PLACEMENT_3D ( 'NONE', #5604, #27907, #27574 ) ;
#28219 = EDGE_CURVE ( 'NONE', #12368, #28677, #20287, .T. ) ;
#28220 = LINE ( 'NONE', #3558, #22720 ) ;
#28221 = DIRECTION ( 'NONE',  ( 1.000000000000000000, 0.000000000000000000, 0.000000000000000000 ) ) ;
#28222 = APPLICATION_PROTOCOL_DEFINITION ( 'draft international standard', 'automotive_design', 1998, #3001 ) ;
#28223 = CARTESIAN_POINT ( 'NONE',  ( 8.000000000000000000, 0.000000000000000000, 0.000000000000000000 ) ) ;
#28224 = VERTEX_POINT ( 'NONE', #9507 ) ;
#28225 = VERTEX_POINT ( 'NONE', #31122 ) ;
#28226 = DIRECTION ( 'NONE',  ( 0.000000000000000000, 0.000000000000000000, -1.000000000000000000 ) ) ;
#28227 = AXIS2_PLACEMENT_3D ( 'NONE', #26427, #23715, #15413 ) ;
#28228 = EDGE_LOOP ( 'NONE', ( #9332, #21778, #4895, #8786 ) ) ;
#28229 = CARTESIAN_POINT ( 'NONE',  ( -34.49999999999998579, -14.67619866229204284, 93.25874355921412473 ) ) ;
#28230 = EDGE_CURVE ( 'NONE', #35346, #21017, #7843, .T. ) ;
#28231 = CARTESIAN_POINT ( 'NONE',  ( -34.50000000000000000, -115.0140978167138712, -0.6247823525984407267 ) ) ;
#28232 = DIRECTION ( 'NONE',  ( 1.000000000000000000, -1.110223024625156540E-16, 0.000000000000000000 ) ) ;
#28233 = CYLINDRICAL_SURFACE ( 'NONE', #27655, 13.99999999999999822 ) ;
#28234 = CARTESIAN_POINT ( 'NONE',  ( -34.50000000000000000, -114.2675000158779710, 8.525177020294046670 ) ) ;
#28235 = ADVANCED_FACE ( 'NONE', ( #14535, #4129 ), #6804, .F. ) ;
#28236 = FACE_OUTER_BOUND ( 'NONE', #3632, .T. ) ;
#28237 = DIRECTION ( 'NONE',  ( -1.000000000000000000, 0.000000000000000000, 0.000000000000000000 ) ) ;
#28238 =( GEOMETRIC_REPRESENTATION_CONTEXT ( 3 ) GLOBAL_UNCERTAINTY_ASSIGNED_CONTEXT ( ( #16433 ) ) GLOBAL_UNIT_ASSIGNED_CONTEXT ( ( #31754, #1888, #9617 ) ) REPRESENTATION_CONTEXT ( 'NONE', 'WORKASPACE' ) );
#28239 = CARTESIAN_POINT ( 'NONE',  ( -34.50000000000000000, -114.3496480102005251, 8.538090462223289379 ) ) ;
#28241 = CARTESIAN_POINT ( 'NONE',  ( 3.983177536951269193, -13.66651769228263724, -1.200000000000006617 ) ) ;
#28240 = VECTOR ( 'NONE', #27172, 1000.000000000000000 ) ;
#28242 = CARTESIAN_POINT ( 'NONE',  ( 7.999999999999992895, -17.50309955389579386, -43.60271849949381817 ) ) ;
#28243 = CYLINDRICAL_SURFACE ( 'NONE', #25658, 20.00000000000000355 ) ;
#28244 = DIRECTION ( 'NONE',  ( 1.000000000000000000, 1.734723475976807094E-16, 0.000000000000000000 ) ) ;
#28245 = ORIENTED_EDGE ( 'NONE', *, *, #3733, .T. ) ;
#28246 = DIRECTION ( 'NONE',  ( -1.000000000000000000, 0.000000000000000000, 0.000000000000000000 ) ) ;
#28247 = VERTEX_POINT ( 'NONE', #23365 ) ;
#28248 = EDGE_CURVE ( 'NONE', #14077, #16923, #26260, .T. ) ;
#28249 = CARTESIAN_POINT ( 'NONE',  ( -34.83677480945819838, -111.9205845034225462, 5.816024454178450043 ) ) ;
#28250 = ADVANCED_FACE ( 'NONE', ( #31644 ), #863, .T. ) ;
#28251 = DIRECTION ( 'NONE',  ( 0.000000000000000000, -0.9048270524660145808, -0.4257792915650830956 ) ) ;
#28252 = CARTESIAN_POINT ( 'NONE',  ( -35.50000000000000711, -113.8474311500459777, -1.624782352598427959 ) ) ;
#28253 = ORIENTED_EDGE ( 'NONE', *, *, #33056, .T. ) ;
#28254 = VERTEX_POINT ( 'NONE', #4301 ) ;
#28255 = FACE_OUTER_BOUND ( 'NONE', #16044, .T. ) ;
#28256 = DIRECTION ( 'NONE',  ( 0.000000000000000000, -0.3090169943749546677, 0.9510565162951511997 ) ) ;
#28257 = EDGE_LOOP ( 'NONE', ( #2147, #25734, #3072, #15827 ) ) ;
#28258 = ORIENTED_EDGE ( 'NONE', *, *, #11092, .F. ) ;
#28259 = DIRECTION ( 'NONE',  ( -1.000000000000000000, 0.000000000000000000, 0.000000000000000000 ) ) ;
#28260 = ORIENTED_EDGE ( 'NONE', *, *, #26815, .T. ) ;
#28261 = ORIENTED_EDGE ( 'NONE', *, *, #8034, .T. ) ;
#28262 = CARTESIAN_POINT ( 'NONE',  ( -36.23083527818513261, -111.9754527089670404, 6.715225545821550845 ) ) ;
#28263 = AXIS2_PLACEMENT_3D ( 'NONE', #8769, #23175, #1049 ) ;
#28264 = STYLED_ITEM ( 'NONE', ( #30308 ), #19774 ) ;
#28265 = AXIS2_PLACEMENT_3D ( 'NONE', #30919, #19906, #24642 ) ;
#28266 = SURFACE_SIDE_STYLE ('',( #34560 ) ) ;
#28267 = DIRECTION ( 'NONE',  ( 0.000000000000000000, 0.000000000000000000, 1.000000000000000000 ) ) ;
#28268 = ORIENTED_EDGE ( 'NONE', *, *, #27389, .F. ) ;
#28269 = ORIENTED_EDGE ( 'NONE', *, *, #28159, .F. ) ;
#28270 = CARTESIAN_POINT ( 'NONE',  ( -35.50000000000000000, -116.0215255531121983, -2.372276521655488857 ) ) ;
#28271 = CARTESIAN_POINT ( 'NONE',  ( 8.000000000000000000, -18.48663108841356717, -3.384281271888017084 ) ) ;
#28272 = ORIENTED_EDGE ( 'NONE', *, *, #7710, .F. ) ;
#28273 = CARTESIAN_POINT ( 'NONE',  ( -35.50640865667918433, -114.9929510916434339, 12.69998175888958514 ) ) ;
#28274 = EDGE_CURVE ( 'NONE', #32201, #6784, #10736, .T. ) ;
#28275 = EDGE_CURVE ( 'NONE', #29296, #11194, #34881, .T. ) ;
#28276 = CARTESIAN_POINT ( 'NONE',  ( -37.62254989966453422, -113.9929510916434339, 14.11371147303758278 ) ) ;
#28277 = DIRECTION ( 'NONE',  ( 0.000000000000000000, 0.000000000000000000, -1.000000000000000000 ) ) ;
#28278 = DIRECTION ( 'NONE',  ( 0.000000000000000000, -1.000000000000000000, 0.000000000000000000 ) ) ;
#28279 = CARTESIAN_POINT ( 'NONE',  ( -37.18750000000004974, -113.9929510916434339, 14.11852480586265024 ) ) ;
#28280 = DIRECTION ( 'NONE',  ( 0.000000000000000000, 0.000000000000000000, 1.000000000000000000 ) ) ;
#28281 = CARTESIAN_POINT ( 'NONE',  ( -35.50160444427493189, -114.9929510916434339, 12.65937477241749853 ) ) ;
#28282 = SURFACE_STYLE_FILL_AREA ( #5959 ) ;
#28283 = ORIENTED_EDGE ( 'NONE', *, *, #13714, .F. ) ;
#28284 = CARTESIAN_POINT ( 'NONE',  ( 8.000000000000007105, 8.725776631572770725, -3.753907720748954180 ) ) ;
#28285 = CARTESIAN_POINT ( 'NONE',  ( 39.30000000000000426, 7.219292880973646134E-15, 0.000000000000000000 ) ) ;
#28286 = ORIENTED_EDGE ( 'NONE', *, *, #28165, .F. ) ;
#28287 = CARTESIAN_POINT ( 'NONE',  ( -35.50000000000000711, -114.9929510916434339, 12.60752341388803544 ) ) ;
#28288 = VERTEX_POINT ( 'NONE', #3586 ) ;
#28289 = AXIS2_PLACEMENT_3D ( 'NONE', #25185, #508, #22624 ) ;
#28290 = CARTESIAN_POINT ( 'NONE',  ( 7.999999999999992895, 46.77034588191305176, 22.72740077717247331 ) ) ;
#28291 = AXIS2_PLACEMENT_3D ( 'NONE', #35593, #30009, #16998 ) ;
#28292 = CARTESIAN_POINT ( 'NONE',  ( 0.000000000000000000, 11.27190672109280811, -0.3151488735047974776 ) ) ;
#28293 = ORIENTED_EDGE ( 'NONE', *, *, #30764, .T. ) ;
#28294 = CARTESIAN_POINT ( 'NONE',  ( 4.000000000000000000, 4.627536653468036720E-16, -45.89999999999999858 ) ) ;
#28295 = EDGE_LOOP ( 'NONE', ( #6769, #10775, #395, #18360 ) ) ;
#28296 = CARTESIAN_POINT ( 'NONE',  ( -35.50000000000000000, -115.0140978167138712, -0.3747823525984422255 ) ) ;
#28297 = DIRECTION ( 'NONE',  ( -1.047965281155519913E-16, -6.938893903907192632E-17, -1.000000000000000000 ) ) ;
#28298 = CARTESIAN_POINT ( 'NONE',  ( -36.11231047232249125, -112.0245472910329880, 2.722274454178448266 ) ) ;
#28299 = ADVANCED_FACE ( 'NONE', ( #25549 ), #11846, .T. ) ;
#28300 = ORIENTED_EDGE ( 'NONE', *, *, #27599, .T. ) ;
#28301 = CARTESIAN_POINT ( 'NONE',  ( -35.54388159064475872, -112.6276912846090568, 5.816024454178449155 ) ) ;
#28302 = CARTESIAN_POINT ( 'NONE',  ( -10.00000000000000000, 0.000000000000000000, 0.000000000000000000 ) ) ;
#28303 = CARTESIAN_POINT ( 'NONE',  ( -35.50000000000000000, -115.0631849411758196, -2.624765990393648885 ) ) ;
#28304 = ORIENTED_EDGE ( 'NONE', *, *, #27285, .F. ) ;
#28305 = ORIENTED_EDGE ( 'NONE', *, *, #34346, .F. ) ;
#28306 = CARTESIAN_POINT ( 'NONE',  ( -49.99999999999998579, -60.00000000000000000, 120.0000000000000000 ) ) ;
#28307 = CARTESIAN_POINT ( 'NONE',  ( 0.000000000000000000, 18.62763138773855687, 10.49404041845541968 ) ) ;
#28308 = ORIENTED_EDGE ( 'NONE', *, *, #21968, .F. ) ;
#28309 = EDGE_LOOP ( 'NONE', ( #21006, #4499 ) ) ;
#28310 = CARTESIAN_POINT ( 'NONE',  ( -34.50000000000000000, -112.0269151300720409, -0.7876962586524208776 ) ) ;
#28311 = CARTESIAN_POINT ( 'NONE',  ( 0.000000000000000000, 6.071532165918824830E-15, 1.000000000000000000 ) ) ;
#28312 = CIRCLE ( 'NONE', #25443, 15.49899999999998634 ) ;
#28313 = ORIENTED_EDGE ( 'NONE', *, *, #32798, .T. ) ;
#28314 = CIRCLE ( 'NONE', #12768, 7.499999999999992895 ) ;
#28315 = ORIENTED_EDGE ( 'NONE', *, *, #3980, .F. ) ;
#28316 = CARTESIAN_POINT ( 'NONE',  ( 8.000000000000007105, 11.27190672109271219, 0.3151488735049640111 ) ) ;
#28317 = EDGE_CURVE ( 'NONE', #31456, #29619, #20112, .T. ) ;
#28318 = CARTESIAN_POINT ( 'NONE',  ( -37.24999999999992184, -113.9929510916434339, 13.11852480586264846 ) ) ;
#28319 = CARTESIAN_POINT ( 'NONE',  ( -34.50000000000000000, -112.0140978167138712, 0.7502176474015694874 ) ) ;
#28320 = CARTESIAN_POINT ( 'NONE',  ( -49.99999999999999289, -25.98076211353320275, 84.99999999999994316 ) ) ;
#28321 = CARTESIAN_POINT ( 'NONE',  ( -35.95915003344518368, -113.9929510916434339, 13.11692036158763308 ) ) ;
#28322 = CARTESIAN_POINT ( 'NONE',  ( -35.50000000000000000, -115.9929510916434481, 10.53376102667243508 ) ) ;
#28323 = UNCERTAINTY_MEASURE_WITH_UNIT (LENGTH_MEASURE( 1.000000000000000082E-05 ), #3166, 'distance_accuracy_value', 'NONE');
#28324 = CYLINDRICAL_SURFACE ( 'NONE', #19849, 47.49900000000001654 ) ;
#28325 = FACE_OUTER_BOUND ( 'NONE', #4668, .T. ) ;
#28326 = EDGE_CURVE ( 'NONE', #34692, #6495, #3264, .T. ) ;
#28327 = CARTESIAN_POINT ( 'NONE',  ( 0.000000000000000000, -2.710505431213761085E-17, 54.99999999999999289 ) ) ;
#28328 = DIRECTION ( 'NONE',  ( -1.000000000000000000, 0.000000000000000000, 0.000000000000000000 ) ) ;
#28329 = FACE_OUTER_BOUND ( 'NONE', #8750, .T. ) ;
#28330 = ORIENTED_EDGE ( 'NONE', *, *, #5178, .F. ) ;
#28331 = DIRECTION ( 'NONE',  ( 0.000000000000000000, 1.000000000000000000, 0.000000000000000000 ) ) ;
#28332 = LINE ( 'NONE', #6895, #6631 ) ;
#28333 = AXIS2_PLACEMENT_3D ( 'NONE', #31857, #7190, #18169 ) ;
#28334 = DIRECTION ( 'NONE',  ( -1.000000000000000000, 0.000000000000000000, 0.000000000000000000 ) ) ;
#28335 = CARTESIAN_POINT ( 'NONE',  ( 0.000000000000000000, 0.000000000000000000, -1.200000000000006617 ) ) ;
#28336 = DIRECTION ( 'NONE',  ( -1.000000000000000000, 0.000000000000000000, -0.000000000000000000 ) ) ;
#28337 = DIRECTION ( 'NONE',  ( 1.000000000000000000, 0.000000000000000000, 0.000000000000000000 ) ) ;
#28338 = ORIENTED_EDGE ( 'NONE', *, *, #22742, .F. ) ;
#28339 = DIRECTION ( 'NONE',  ( 0.000000000000000000, 0.5877852522924739143, -0.8090169943749468962 ) ) ;
#28340 = DIRECTION ( 'NONE',  ( 0.000000000000000000, 0.000000000000000000, -1.000000000000000000 ) ) ;
#28341 = DIRECTION ( 'NONE',  ( 0.000000000000000000, 0.5000000000000031086, -0.8660254037844368202 ) ) ;
#28342 = ORIENTED_EDGE ( 'NONE', *, *, #714, .T. ) ;
#28343 = EDGE_LOOP ( 'NONE', ( #6022, #16147, #29827, #13666 ) ) ;
#28344 = CARTESIAN_POINT ( 'NONE',  ( -37.97545270896702618, -114.4734759653044023, 7.652725545821552622 ) ) ;
#28345 = VERTEX_POINT ( 'NONE', #10040 ) ;
#28346 = FILL_AREA_STYLE_COLOUR ( '', #31669 ) ;
#28348 = VERTEX_POINT ( 'NONE', #5192 ) ;
#28347 = AXIS2_PLACEMENT_3D ( 'NONE', #31380, #25988, #1314 ) ;
#28349 = VERTEX_POINT ( 'NONE', #26793 ) ;
#28350 = CYLINDRICAL_SURFACE ( 'NONE', #15437, 9.499000000000000554 ) ;
#28351 = CIRCLE ( 'NONE', #27772, 3.999999999999993339 ) ;
#28352 = DIRECTION ( 'NONE',  ( 1.000000000000000000, 1.734723475976807094E-16, 0.000000000000000000 ) ) ;
#28353 = DIRECTION ( 'NONE',  ( -1.000000000000000000, 0.000000000000000000, 0.000000000000000000 ) ) ;
#28354 = VECTOR ( 'NONE', #35345, 1000.000000000000000 ) ;
#28355 = EDGE_CURVE ( 'NONE', #15935, #31584, #7158, .T. ) ;
#28356 = CARTESIAN_POINT ( 'NONE',  ( -36.01562499999996447, -114.9929510916434339, 13.11852480586264669 ) ) ;
#28357 = DIRECTION ( 'NONE',  ( 0.000000000000000000, -0.9510565162951502005, -0.3090169943749580539 ) ) ;
#28358 = EDGE_CURVE ( 'NONE', #29334, #5158, #7514, .T. ) ;
#28359 = VECTOR ( 'NONE', #93, 1000.000000000000000 ) ;
#28360 = DIRECTION ( 'NONE',  ( -1.000000000000000000, -1.734723475976807094E-16, 0.000000000000000000 ) ) ;
#28361 = CARTESIAN_POINT ( 'NONE',  ( -34.50000000000000000, -114.3464919575557843, 9.568884482464163455 ) ) ;
#28362 = DIRECTION ( 'NONE',  ( -0.000000000000000000, 0.000000000000000000, -1.000000000000000000 ) ) ;
#28363 = CARTESIAN_POINT ( 'NONE',  ( -1.498621416870349332, 0.000000000000000000, 0.000000000000000000 ) ) ;
#28364 = VERTEX_POINT ( 'NONE', #34718 ) ;
#28365 = EDGE_CURVE ( 'NONE', #16103, #8708, #15879, .T. ) ;
#28366 = CARTESIAN_POINT ( 'NONE',  ( -35.50000000000000000, -115.9929524668003182, 10.51038305125561401 ) ) ;
#28367 = CARTESIAN_POINT ( 'NONE',  ( -35.50000000000000711, -112.9876085932806262, 1.879154677457530065 ) ) ;
#28368 = CARTESIAN_POINT ( 'NONE',  ( -34.49999999999998579, -25.98076211353320986, 84.99999999999994316 ) ) ;
#28369 = DIRECTION ( 'NONE',  ( 1.000000000000000000, -0.000000000000000000, -0.000000000000000000 ) ) ;
#28370 = CIRCLE ( 'NONE', #25498, 14.00000000000000000 ) ;
#28371 = DIRECTION ( 'NONE',  ( -1.000000000000000000, -0.000000000000000000, 0.000000000000000000 ) ) ;
#28372 = CARTESIAN_POINT ( 'NONE',  ( 0.000000000000000000, 0.000000000000000000, 0.000000000000000000 ) ) ;
#28373 = CARTESIAN_POINT ( 'NONE',  ( 7.999999999999992895, -36.34385289850568057, -29.77717097092114074 ) ) ;
#28374 = DIRECTION ( 'NONE',  ( 1.226634733346697831E-16, 0.7071067811865507924, -0.7071067811865441310 ) ) ;
#28375 = ORIENTED_EDGE ( 'NONE', *, *, #33776, .F. ) ;
#28376 = CARTESIAN_POINT ( 'NONE',  ( -36.02454729103298092, -114.4734759653044307, 1.597274454178448932 ) ) ;
#28377 = FACE_OUTER_BOUND ( 'NONE', #22929, .T. ) ;
#28378 = PLANE ( 'NONE',  #20541 ) ;
#28379 = ORIENTED_EDGE ( 'NONE', *, *, #7627, .T. ) ;
#28380 = VERTEX_POINT ( 'NONE', #27151 ) ;
#28381 = CIRCLE ( 'NONE', #212, 47.49900000000000944 ) ;
#28382 = CARTESIAN_POINT ( 'NONE',  ( -4.747884751462066788, -5.143694235356003119, 0.000000000000000000 ) ) ;
#28383 = VECTOR ( 'NONE', #25317, 1000.000000000000000 ) ;
#28384 = FACE_OUTER_BOUND ( 'NONE', #17850, .T. ) ;
#28385 = EDGE_LOOP ( 'NONE', ( #536, #12498 ) ) ;
#28386 = CARTESIAN_POINT ( 'NONE',  ( -40.02454729103296671, -115.1833782841879525, 8.159774454178448266 ) ) ;
#28387 = ORIENTED_EDGE ( 'NONE', *, *, #26888, .T. ) ;
#28388 = EDGE_CURVE ( 'NONE', #16289, #272, #21043, .T. ) ;
#28389 = TOROIDAL_SURFACE ( 'NONE', #29570, 4.200000000000000178, 0.1999999999999998723 ) ;
#28390 = CYLINDRICAL_SURFACE ( 'NONE', #18122, 3.799999999999999822 ) ;
#28391 = FACE_OUTER_BOUND ( 'NONE', #17695, .T. ) ;
#28392 = APPLICATION_PROTOCOL_DEFINITION ( 'draft international standard', 'automotive_design', 1998, #1346 ) ;
#28393 = DIRECTION ( 'NONE',  ( 0.000000000000000000, -0.9848077530122097967, 0.1736481776669208388 ) ) ;
#28394 = ORIENTED_EDGE ( 'NONE', *, *, #16264, .T. ) ;
#28395 = ORIENTED_EDGE ( 'NONE', *, *, #15678, .T. ) ;
#28396 = VECTOR ( 'NONE', #20279, 1000.000000000000000 ) ;
#28397 = ADVANCED_FACE ( 'NONE', ( #26438 ), #34539, .T. ) ;
#28398 = DIRECTION ( 'NONE',  ( -1.000000000000000000, 0.000000000000000000, 0.000000000000000000 ) ) ;
#28399 = DIRECTION ( 'NONE',  ( -1.000000000000000000, 0.000000000000000000, 0.000000000000000000 ) ) ;
#28400 = EDGE_CURVE ( 'NONE', #3028, #34652, #5008, .T. ) ;
#28401 = EDGE_CURVE ( 'NONE', #17782, #8803, #29494, .T. ) ;
#28402 = ORIENTED_EDGE ( 'NONE', *, *, #20227, .T. ) ;
#28403 = CARTESIAN_POINT ( 'NONE',  ( 50.00000000000000000, -59.99999999999997158, 120.0000000000000000 ) ) ;
#28404 = CARTESIAN_POINT ( 'NONE',  ( -34.50000000000000000, -112.9876085932806262, 1.879154677457530065 ) ) ;
#28405 = DIRECTION ( 'NONE',  ( -1.000000000000000000, 0.000000000000000000, 0.000000000000000000 ) ) ;
#28406 = CARTESIAN_POINT ( 'NONE',  ( 0.000000000000000000, 0.000000000000000000, 0.000000000000000000 ) ) ;
#28407 = AXIS2_PLACEMENT_3D ( 'NONE', #6632, #34552, #3963 ) ;
#28408 = CARTESIAN_POINT ( 'NONE',  ( -34.50000000000000000, -115.9929510916434481, 10.59426868253284226 ) ) ;
#28409 = AXIS2_PLACEMENT_3D ( 'NONE', #7019, #28817, #20689 ) ;
#28410 = DIRECTION ( 'NONE',  ( -1.000000000000000000, -0.000000000000000000, -0.000000000000000000 ) ) ;
#28411 = CARTESIAN_POINT ( 'NONE',  ( -35.62769128460905677, -115.4561184093552413, 1.691024454178448710 ) ) ;
#28412 = EDGE_CURVE ( 'NONE', #1640, #33383, #3831, .T. ) ;
#28413 = CARTESIAN_POINT ( 'NONE',  ( -37.62254989966454133, -114.9929510916434339, 14.11371147303758278 ) ) ;
#28414 = CARTESIAN_POINT ( 'NONE',  ( -4.000000000000000000, -2.710505431213761085E-17, -54.99999999999999289 ) ) ;
#28415 = EDGE_CURVE ( 'NONE', #14157, #18547, #8410, .T. ) ;
#28416 = CARTESIAN_POINT ( 'NONE',  ( -42.49999999999999289, -29.98076211353323828, 86.49999999999990052 ) ) ;
#28417 = DIRECTION ( 'NONE',  ( 1.000000000000000000, 0.000000000000000000, 0.000000000000000000 ) ) ;
#28418 = CARTESIAN_POINT ( 'NONE',  ( 8.000000000000000000, 11.11653975335807587, -12.74840161668719851 ) ) ;
#28419 = ORIENTED_EDGE ( 'NONE', *, *, #13745, .T. ) ;
#28420 = DIRECTION ( 'NONE',  ( 0.000000000000000000, -0.3420201433256756518, 0.9396926207859058744 ) ) ;
#28421 = ORIENTED_EDGE ( 'NONE', *, *, #26127, .F. ) ;
#28422 = CARTESIAN_POINT ( 'NONE',  ( -33.97545270896703329, -115.1833782841879810, 4.090225545821551734 ) ) ;
#28423 = CARTESIAN_POINT ( 'NONE',  ( 0.000000000000000000, -7.613867765417531075, 5.679790370316011305 ) ) ;
#28424 = CARTESIAN_POINT ( 'NONE',  ( -35.50000000000000711, -112.0140978167138712, 0.3752176474015640473 ) ) ;
#28425 = ORIENTED_EDGE ( 'NONE', *, *, #12873, .T. ) ;
#28426 = ORIENTED_EDGE ( 'NONE', *, *, #6134, .F. ) ;
#28427 = CARTESIAN_POINT ( 'NONE',  ( 0.000000000000000000, -2.710505431213761085E-17, 55.00000000000000000 ) ) ;
#28428 = CARTESIAN_POINT ( 'NONE',  ( 8.000000000000000000, 0.000000000000000000, 0.000000000000000000 ) ) ;
#28429 = EDGE_LOOP ( 'NONE', ( #7203, #17831, #11773, #618 ) ) ;
#28430 = ORIENTED_EDGE ( 'NONE', *, *, #21512, .F. ) ;
#28431 = EDGE_CURVE ( 'NONE', #27252, #32280, #18495, .T. ) ;
#28432 = AXIS2_PLACEMENT_3D ( 'NONE', #24809, #132, #11123 ) ;
#28433 = FACE_OUTER_BOUND ( 'NONE', #6541, .T. ) ;
#28434 = VECTOR ( 'NONE', #6312, 1000.000000000000000 ) ;
#28435 = ORIENTED_EDGE ( 'NONE', *, *, #1378, .T. ) ;
#28437 = ORIENTED_EDGE ( 'NONE', *, *, #23302, .T. ) ;
#28436 = EDGE_CURVE ( 'NONE', #31548, #33309, #28540, .T. ) ;
#28438 = CARTESIAN_POINT ( 'NONE',  ( -37.88768952767750875, -112.0245472910329880, 5.027725545821550845 ) ) ;
#28439 = ADVANCED_FACE ( 'NONE', ( #1769 ), #12573, .T. ) ;
#28440 = AXIS2_PLACEMENT_3D ( 'NONE', #6807, #1066, #20293 ) ;
#28441 = PLANE ( 'NONE',  #4124 ) ;
#28442 = ORIENTED_EDGE ( 'NONE', *, *, #6781, .F. ) ;
#28443 = VERTEX_POINT ( 'NONE', #9858 ) ;
#28444 = CARTESIAN_POINT ( 'NONE',  ( -35.50000000000000000, -116.9884631899972476, -0.9506101647064282290 ) ) ;
#28445 = EDGE_CURVE ( 'NONE', #34437, #28224, #4490, .T. ) ;
#28446 = DIRECTION ( 'NONE',  ( 0.000000000000000000, 0.000000000000000000, 1.000000000000000000 ) ) ;
#28447 = ORIENTED_EDGE ( 'NONE', *, *, #8840, .T. ) ;
#28448 = ADVANCED_FACE ( 'NONE', ( #21196 ), #13121, .T. ) ;
#28449 = CARTESIAN_POINT ( 'NONE',  ( -37.98402046630260287, -114.9929510916434339, 12.74811950270164118 ) ) ;
#28450 = CARTESIAN_POINT ( 'NONE',  ( -39.00000000000000000, -113.9929510916434339, 12.26648026267477221 ) ) ;
#28451 = DIRECTION ( 'NONE',  ( -1.000000000000000000, 0.000000000000000000, 0.000000000000000000 ) ) ;
#28452 = LINE ( 'NONE', #25582, #11668 ) ;
#28453 = CARTESIAN_POINT ( 'NONE',  ( -37.51022648969539119, -113.9929510916434339, 14.11852173794918563 ) ) ;
#28454 = DIRECTION ( 'NONE',  ( 0.000000000000000000, 0.9048270524660175784, 0.4257792915650768784 ) ) ;
#28455 = EDGE_CURVE ( 'NONE', #27081, #4678, #31985, .T. ) ;
#28456 = CARTESIAN_POINT ( 'NONE',  ( -35.50000000000000711, -114.9929510916434339, 12.17846912687782712 ) ) ;
#28457 = FILL_AREA_STYLE ('',( #28642 ) ) ;
#28458 = EDGE_LOOP ( 'NONE', ( #1651, #736, #18003, #27622 ) ) ;
#28459 = CARTESIAN_POINT ( 'NONE',  ( 0.000000000000000000, 18.62763138773856397, -2.494040418455147456 ) ) ;
#28460 = FACE_OUTER_BOUND ( 'NONE', #1416, .T. ) ;
#28461 = VERTEX_POINT ( 'NONE', #13291 ) ;
#28462 = CARTESIAN_POINT ( 'NONE',  ( -35.95915003344517658, -114.9929510916434339, 13.11692036158763308 ) ) ;
#28463 = ORIENTED_EDGE ( 'NONE', *, *, #9282, .F. ) ;
#28464 = DIRECTION ( 'NONE',  ( 0.000000000000000000, -0.9510565162951565288, 0.3090169943749383474 ) ) ;
#28465 = AXIS2_PLACEMENT_3D ( 'NONE', #27513, #18857, #5881 ) ;
#28466 = ORIENTED_EDGE ( 'NONE', *, *, #17176, .F. ) ;
#28467 = DIRECTION ( 'NONE',  ( 0.000000000000000000, 0.000000000000000000, -1.000000000000000000 ) ) ;
#28468 = ORIENTED_EDGE ( 'NONE', *, *, #29600, .F. ) ;
#28469 = VECTOR ( 'NONE', #13223, 1000.000000000000000 ) ;
#28470 = CARTESIAN_POINT ( 'NONE',  ( -35.50000000000000000, -113.3474311500483935, -0.6247823525984269599 ) ) ;
#28471 = DIRECTION ( 'NONE',  ( 1.000000000000000000, -0.000000000000000000, -0.000000000000000000 ) ) ;
#28472 = CARTESIAN_POINT ( 'NONE',  ( -38.99999999999999289, -113.9407375970686900, 5.253524454178449155 ) ) ;
#28473 = EDGE_LOOP ( 'NONE', ( #33438, #34018 ) ) ;
#28474 = CARTESIAN_POINT ( 'NONE',  ( -37.76916472181487450, -111.9754527089670404, 4.034774454178449155 ) ) ;
#28475 = ADVANCED_FACE ( 'NONE', ( #35256 ), #2490, .F. ) ;
#28476 = EDGE_CURVE ( 'NONE', #5329, #14055, #16446, .T. ) ;
#28477 = DIRECTION ( 'NONE',  ( 0.000000000000000000, 0.000000000000000000, -1.000000000000000000 ) ) ;
#28478 = CARTESIAN_POINT ( 'NONE',  ( -35.50000000000000711, -113.0974311500471714, -1.624782352598427959 ) ) ;
#28479 = ORIENTED_EDGE ( 'NONE', *, *, #2033, .T. ) ;
#28480 = ORIENTED_EDGE ( 'NONE', *, *, #3391, .T. ) ;
#28481 = DIRECTION ( 'NONE',  ( -1.000000000000000000, 0.000000000000000000, 0.000000000000000000 ) ) ;
#28482 = CYLINDRICAL_SURFACE ( 'NONE', #9831, 47.49900000000001654 ) ;
#28483 = ORIENTED_EDGE ( 'NONE', *, *, #16140, .F. ) ;
#28484 = ORIENTED_EDGE ( 'NONE', *, *, #3857, .T. ) ;
#28485 = CARTESIAN_POINT ( 'NONE',  ( -34.50000000000000000, -115.9630435732166518, -0.9469505670456015434 ) ) ;
#28486 = CARTESIAN_POINT ( 'NONE',  ( 50.00000000000000000, -25.98076211353320275, 84.99999999999992895 ) ) ;
#28487 = PRODUCT_DEFINITION_SHAPE ( 'NONE', 'NONE',  #35631 ) ;
#28488 = CIRCLE ( 'NONE', #35387, 17.49900000000001299 ) ;
#28489 = ADVANCED_FACE ( 'NONE', ( #10936 ), #30026, .T. ) ;
#28490 = EDGE_LOOP ( 'NONE', ( #25098, #15975, #11803, #19084 ) ) ;
#28491 = VERTEX_POINT ( 'NONE', #30722 ) ;
#28492 = EDGE_CURVE ( 'NONE', #23109, #6425, #6688, .T. ) ;
#28493 = PLANE ( 'NONE',  #32731 ) ;
#28494 = CIRCLE ( 'NONE', #5501, 9.999999999999994671 ) ;
#28495 = CARTESIAN_POINT ( 'NONE',  ( -37.42187499999996447, -113.9929510916434339, 13.11852480586264846 ) ) ;
#28496 = CARTESIAN_POINT ( 'NONE',  ( 7.999999999999992895, 20.99948489194482448, -42.60488980472762677 ) ) ;
#28497 = CARTESIAN_POINT ( 'NONE',  ( 0.000000000000000000, -10.62435788049434038, -13.16139124467930444 ) ) ;
#28498 = CARTESIAN_POINT ( 'NONE',  ( -35.50040135968784938, -113.9929510916434339, 12.63896776382214071 ) ) ;
#28499 = CARTESIAN_POINT ( 'NONE',  ( -35.50000000000000000, -115.9929510916434481, 12.17846912687782712 ) ) ;
#28500 = AXIS2_PLACEMENT_3D ( 'NONE', #21761, #11150, #24835 ) ;
#28501 = CARTESIAN_POINT ( 'NONE',  ( 7.999999999999992895, 0.000000000000000000, 0.000000000000000000 ) ) ;
#28502 = CARTESIAN_POINT ( 'NONE',  ( 0.000000000000000000, -2.710505431213761085E-17, -45.10000000000000142 ) ) ;
#28503 = CARTESIAN_POINT ( 'NONE',  ( -9.999999999999994671, 0.000000000000000000, 0.000000000000000000 ) ) ;
#28504 = DIRECTION ( 'NONE',  ( 1.000000000000000000, -0.000000000000000000, 0.000000000000000000 ) ) ;
#28505 = ORIENTED_EDGE ( 'NONE', *, *, #26272, .T. ) ;
#28506 = CARTESIAN_POINT ( 'NONE',  ( 0.000000000000000000, 49.65209126885763169, 15.44894276735568539 ) ) ;
#28507 = CARTESIAN_POINT ( 'NONE',  ( 23.00000000000000000, 11.00000000000000533, 0.000000000000000000 ) ) ;
#28508 = CIRCLE ( 'NONE', #12997, 7.199999999999992184 ) ;
#28509 = DIRECTION ( 'NONE',  ( -1.000000000000000000, -1.734723475976807094E-16, 0.000000000000000000 ) ) ;
#28510 = DIRECTION ( 'NONE',  ( -1.000000000000000000, -0.000000000000000000, 0.000000000000000000 ) ) ;
#28511 = ITEM_DEFINED_TRANSFORMATION ( 'NONE', 'NONE', #33979,  #21307 ) ;
#28512 = CARTESIAN_POINT ( 'NONE',  ( 50.00000000000000000, 20.00000000000001776, 120.0000000000000000 ) ) ;
#28513 = DIRECTION ( 'NONE',  ( 0.9914448613738107152, -0.1305261922200497138, -2.588645552990029003E-31 ) ) ;
#28514 = CIRCLE ( 'NONE', #13561, 10.50000000000000178 ) ;
#28515 = CIRCLE ( 'NONE', #27401, 20.00000000000001066 ) ;
#28516 = EDGE_LOOP ( 'NONE', ( #32575, #6550, #32152, #21854 ) ) ;
#28517 = AXIS2_PLACEMENT_3D ( 'NONE', #6767, #14864, #12348 ) ;
#28518 = VECTOR ( 'NONE', #14022, 1000.000000000000000 ) ;
#28519 = EDGE_CURVE ( 'NONE', #32982, #3028, #11456, .T. ) ;
#28520 = CARTESIAN_POINT ( 'NONE',  ( 3.799999999999999822, 4.653657836759942730E-16, -50.00000000000000000 ) ) ;
#28521 = CARTESIAN_POINT ( 'NONE',  ( -34.50000000000000000, -117.0140978167138854, -0.4685323525984310122 ) ) ;
#28522 = DIRECTION ( 'NONE',  ( -1.000000000000000000, -0.000000000000000000, -0.000000000000000000 ) ) ;
#28523 = ORIENTED_EDGE ( 'NONE', *, *, #33440, .T. ) ;
#28524 = EDGE_LOOP ( 'NONE', ( #32210, #3484, #17123, #26400 ) ) ;
#28525 = CARTESIAN_POINT ( 'NONE',  ( -36.33479806579560289, -113.2509883718313262, 9.808975545821553510 ) ) ;
#28526 = EDGE_LOOP ( 'NONE', ( #21702, #22555, #11133, #14962, #14871, #19860 ) ) ;
#28527 = AXIS2_PLACEMENT_3D ( 'NONE', #31217, #25999, #9252 ) ;
#28528 =( NAMED_UNIT ( * ) SI_UNIT ( $, .STERADIAN. ) SOLID_ANGLE_UNIT ( ) );
#28529 = ORIENTED_EDGE ( 'NONE', *, *, #29628, .F. ) ;
#28530 = ORIENTED_EDGE ( 'NONE', *, *, #11610, .F. ) ;
#28531 = CARTESIAN_POINT ( 'NONE',  ( -34.50000000000000000, -113.0140978167142833, 0.8752176474015604946 ) ) ;
#28532 =( REPRESENTATION_RELATIONSHIP ('NONE','NONE', #26607, #2005 ) REPRESENTATION_RELATIONSHIP_WITH_TRANSFORMATION ( #11954 )SHAPE_REPRESENTATION_RELATIONSHIP( ) );
#28533 = CARTESIAN_POINT ( 'NONE',  ( -35.50000000000000711, -113.4307644833805000, -1.624782352598427959 ) ) ;
#28534 = CARTESIAN_POINT ( 'NONE',  ( 8.000000000000000000, 0.000000000000000000, 0.000000000000000000 ) ) ;
#28535 = VECTOR ( 'NONE', #24712, 1000.000000000000000 ) ;
#28536 = CARTESIAN_POINT ( 'NONE',  ( -36.24999999999983658, -114.9929510916434339, 13.11852480586264669 ) ) ;
#28537 = CARTESIAN_POINT ( 'NONE',  ( 8.000000000000000000, -13.24207120356955159, -14.98824707027454828 ) ) ;
#28538 = CYLINDRICAL_SURFACE ( 'NONE', #3968, 8.000000000000001776 ) ;
#28539 = VECTOR ( 'NONE', #16749, 1000.000000000000000 ) ;
#28540 = CIRCLE ( 'NONE', #33698, 9.999999999999994671 ) ;
#28541 = CARTESIAN_POINT ( 'NONE',  ( -34.50000000000000000, -114.1489256397697289, 9.518467544735724317 ) ) ;
#28542 = FACE_OUTER_BOUND ( 'NONE', #10238, .T. ) ;
#28543 = VECTOR ( 'NONE', #27988, 1000.000000000000000 ) ;
#28544 = CIRCLE ( 'NONE', #18208, 7.200000000000000178 ) ;
#28545 = CYLINDRICAL_SURFACE ( 'NONE', #30705, 11.00000000000001066 ) ;
#28546 = EDGE_LOOP ( 'NONE', ( #32983, #30357, #28564, #24983 ) ) ;
#28547 = CARTESIAN_POINT ( 'NONE',  ( -35.50000000000000000, -114.1835524127412924, 8.514811007161055656 ) ) ;
#28548 = CARTESIAN_POINT ( 'NONE',  ( -35.50000000000000711, -112.0154707866092707, 0.9357013553229778235 ) ) ;
#28549 = FILL_AREA_STYLE_COLOUR ( '', #12185 ) ;
#28550 = AXIS2_PLACEMENT_3D ( 'NONE', #10681, #10865, #32110 ) ;
#28551 = CARTESIAN_POINT ( 'NONE',  ( 0.000000000000000000, -30.03615769709762873, 42.44795908868979950 ) ) ;
#28552 = DIRECTION ( 'NONE',  ( -1.734723475976807094E-16, 1.000000000000000000, -1.067522139062650474E-15 ) ) ;
#28553 = AXIS2_PLACEMENT_3D ( 'NONE', #11619, #17191, #25146 ) ;
#28554 = CARTESIAN_POINT ( 'NONE',  ( 4.000000000000003553, -15.17386234660370370, -15.92965478239635679 ) ) ;
#28555 = CYLINDRICAL_SURFACE ( 'NONE', #20985, 15.49899999999998457 ) ;
#28556 = CARTESIAN_POINT ( 'NONE',  ( 0.000000000000000000, -2.710505431213761085E-17, 30.00000000000000000 ) ) ;
#28557 = FACE_OUTER_BOUND ( 'NONE', #5892, .T. ) ;
#28558 = VERTEX_POINT ( 'NONE', #17017 ) ;
#28559 = CARTESIAN_POINT ( 'NONE',  ( -37.05926240293131713, -113.0000000000000000, 9.621475545821549957 ) ) ;
#28560 = DIRECTION ( 'NONE',  ( 0.000000000000000000, -0.8660254037844392627, 0.4999999999999989453 ) ) ;
#28561 = DIRECTION ( 'NONE',  ( 0.000000000000000000, 0.000000000000000000, 1.000000000000000000 ) ) ;
#28562 = ORIENTED_EDGE ( 'NONE', *, *, #3765, .T. ) ;
#28563 = CIRCLE ( 'NONE', #2141, 10.99999999999999822 ) ;
#28564 = ORIENTED_EDGE ( 'NONE', *, *, #21635, .F. ) ;
#28565 = EDGE_CURVE ( 'NONE', #16796, #6240, #5364, .T. ) ;
#28566 = AXIS2_PLACEMENT_3D ( 'NONE', #19203, #30203, #24976 ) ;
#28567 = CARTESIAN_POINT ( 'NONE',  ( 7.999999999999992895, -35.20873326984104068, 31.88259874184018372 ) ) ;
#28568 = ORIENTED_EDGE ( 'NONE', *, *, #11800, .T. ) ;
#28569 = CARTESIAN_POINT ( 'NONE',  ( -34.02454729103297382, -112.6980969099494132, 8.402725545821549957 ) ) ;
#28570 = ORIENTED_EDGE ( 'NONE', *, *, #8965, .T. ) ;
#28571 = AXIS2_PLACEMENT_3D ( 'NONE', #25586, #9894, #6661 ) ;
#28572 = CIRCLE ( 'NONE', #18795, 20.00000000000000355 ) ;
#28573 = LINE ( 'NONE', #13519, #23584 ) ;
#28574 = CIRCLE ( 'NONE', #28009, 47.49900000000000944 ) ;
#28575 = DIRECTION ( 'NONE',  ( -1.000000000000000000, 0.000000000000000000, 0.000000000000000000 ) ) ;
#28576 = CARTESIAN_POINT ( 'NONE',  ( 0.000000000000000000, 29.60891106212840285, -37.14118181634734839 ) ) ;
#28577 = EDGE_CURVE ( 'NONE', #24996, #9078, #4985, .T. ) ;
#28578 = PRODUCT_CONTEXT ( 'NONE', #7346, 'mechanical' ) ;
#28579 = CARTESIAN_POINT ( 'NONE',  ( -10.00000000000000178, 0.000000000000000000, 0.000000000000000000 ) ) ;
#28580 = VERTEX_POINT ( 'NONE', #16309 ) ;
#28581 = EDGE_LOOP ( 'NONE', ( #31181, #2622, #26157, #19651 ) ) ;
#28582 = CARTESIAN_POINT ( 'NONE',  ( 70.00001200000001234, -26.50436088913151522, 80.99999999999990052 ) ) ;
#28583 = FACE_OUTER_BOUND ( 'NONE', #20894, .T. ) ;
#28584 = VERTEX_POINT ( 'NONE', #13631 ) ;
#28585 = CARTESIAN_POINT ( 'NONE',  ( 50.00000000000000711, 0.000000000000000000, 64.00000000000000000 ) ) ;
#28586 = VECTOR ( 'NONE', #5667, 1000.000000000000000 ) ;
#28587 = CARTESIAN_POINT ( 'NONE',  ( -34.50000000000000000, -113.0140978167139991, -0.6247823525984269599 ) ) ;
#28588 = CARTESIAN_POINT ( 'NONE',  ( 4.747884751462025044, -5.143694235356003119, -0.7999999999999951594 ) ) ;
#28589 = DIRECTION ( 'NONE',  ( 0.000000000000000000, 0.000000000000000000, 1.000000000000000000 ) ) ;
#28590 = CARTESIAN_POINT ( 'NONE',  ( -34.50000000000000000, -115.9874658933321001, 10.35517832894335832 ) ) ;
#28591 = AXIS2_PLACEMENT_3D ( 'NONE', #30727, #11626, #28033 ) ;
#28592 = DIRECTION ( 'NONE',  ( 0.02040816326530624225, 0.9997917317482359900, -1.513872302910508719E-31 ) ) ;
#28593 = DIRECTION ( 'NONE',  ( 0.000000000000000000, 0.000000000000000000, 1.000000000000000000 ) ) ;
#28594 = CARTESIAN_POINT ( 'NONE',  ( -39.00000000000000711, -114.9929510916434339, 12.50851088611646311 ) ) ;
#28595 = CARTESIAN_POINT ( 'NONE',  ( 7.999999999999992895, -46.90537658765333617, 2.727856614654147638 ) ) ;
#28596 = EDGE_CURVE ( 'NONE', #6533, #12194, #2668, .T. ) ;
#28597 = VECTOR ( 'NONE', #8349, 1000.000000000000000 ) ;
#28598 = FACE_BOUND ( 'NONE', #16472, .T. ) ;
#28599 = AXIS2_PLACEMENT_3D ( 'NONE', #5253, #2212, #7749 ) ;
#28600 = CYLINDRICAL_SURFACE ( 'NONE', #23934, 4.000000000000000000 ) ;
#28601 = CARTESIAN_POINT ( 'NONE',  ( 0.000000000000000000, -2.710505431213761085E-17, -45.10000000000000142 ) ) ;
#28602 = CIRCLE ( 'NONE', #10773, 19.99999999999998579 ) ;
#28603 = DIRECTION ( 'NONE',  ( -1.000000000000000000, 0.000000000000000000, -0.000000000000000000 ) ) ;
#28604 = EDGE_LOOP ( 'NONE', ( #20044, #29733, #567, #23052 ) ) ;
#28605 = CARTESIAN_POINT ( 'NONE',  ( -34.02454729103297382, -112.6980969099494132, 3.902725545821552178 ) ) ;
#28606 = CIRCLE ( 'NONE', #9063, 7.199999999999998401 ) ;
#28607 = DIRECTION ( 'NONE',  ( 0.000000000000000000, 0.8660254037844364872, 0.5000000000000036637 ) ) ;
#28608 = CARTESIAN_POINT ( 'NONE',  ( -35.50000000000000000, -113.0140978167138712, -0.3747823525984258497 ) ) ;
#28609 = VERTEX_POINT ( 'NONE', #19199 ) ;
#28610 = EDGE_LOOP ( 'NONE', ( #11355, #32368, #19255, #13633, #24056, #21297, #31579, #7559 ) ) ;
#28611 = EDGE_CURVE ( 'NONE', #22897, #15158, #27978, .T. ) ;
#28612 = DIRECTION ( 'NONE',  ( 0.000000000000000000, 0.000000000000000000, -1.000000000000000000 ) ) ;
#28613 = DIRECTION ( 'NONE',  ( 0.000000000000000000, 0.000000000000000000, 1.000000000000000000 ) ) ;
#28614 = ORIENTED_EDGE ( 'NONE', *, *, #25274, .F. ) ;
#28615 = EDGE_CURVE ( 'NONE', #8278, #10254, #32572, .T. ) ;
#28616 = ADVANCED_FACE ( 'NONE', ( #5533 ), #19707, .F. ) ;
#28617 = VERTEX_POINT ( 'NONE', #24971 ) ;
#28618 = CIRCLE ( 'NONE', #18266, 52.00000000000000711 ) ;
#28619 = AXIS2_PLACEMENT_3D ( 'NONE', #34349, #23901, #15412 ) ;
#28620 = DIRECTION ( 'NONE',  ( 0.000000000000000000, 0.000000000000000000, 1.000000000000000000 ) ) ;
#28621 = ORIENTED_EDGE ( 'NONE', *, *, #32840, .F. ) ;
#28622 = CARTESIAN_POINT ( 'NONE',  ( -36.23083527818513261, -111.9754527089670404, 3.715225545821551290 ) ) ;
#28623 = ADVANCED_FACE ( 'NONE', ( #11112 ), #8045, .F. ) ;
#28624 = CIRCLE ( 'NONE', #2793, 4.000000000000000000 ) ;
#28625 = EDGE_CURVE ( 'NONE', #1924, #26408, #22080, .T. ) ;
#28626 = DIRECTION ( 'NONE',  ( 0.000000000000000000, 0.000000000000000000, 1.000000000000000000 ) ) ;
#28627 = ORIENTED_EDGE ( 'NONE', *, *, #24762, .F. ) ;
#28628 = ORIENTED_EDGE ( 'NONE', *, *, #2259, .F. ) ;
#28629 = CARTESIAN_POINT ( 'NONE',  ( -35.50000000000000000, -113.3474311500483935, -2.624782352598442614 ) ) ;
#28630 = AXIS2_PLACEMENT_3D ( 'NONE', #3734, #14687, #26054 ) ;
#28631 = UNCERTAINTY_MEASURE_WITH_UNIT (LENGTH_MEASURE( 1.000000000000000082E-05 ), #30444, 'distance_accuracy_value', 'NONE');
#28632 = CARTESIAN_POINT ( 'NONE',  ( 7.999999999999992895, -49.65209126885775248, 15.44894276735532479 ) ) ;
#28633 = ORIENTED_EDGE ( 'NONE', *, *, #33056, .F. ) ;
#28634 = CARTESIAN_POINT ( 'NONE',  ( -37.89983305244309975, -114.9929510916434339, 12.92579853460519246 ) ) ;
#28635 = CARTESIAN_POINT ( 'NONE',  ( -39.00000000000000000, -113.9929510916434339, 10.85830208992306822 ) ) ;
#28636 = DIRECTION ( 'NONE',  ( -1.000000000000000000, 0.000000000000000000, 0.000000000000000000 ) ) ;
#28637 = CARTESIAN_POINT ( 'NONE',  ( 8.000000000000000000, 0.000000000000000000, 0.000000000000000000 ) ) ;
#28638 = CARTESIAN_POINT ( 'NONE',  ( -36.01562499999997158, -113.9929510916434339, 14.11852480586265024 ) ) ;
#28639 = DIRECTION ( 'NONE',  ( 1.000000000000000000, -0.000000000000000000, -0.000000000000000000 ) ) ;
#28640 = ADVANCED_FACE ( 'NONE', ( #8392, #30381 ), #3019, .F. ) ;
#28641 = CARTESIAN_POINT ( 'NONE',  ( -37.18750000000006395, -114.9929510916434339, 13.11852480586264669 ) ) ;
#28642 = FILL_AREA_STYLE_COLOUR ( '', #21610 ) ;
#28643 = ORIENTED_EDGE ( 'NONE', *, *, #20054, .F. ) ;
#28644 = DIRECTION ( 'NONE',  ( -1.000000000000000000, 0.000000000000000000, 0.000000000000000000 ) ) ;
#28645 = DIRECTION ( 'NONE',  ( -0.000000000000000000, 0.000000000000000000, -1.000000000000000000 ) ) ;
#28646 = ORIENTED_EDGE ( 'NONE', *, *, #21115, .F. ) ;
#28647 = EDGE_CURVE ( 'NONE', #3876, #33861, #30879, .T. ) ;
#28648 = CARTESIAN_POINT ( 'NONE',  ( -35.50000000000000711, -114.9929510916434339, 12.39849696637031506 ) ) ;
#28649 = ORIENTED_EDGE ( 'NONE', *, *, #12831, .F. ) ;
#28650 = CIRCLE ( 'NONE', #18275, 20.00000000000000355 ) ;
#28651 = CARTESIAN_POINT ( 'NONE',  ( -35.00000000000000000, -114.0592624029313242, 1.503524454178448710 ) ) ;
#28652 = ORIENTED_EDGE ( 'NONE', *, *, #10109, .T. ) ;
#28653 = AXIS2_PLACEMENT_3D ( 'NONE', #659, #3559, #30917 ) ;
#28654 = CYLINDRICAL_SURFACE ( 'NONE', #35462, 4.000000000000000000 ) ;
#28655 = ORIENTED_EDGE ( 'NONE', *, *, #34254, .T. ) ;
#28656 = EDGE_CURVE ( 'NONE', #8054, #10239, #28572, .T. ) ;
#28657 = CARTESIAN_POINT ( 'NONE',  ( -34.50000000000000000, -113.1061333991432321, 0.8862035858144284850 ) ) ;
#28658 = DIRECTION ( 'NONE',  ( -1.000000000000000000, -0.000000000000000000, 0.000000000000000000 ) ) ;
#28659 = CARTESIAN_POINT ( 'NONE',  ( 8.000000000000007105, 0.000000000000000000, 0.000000000000000000 ) ) ;
#28660 = ADVANCED_FACE ( 'NONE', ( #8921 ), #4089, .T. ) ;
#28661 = EDGE_CURVE ( 'NONE', #15482, #2330, #11621, .T. ) ;
#28662 = ORIENTED_EDGE ( 'NONE', *, *, #21174, .T. ) ;
#28663 = AXIS2_PLACEMENT_3D ( 'NONE', #3029, #5717, #19388 ) ;
#28664 = CARTESIAN_POINT ( 'NONE',  ( -36.23083527818512550, -116.0245472910329880, 4.784774454178448266 ) ) ;
#28665 = DIRECTION ( 'NONE',  ( -1.000000000000000000, 0.000000000000000000, 0.000000000000000000 ) ) ;
#28666 = CARTESIAN_POINT ( 'NONE',  ( -35.50000000000000711, -115.5178116849130276, -1.498529437126731034 ) ) ;
#28667 = ORIENTED_EDGE ( 'NONE', *, *, #10156, .F. ) ;
#28668 = EDGE_LOOP ( 'NONE', ( #17479, #13521, #5971, #6145 ) ) ;
#28669 = DIRECTION ( 'NONE',  ( 0.000000000000000000, 0.000000000000000000, 1.000000000000000000 ) ) ;
#28670 = ADVANCED_FACE ( 'NONE', ( #11801 ), #17371, .T. ) ;
#28671 = DIRECTION ( 'NONE',  ( 0.000000000000000000, 0.000000000000000000, 1.000000000000000000 ) ) ;
#28672 = ORIENTED_EDGE ( 'NONE', *, *, #19792, .T. ) ;
#28673 = ORIENTED_EDGE ( 'NONE', *, *, #857, .F. ) ;
#28674 = CARTESIAN_POINT ( 'NONE',  ( -34.50000000000000000, -113.6974040292745656, 2.970979214817929481 ) ) ;
#28675 = CARTESIAN_POINT ( 'NONE',  ( -35.50000000000000711, -112.9415908020655195, 1.873661708251232572 ) ) ;
#28676 = VERTEX_POINT ( 'NONE', #22960 ) ;
#28677 = VERTEX_POINT ( 'NONE', #3905 ) ;
#28678 = EDGE_CURVE ( 'NONE', #19248, #34240, #26034, .T. ) ;
#28679 = DIRECTION ( 'NONE',  ( 0.000000000000000000, 0.000000000000000000, 1.000000000000000000 ) ) ;
#28680 = CIRCLE ( 'NONE', #25230, 20.00000000000000711 ) ;
#28681 = VECTOR ( 'NONE', #15358, 1000.000000000000000 ) ;
#28682 = CARTESIAN_POINT ( 'NONE',  ( -37.54084996655477369, -113.9929510916434339, 13.11692036158760466 ) ) ;
#28683 = FACE_OUTER_BOUND ( 'NONE', #9315, .T. ) ;
#28684 = CARTESIAN_POINT ( 'NONE',  ( -35.93473953453761993, -113.9929510916434339, 13.11451721564123396 ) ) ;
#28685 = ADVANCED_FACE ( 'NONE', ( #1366 ), #20605, .T. ) ;
#28686 = CARTESIAN_POINT ( 'NONE',  ( -35.50000000000000000, -115.6492853190479337, 9.359470924297957239 ) ) ;
#28687 = UNCERTAINTY_MEASURE_WITH_UNIT (LENGTH_MEASURE( 1.000000000000000082E-05 ), #10148, 'distance_accuracy_value', 'NONE');
#28688 = LINE ( 'NONE', #31905, #27372 ) ;
#28689 = DIRECTION ( 'NONE',  ( -1.000000000000000000, -0.000000000000000000, -0.000000000000000000 ) ) ;
#28690 = EDGE_CURVE ( 'NONE', #26850, #18961, #13639, .T. ) ;
#28691 = CYLINDRICAL_SURFACE ( 'NONE', #6199, 17.49900000000000233 ) ;
#28692 = CYLINDRICAL_SURFACE ( 'NONE', #32951, 3.799999999999999822 ) ;
#28693 = FACE_OUTER_BOUND ( 'NONE', #26582, .T. ) ;
#28694 = ORIENTED_EDGE ( 'NONE', *, *, #12975, .T. ) ;
#28695 = FACE_OUTER_BOUND ( 'NONE', #28668, .T. ) ;
#28696 = CARTESIAN_POINT ( 'NONE',  ( -35.50000000000000711, -112.9415908020655195, 1.873661708251232572 ) ) ;
#28697 = CARTESIAN_POINT ( 'NONE',  ( 8.000000000000000000, -15.46619997295641369, -1.007799283846847471 ) ) ;
#28698 = EDGE_CURVE ( 'NONE', #10424, #24324, #17628, .T. ) ;
#28699 = CONTEXT_DEPENDENT_SHAPE_REPRESENTATION ( #5100, #6629 ) ;
#28700 = EDGE_CURVE ( 'NONE', #18020, #30594, #9599, .T. ) ;
#28701 = CARTESIAN_POINT ( 'NONE',  ( 8.000000000000000000, 21.63912866391140000, 3.968388925834891001 ) ) ;
#28702 = CARTESIAN_POINT ( 'NONE',  ( 0.000000000000000000, -5.679790370315976666, -7.613867765417642097 ) ) ;
#28703 = VERTEX_POINT ( 'NONE', #17194 ) ;
#28704 = VECTOR ( 'NONE', #30835, 1000.000000000000000 ) ;
#28705 = DIRECTION ( 'NONE',  ( -1.000000000000000000, 0.000000000000000000, 0.000000000000000000 ) ) ;
#28706 = CARTESIAN_POINT ( 'NONE',  ( -34.50000000000000000, -112.9650106922503170, -2.624765990393421955 ) ) ;
#28707 = CARTESIAN_POINT ( 'NONE',  ( 0.000000000000000000, -11.27190672109260028, -0.3151488735048807444 ) ) ;
#28708 = ORIENTED_EDGE ( 'NONE', *, *, #3953, .T. ) ;
#28709 = ORIENTED_EDGE ( 'NONE', *, *, #31047, .T. ) ;
#28710 = CARTESIAN_POINT ( 'NONE',  ( -35.97545270896702618, -113.6450488405582604, 2.909774454178449155 ) ) ;
#28711 = VERTEX_POINT ( 'NONE', #25684 ) ;
#28712 = VERTEX_POINT ( 'NONE', #9287 ) ;
#28713 = EDGE_LOOP ( 'NONE', ( #12413, #10151, #35206, #8313 ) ) ;
#28714 = CARTESIAN_POINT ( 'NONE',  ( -34.50000000000000000, -113.2441867727860227, 0.9026824934337903672 ) ) ;
#28715 = DIRECTION ( 'NONE',  ( -1.000000000000000000, 0.000000000000000000, 0.000000000000000000 ) ) ;
#28716 = DIRECTION ( 'NONE',  ( 0.000000000000000000, 0.000000000000000000, 1.000000000000000000 ) ) ;
#28717 = CARTESIAN_POINT ( 'NONE',  ( -35.74814306589956914, -114.9929510916434339, 13.05539834812772781 ) ) ;
#28718 = LINE ( 'NONE', #26375, #16104 ) ;
#28719 = AXIS2_PLACEMENT_3D ( 'NONE', #16653, #14476, #11442 ) ;
#28720 = CARTESIAN_POINT ( 'NONE',  ( -34.49999999999998579, -28.31857036507959791, 80.03062855292519373 ) ) ;
#28721 = EDGE_CURVE ( 'NONE', #31502, #23346, #33728, .T. ) ;
#28722 = CARTESIAN_POINT ( 'NONE',  ( -37.34375000000001421, -114.9929510916434339, 14.11852480586264846 ) ) ;
#28723 = DIRECTION ( 'NONE',  ( -1.000000000000000000, 0.000000000000000000, 0.000000000000000000 ) ) ;
#28724 = AXIS2_PLACEMENT_3D ( 'NONE', #21750, #18880, #34745 ) ;
#28725 = EDGE_CURVE ( 'NONE', #9377, #25123, #21071, .T. ) ;
#28726 = DIRECTION ( 'NONE',  ( 1.000000000000000000, -1.110223024625156540E-16, 0.000000000000000000 ) ) ;
#28727 = ORIENTED_EDGE ( 'NONE', *, *, #30275, .F. ) ;
#28728 = CIRCLE ( 'NONE', #8008, 20.00000000000000711 ) ;
#28729 = AXIS2_PLACEMENT_3D ( 'NONE', #23567, #14914, #25923 ) ;
#28730 = CARTESIAN_POINT ( 'NONE',  ( -35.50000000000000000, -115.9895221797699065, 10.38535157366622563 ) ) ;
#28731 = CARTESIAN_POINT ( 'NONE',  ( -35.50000000000000711, -116.0140978167138712, -0.4685323525984310677 ) ) ;
#28732 = AXIS2_PLACEMENT_3D ( 'NONE', #15272, #31508, #21031 ) ;
#28733 = CYLINDRICAL_SURFACE ( 'NONE', #16949, 7.199999999999994849 ) ;
#28734 = CARTESIAN_POINT ( 'NONE',  ( 0.000000000000000000, -6.085920226790910270, -15.78165944574524637 ) ) ;
#28735 = CYLINDRICAL_SURFACE ( 'NONE', #21081, 8.000000000000000000 ) ;
#28736 = CARTESIAN_POINT ( 'NONE',  ( 8.000000000000000000, 0.000000000000000000, 0.000000000000000000 ) ) ;
#28737 = CARTESIAN_POINT ( 'NONE',  ( 7.999999999999992895, -47.00885577955417460, 6.806061952192132836 ) ) ;
#28738 = DIRECTION ( 'NONE',  ( 0.000000000000000000, 0.000000000000000000, 1.000000000000000000 ) ) ;
#28739 = VERTEX_POINT ( 'NONE', #23317 ) ;
#28740 = CARTESIAN_POINT ( 'NONE',  ( -35.99999999999999289, -113.9407375970686758, 6.996475545821551734 ) ) ;
#28741 = FACE_OUTER_BOUND ( 'NONE', #34323, .T. ) ;
#28742 = CARTESIAN_POINT ( 'NONE',  ( 3.799999999999999822, 0.000000000000000000, -40.89999999999999858 ) ) ;
#28743 = ORIENTED_EDGE ( 'NONE', *, *, #10165, .T. ) ;
#28744 = VERTEX_POINT ( 'NONE', #33782 ) ;
#28745 = CARTESIAN_POINT ( 'NONE',  ( 5.400000000000003020, 1.000000000000000888, 30.00000000000000000 ) ) ;
#28746 = ORIENTED_EDGE ( 'NONE', *, *, #3954, .F. ) ;
#28747 = CARTESIAN_POINT ( 'NONE',  ( -35.69809690994941320, -116.9754527089670546, 5.777725545821551734 ) ) ;
#28748 = VERTEX_POINT ( 'NONE', #28202 ) ;
#28749 = DIRECTION ( 'NONE',  ( 0.000000000000000000, 0.000000000000000000, -1.000000000000000000 ) ) ;
#28750 = AXIS2_PLACEMENT_3D ( 'NONE', #16171, #14014, #8437 ) ;
#28751 = DIRECTION ( 'NONE',  ( 0.000000000000000000, 0.000000000000000000, 1.000000000000000000 ) ) ;
#28752 = CARTESIAN_POINT ( 'NONE',  ( -1.799999999999995604, -2.775557561562891351E-16, -4.000000000000014211 ) ) ;
#28753 = AXIS2_PLACEMENT_3D ( 'NONE', #28760, #23897, #1218 ) ;
#28754 = AXIS2_PLACEMENT_3D ( 'NONE', #30744, #5735, #22620 ) ;
#28755 = PRODUCT_CONTEXT ( 'NONE', #2522, 'mechanical' ) ;
#28756 = DIRECTION ( 'NONE',  ( -1.000000000000000000, 0.000000000000000000, 0.000000000000000000 ) ) ;
#28757 = EDGE_LOOP ( 'NONE', ( #3975, #5252, #18148, #35331, #29744, #14250, #10282, #31220, #29888, #27739, #17393, #20516, #19291, #5236, #27173, #7525, #18199, #31825, #30339, #7788, #18678, #32556, #14098, #25875, #11949 ) ) ;
#28758 = VERTEX_POINT ( 'NONE', #31605 ) ;
#28759 = CARTESIAN_POINT ( 'NONE',  ( 0.000000000000000000, 0.000000000000000000, -0.7999999999999951594 ) ) ;
#28760 = CARTESIAN_POINT ( 'NONE',  ( 8.000000000000000000, -16.53603053422202862, -8.931325931664767737 ) ) ;
#28761 = ORIENTED_EDGE ( 'NONE', *, *, #32189, .F. ) ;
#28762 = DIRECTION ( 'NONE',  ( -5.339440136655842133E-16, -1.000000000000000000, 6.938893903907197563E-17 ) ) ;
#28763 = CARTESIAN_POINT ( 'NONE',  ( -34.50000000000000000, -113.1807644833805426, -0.6247823525984269599 ) ) ;
#28764 = DIRECTION ( 'NONE',  ( 0.000000000000000000, 0.000000000000000000, 1.000000000000000000 ) ) ;
#28765 = CYLINDRICAL_SURFACE ( 'NONE', #28821, 20.00000000000000711 ) ;
#28766 = EDGE_CURVE ( 'NONE', #4943, #16000, #3542, .T. ) ;
#28767 = CARTESIAN_POINT ( 'NONE',  ( -37.37500000000009237, -115.9929510916434481, 14.11852480586265024 ) ) ;
#28768 = DIRECTION ( 'NONE',  ( 0.000000000000000000, 0.000000000000000000, 1.000000000000000000 ) ) ;
#28769 = DIRECTION ( 'NONE',  ( 0.000000000000000000, 0.000000000000000000, 1.000000000000000000 ) ) ;
#28770 = CARTESIAN_POINT ( 'NONE',  ( -39.00000000000000711, -114.9929510916434339, 12.39849696637031151 ) ) ;
#28771 = PLANE ( 'NONE',  #29163 ) ;
#28772 = CARTESIAN_POINT ( 'NONE',  ( 4.000000000000000000, 4.898587196589412829E-16, 65.00000000000000000 ) ) ;
#28773 = AXIS2_PLACEMENT_3D ( 'NONE', #8215, #13805, #13287 ) ;
#28774 = FACE_OUTER_BOUND ( 'NONE', #6256, .T. ) ;
#28775 = CARTESIAN_POINT ( 'NONE',  ( 27.00000000000001776, -44.99999999999997868, 0.000000000000000000 ) ) ;
#28776 = DIRECTION ( 'NONE',  ( 0.000000000000000000, 0.000000000000000000, 1.000000000000000000 ) ) ;
#28777 = ORIENTED_EDGE ( 'NONE', *, *, #30419, .T. ) ;
#28778 = EDGE_CURVE ( 'NONE', #1301, #17170, #15906, .T. ) ;
#28779 = AXIS2_PLACEMENT_3D ( 'NONE', #13777, #5496, #8179 ) ;
#28780 = CIRCLE ( 'NONE', #17841, 7.199999999999993960 ) ;
#28781 = CARTESIAN_POINT ( 'NONE',  ( -38.30190309005061522, -111.0245472910330022, 6.527725545821552622 ) ) ;
#28782 = FACE_BOUND ( 'NONE', #25251, .T. ) ;
#28783 = CARTESIAN_POINT ( 'NONE',  ( -35.50000000000000000, -113.0140978167137717, -0.6411448143358797758 ) ) ;
#28784 = VERTEX_POINT ( 'NONE', #9110 ) ;
#28785 = ORIENTED_EDGE ( 'NONE', *, *, #35124, .F. ) ;
#28787 = CARTESIAN_POINT ( 'NONE',  ( 4.000000000000000000, 4.898587196589412829E-16, 49.10000000000000142 ) ) ;
#28786 = PRODUCT ( 'circlip for shafts normal_din_Circlip DIN 471 - 22 x 1.2', 'circlip for shafts normal_din_Circlip DIN 471 - 22 x 1.2', '', ( #11306 ) ) ;
#28788 = FACE_OUTER_BOUND ( 'NONE', #11125, .T. ) ;
#28789 = ORIENTED_EDGE ( 'NONE', *, *, #26959, .T. ) ;
#28790 = ORIENTED_EDGE ( 'NONE', *, *, #21844, .F. ) ;
#28791 = EDGE_LOOP ( 'NONE', ( #22888, #31026, #11586, #26010 ) ) ;
#28792 = DIRECTION ( 'NONE',  ( 1.000000000000000000, 0.000000000000000000, -1.691777834109591283E-31 ) ) ;
#28793 = CARTESIAN_POINT ( 'NONE',  ( -37.76916472181486739, -116.0245472910329880, 4.465225545821550845 ) ) ;
#28794 = AXIS2_PLACEMENT_3D ( 'NONE', #19828, #5825, #16958 ) ;
#28795 =( NAMED_UNIT ( * ) PLANE_ANGLE_UNIT ( ) SI_UNIT ( $, .RADIAN. ) );
#28796 = CYLINDRICAL_SURFACE ( 'NONE', #16162, 20.00000000000000355 ) ;
#28797 = ORIENTED_EDGE ( 'NONE', *, *, #3592, .T. ) ;
#28798 = VERTEX_POINT ( 'NONE', #643 ) ;
#28799 = CARTESIAN_POINT ( 'NONE',  ( -35.50000000000000000, -114.9307644833806137, -2.624782352598442614 ) ) ;
#28800 = DIRECTION ( 'NONE',  ( -1.000000000000000000, 0.000000000000000000, 0.000000000000000000 ) ) ;
#28801 = CARTESIAN_POINT ( 'NONE',  ( 0.000000000000000000, 0.000000000000000000, 35.10000000000000142 ) ) ;
#28802 = CIRCLE ( 'NONE', #7517, 6.000000000000005329 ) ;
#28803 = AXIS2_PLACEMENT_3D ( 'NONE', #7132, #6778, #20619 ) ;
#28804 = ORIENTED_EDGE ( 'NONE', *, *, #20768, .T. ) ;
#28805 = CARTESIAN_POINT ( 'NONE',  ( -37.99359134332094357, -114.9929510916434339, 12.69998175888958158 ) ) ;
#28806 = EDGE_CURVE ( 'NONE', #13985, #33840, #15030, .T. ) ;
#28807 = CARTESIAN_POINT ( 'NONE',  ( -34.50000000000000000, -114.1264797827112574, 9.515205387299289441 ) ) ;
#28808 = EDGE_CURVE ( 'NONE', #3685, #15482, #24567, .T. ) ;
#28809 = DIRECTION ( 'NONE',  ( -1.000000000000000000, 0.000000000000000000, 0.000000000000000000 ) ) ;
#28810 = CARTESIAN_POINT ( 'NONE',  ( -4.000000000000000000, -2.710505431213761085E-17, 30.00000000000000000 ) ) ;
#28811 = CARTESIAN_POINT ( 'NONE',  ( -38.25557080230232998, -113.9929510916434339, 13.92914543265419525 ) ) ;
#28812 = DIRECTION ( 'NONE',  ( 0.000000000000000000, 0.000000000000000000, 1.000000000000000000 ) ) ;
#28813 = CARTESIAN_POINT ( 'NONE',  ( -35.50000000000000711, -114.9929510916434339, 12.60752341388803544 ) ) ;
#28814 = FACE_OUTER_BOUND ( 'NONE', #30041, .T. ) ;
#28815 = ORIENTED_EDGE ( 'NONE', *, *, #19406, .F. ) ;
#28816 = DIRECTION ( 'NONE',  ( -1.000000000000000000, 0.000000000000000000, 0.000000000000000000 ) ) ;
#28817 = DIRECTION ( 'NONE',  ( -1.000000000000000000, 0.000000000000000000, -0.000000000000000000 ) ) ;
#28818 = ORIENTED_EDGE ( 'NONE', *, *, #14298, .F. ) ;
#28819 = CARTESIAN_POINT ( 'NONE',  ( -35.50005019975638021, -114.9929510916434339, 12.62670525340498529 ) ) ;
#28820 = VERTEX_POINT ( 'NONE', #14859 ) ;
#28821 = AXIS2_PLACEMENT_3D ( 'NONE', #9844, #7501, #15763 ) ;
#28822 = EDGE_CURVE ( 'NONE', #22338, #1992, #19924, .T. ) ;
#28823 = DIRECTION ( 'NONE',  ( 0.000000000000000000, 0.000000000000000000, -1.000000000000000000 ) ) ;
#28824 = VERTEX_POINT ( 'NONE', #3375 ) ;
#28825 = DIRECTION ( 'NONE',  ( -1.000000000000000000, 0.000000000000000000, 0.000000000000000000 ) ) ;
#28826 = ORIENTED_EDGE ( 'NONE', *, *, #9702, .T. ) ;
#28827 = CARTESIAN_POINT ( 'NONE',  ( -34.50000000000000000, -113.0140978167138712, 0.6252176474015680441 ) ) ;
#28828 = DIRECTION ( 'NONE',  ( -1.000000000000000000, 0.000000000000000000, 0.000000000000000000 ) ) ;
#28829 = CARTESIAN_POINT ( 'NONE',  ( -35.00000000000000000, -114.0592624029313242, 7.503524454178449155 ) ) ;
#28830 = COLOUR_RGB ( '', 0.66274510, 0.83137255, 0.94901961) ;
#28831 = ORIENTED_EDGE ( 'NONE', *, *, #7774, .T. ) ;
#28832 = AXIS2_PLACEMENT_3D ( 'NONE', #4685, #35451, #7703 ) ;
#28833 = CARTESIAN_POINT ( 'NONE',  ( -37.05926240293131713, -115.9999999999999858, 6.378524454178448266 ) ) ;
#28834 = FACE_BOUND ( 'NONE', #31868, .T. ) ;
#28835 = CARTESIAN_POINT ( 'NONE',  ( -35.50000000000000711, -112.0140978167138712, 0.0002176474015661141945 ) ) ;
#28836 = VERTEX_POINT ( 'NONE', #7115 ) ;
#28837 = ORIENTED_EDGE ( 'NONE', *, *, #33117, .T. ) ;
#28838 = CARTESIAN_POINT ( 'NONE',  ( 4.000000000000000000, 4.627536653468036720E-16, 55.00000000000000000 ) ) ;
#28839 = EDGE_CURVE ( 'NONE', #8462, #10099, #20960, .T. ) ;
#28840 = CARTESIAN_POINT ( 'NONE',  ( -34.49999999999998579, -34.23950567274729195, 73.69543654875865002 ) ) ;
#28841 = ORIENTED_EDGE ( 'NONE', *, *, #32345, .F. ) ;
#28842 = VERTEX_POINT ( 'NONE', #31960 ) ;
#28843 = CARTESIAN_POINT ( 'NONE',  ( -34.50000000000000000, -116.0140978167138712, 0.0002176474015577116276 ) ) ;
#28844 = CARTESIAN_POINT ( 'NONE',  ( -35.50000000000000711, -113.0106174888879877, 1.881901162060937827 ) ) ;
#28845 = AXIS2_PLACEMENT_3D ( 'NONE', #32520, #10928, #16297 ) ;
#28846 = ORIENTED_EDGE ( 'NONE', *, *, #29189, .T. ) ;
#28847 = ORIENTED_EDGE ( 'NONE', *, *, #31496, .F. ) ;
#28848 = DIRECTION ( 'NONE',  ( -0.000000000000000000, 0.000000000000000000, -1.000000000000000000 ) ) ;
#28849 = EDGE_CURVE ( 'NONE', #8462, #32097, #33757, .T. ) ;
#28850 = CARTESIAN_POINT ( 'NONE',  ( -36.03125000000003553, -113.9929510916434339, 13.11852480586264846 ) ) ;
#28851 = EDGE_CURVE ( 'NONE', #32250, #35186, #31446, .T. ) ;
#28852 = DIRECTION ( 'NONE',  ( -1.000000000000000000, 0.000000000000000000, 0.000000000000000000 ) ) ;
#28853 = EDGE_CURVE ( 'NONE', #19590, #1645, #21494, .T. ) ;
#28854 = AXIS2_PLACEMENT_3D ( 'NONE', #23803, #29571, #7583 ) ;
#28855 = CARTESIAN_POINT ( 'NONE',  ( -36.50000000000010658, -113.9929510916434339, 13.11852480586264846 ) ) ;
#28856 = CARTESIAN_POINT ( 'NONE',  ( -35.52552712174883709, -115.9929510916434481, 12.77960891308624625 ) ) ;
#28857 = CARTESIAN_POINT ( 'NONE',  ( 4.000000000000003553, -49.25004636492401033, 16.68630974939741662 ) ) ;
#28858 = CARTESIAN_POINT ( 'NONE',  ( 8.000000000000000000, -16.71027810728550733, -2.620268201066114688 ) ) ;
#28859 = ORIENTED_EDGE ( 'NONE', *, *, #30365, .F. ) ;
#28860 = EDGE_CURVE ( 'NONE', #28739, #29834, #29173, .T. ) ;
#28861 = CARTESIAN_POINT ( 'NONE',  ( 7.999999999999992895, 9.714451465470119729E-14, 1.000000000000000888 ) ) ;
#28862 = DIRECTION ( 'NONE',  ( -1.783119874454246424E-31, -1.187911941725854497E-31, 1.000000000000000000 ) ) ;
#28863 = CARTESIAN_POINT ( 'NONE',  ( -42.49999999999999289, -31.64142946139395107, 72.19543654875866423 ) ) ;
#28864 = EDGE_CURVE ( 'NONE', #14196, #4114, #7297, .T. ) ;
#28865 = EDGE_LOOP ( 'NONE', ( #1478, #32875, #19662, #31612 ) ) ;
#28866 = STYLED_ITEM ( 'NONE', ( #13678 ), #22543 ) ;
#28867 = CYLINDRICAL_SURFACE ( 'NONE', #3232, 4.999999999999997335 ) ;
#28868 = CARTESIAN_POINT ( 'NONE',  ( -35.50000000000000711, -112.0141059978162019, -0.6575071456984691309 ) ) ;
#28869 = CARTESIAN_POINT ( 'NONE',  ( 0.000000000000000000, 46.90537658765329354, 2.727856614654466938 ) ) ;
#28870 = ITEM_DEFINED_TRANSFORMATION ( 'NONE', 'NONE', #31596,  #21307 ) ;
#28871 = DIRECTION ( 'NONE',  ( -1.000000000000000000, 0.000000000000000000, 0.000000000000000000 ) ) ;
#28872 = DIRECTION ( 'NONE',  ( -1.000000000000000000, 0.000000000000000000, 0.000000000000000000 ) ) ;
#28873 = ORIENTED_EDGE ( 'NONE', *, *, #11732, .F. ) ;
#28874 = DIRECTION ( 'NONE',  ( 1.000000000000000000, 0.000000000000000000, 0.000000000000000000 ) ) ;
#28875 = CARTESIAN_POINT ( 'NONE',  ( -34.50000000000000000, -115.5324766040685631, -2.560864217809699195 ) ) ;
#28876 = CYLINDRICAL_SURFACE ( 'NONE', #32994, 4.000000000000003553 ) ;
#28877 = ORIENTED_EDGE ( 'NONE', *, *, #7142, .T. ) ;
#28878 = ORIENTED_EDGE ( 'NONE', *, *, #34922, .F. ) ;
#28879 = CARTESIAN_POINT ( 'NONE',  ( -37.47347596530441649, -113.0245472910329880, 9.527725545821551734 ) ) ;
#28880 = ORIENTED_EDGE ( 'NONE', *, *, #8563, .F. ) ;
#28881 = CIRCLE ( 'NONE', #11077, 4.000000000000000000 ) ;
#28882 = TOROIDAL_SURFACE ( 'NONE', #13920, 4.200000000000000178, 0.1999999999999998723 ) ;
#28883 = EDGE_CURVE ( 'NONE', #2676, #17256, #35498, .T. ) ;
#28884 = VERTEX_POINT ( 'NONE', #15198 ) ;
#28885 = VERTEX_POINT ( 'NONE', #35047 ) ;
#28886 = CARTESIAN_POINT ( 'NONE',  ( -35.50000000000000000, -114.8474311500471572, -0.6247823525984269599 ) ) ;
#28887 = EDGE_CURVE ( 'NONE', #5884, #8628, #5015, .T. ) ;
#28888 = ADVANCED_FACE ( 'NONE', ( #4622 ), #15556, .T. ) ;
#28889 = FACE_OUTER_BOUND ( 'NONE', #12259, .T. ) ;
#28890 = DIRECTION ( 'NONE',  ( 0.000000000000000000, 0.000000000000000000, 1.000000000000000000 ) ) ;
#28891 = CARTESIAN_POINT ( 'NONE',  ( -35.50000000000000711, -114.9929510916434339, 12.57451923796416082 ) ) ;
#28892 = DIRECTION ( 'NONE',  ( -1.000000000000000000, 0.000000000000000000, 0.000000000000000000 ) ) ;
#28893 = EDGE_CURVE ( 'NONE', #32097, #14060, #34911, .T. ) ;
#28894 = EDGE_CURVE ( 'NONE', #19681, #17706, #4439, .T. ) ;
#28895 = CARTESIAN_POINT ( 'NONE',  ( -37.52454134262690388, -114.9929510916434339, 14.11837420659362152 ) ) ;
#28896 = DIRECTION ( 'NONE',  ( 0.000000000000000000, 0.000000000000000000, 1.000000000000000000 ) ) ;
#28897 = CIRCLE ( 'NONE', #34643, 3.799999999999999822 ) ;
#28898 = LINE ( 'NONE', #34125, #18614 ) ;
#28899 = VERTEX_POINT ( 'NONE', #23684 ) ;
#28900 = VECTOR ( 'NONE', #29286, 1000.000000000000000 ) ;
#28901 = CARTESIAN_POINT ( 'NONE',  ( -35.50000000000000000, -115.9929510916434481, 11.38636890470581164 ) ) ;
#28903 = CARTESIAN_POINT ( 'NONE',  ( -35.50000000000000711, -113.8474311500459777, -1.624782352598427959 ) ) ;
#28902 = AXIS2_PLACEMENT_3D ( 'NONE', #13571, #32835, #2794 ) ;
#28904 = FILL_AREA_STYLE_COLOUR ( '', #3077 ) ;
#28905 = DIRECTION ( 'NONE',  ( 0.000000000000000000, 0.000000000000000000, -1.000000000000000000 ) ) ;
#28906 = FACE_OUTER_BOUND ( 'NONE', #20755, .T. ) ;
#28907 = ADVANCED_FACE ( 'NONE', ( #26755, #35215 ), #21150, .T. ) ;
#28908 = LINE ( 'NONE', #2096, #18214 ) ;
#28909 = DIRECTION ( 'NONE',  ( 0.000000000000000000, 0.000000000000000000, 1.000000000000000000 ) ) ;
#28910 = DIRECTION ( 'NONE',  ( -1.000000000000000000, 0.000000000000000000, 0.000000000000000000 ) ) ;
#28911 = CARTESIAN_POINT ( 'NONE',  ( 0.000000000000000000, 3.872983346207531596, 1.000000000000000888 ) ) ;
#28912 = ORIENTED_EDGE ( 'NONE', *, *, #14127, .T. ) ;
#28913 = CARTESIAN_POINT ( 'NONE',  ( -35.97545270896705460, -114.3549511594417680, 5.590225545821552622 ) ) ;
#28914 = DIRECTION ( 'NONE',  ( 0.000000000000000000, 0.000000000000000000, 1.000000000000000000 ) ) ;
#28915 = LINE ( 'NONE', #3722, #29681 ) ;
#28916 = EDGE_LOOP ( 'NONE', ( #10919, #21289, #25647, #19648 ) ) ;
#28917 = AXIS2_PLACEMENT_3D ( 'NONE', #26532, #4751, #6711 ) ;
#28918 = ORIENTED_EDGE ( 'NONE', *, *, #14550, .T. ) ;
#28919 = CIRCLE ( 'NONE', #23149, 20.00000000000000355 ) ;
#28920 = DIRECTION ( 'NONE',  ( 0.000000000000000000, -1.000000000000000000, 0.000000000000000000 ) ) ;
#28921 = DIRECTION ( 'NONE',  ( -0.000000000000000000, 0.000000000000000000, -1.000000000000000000 ) ) ;
#28922 = EDGE_LOOP ( 'NONE', ( #27323, #6424, #19929, #22005 ) ) ;
#28923 = CARTESIAN_POINT ( 'NONE',  ( -34.00000000000000000, -113.9407375970686758, 9.996475545821549957 ) ) ;
#28924 = VERTEX_POINT ( 'NONE', #32144 ) ;
#28925 = EDGE_CURVE ( 'NONE', #3630, #779, #26574, .T. ) ;
#28926 = DIRECTION ( 'NONE',  ( -1.000000000000000000, 0.000000000000000000, 0.000000000000000000 ) ) ;
#28927 = FACE_OUTER_BOUND ( 'NONE', #3598, .T. ) ;
#28928 = ADVANCED_FACE ( 'NONE', ( #7642 ), #7473, .T. ) ;
#28929 = AXIS2_PLACEMENT_3D ( 'NONE', #22204, #22734, #22554 ) ;
#28930 = AXIS2_PLACEMENT_3D ( 'NONE', #22330, #19964, #25044 ) ;
#28931 = DIRECTION ( 'NONE',  ( 1.000000000000000000, -0.000000000000000000, 0.000000000000000000 ) ) ;
#28932 = AXIS2_PLACEMENT_3D ( 'NONE', #28707, #25837, #25471 ) ;
#28933 = CARTESIAN_POINT ( 'NONE',  ( -10.00000000000000000, 0.000000000000000000, 19.99999999999998579 ) ) ;
#28934 = ORIENTED_EDGE ( 'NONE', *, *, #11463, .T. ) ;
#28935 = EDGE_LOOP ( 'NONE', ( #3915, #35383, #17263, #24420 ) ) ;
#28936 = DIRECTION ( 'NONE',  ( 0.000000000000000000, 0.9510565162951523099, 0.3090169943749513926 ) ) ;
#28937 = DIRECTION ( 'NONE',  ( -1.000000000000000000, 0.000000000000000000, 0.000000000000000000 ) ) ;
#28938 = ORIENTED_EDGE ( 'NONE', *, *, #18719, .T. ) ;
#28939 = DIRECTION ( 'NONE',  ( 0.000000000000000000, 0.000000000000000000, 1.000000000000000000 ) ) ;
#28940 = VECTOR ( 'NONE', #4518, 1000.000000000000000 ) ;
#28941 = FACE_OUTER_BOUND ( 'NONE', #1820, .T. ) ;
#28942 = DIRECTION ( 'NONE',  ( -1.000000000000000000, -0.000000000000000000, 0.000000000000000000 ) ) ;
#28943 = AXIS2_PLACEMENT_3D ( 'NONE', #5139, #32672, #24048 ) ;
#28944 = CARTESIAN_POINT ( 'NONE',  ( -35.07817881376918479, -115.9929510916434481, 13.81802396319203474 ) ) ;
#28945 = DIRECTION ( 'NONE',  ( 0.000000000000000000, 0.9929510916431029122, -0.1185248058626136303 ) ) ;
#28946 = CYLINDRICAL_SURFACE ( 'NONE', #9981, 3.799999999999999822 ) ;
#28947 = CARTESIAN_POINT ( 'NONE',  ( -34.57658136524561598, -115.9929510916434481, 13.10177712753338675 ) ) ;
#28948 = CARTESIAN_POINT ( 'NONE',  ( 3.799999999999999822, 0.000000000000000000, -32.00000000000000000 ) ) ;
#28949 = LINE ( 'NONE', #5003, #10964 ) ;
#28950 = CARTESIAN_POINT ( 'NONE',  ( 0.000000000000000000, 11.11653975335790179, 12.74840161668735661 ) ) ;
#28951 = DIRECTION ( 'NONE',  ( 0.000000000000000000, 0.000000000000000000, 1.000000000000000000 ) ) ;
#28952 = AXIS2_PLACEMENT_3D ( 'NONE', #559, #6317, #2935 ) ;
#28953 = VECTOR ( 'NONE', #6089, 1000.000000000000000 ) ;
#28954 = DIRECTION ( 'NONE',  ( 0.000000000000000000, 0.000000000000000000, 1.000000000000000000 ) ) ;
#28955 = DIRECTION ( 'NONE',  ( 0.000000000000000000, 0.3420201433256695456, -0.9396926207859079838 ) ) ;
#28956 = ORIENTED_EDGE ( 'NONE', *, *, #12062, .F. ) ;
#28957 = VECTOR ( 'NONE', #1695, 1000.000000000000000 ) ;
#28958 = CARTESIAN_POINT ( 'NONE',  ( -34.83677480945821259, -116.0794154965774965, 5.683975545821551734 ) ) ;
#28959 = DIRECTION ( 'NONE',  ( -1.000000000000000000, 0.000000000000000000, 0.000000000000000000 ) ) ;
#28960 = CARTESIAN_POINT ( 'NONE',  ( -35.50000000000000000, -113.0140978167138996, -0.6247823525984306237 ) ) ;
#28961 = ORIENTED_EDGE ( 'NONE', *, *, #12303, .T. ) ;
#28962 = ORIENTED_EDGE ( 'NONE', *, *, #12766, .F. ) ;
#28963 = CARTESIAN_POINT ( 'NONE',  ( 7.999999999999992895, 47.22458491092821475, 5.098390039074404356 ) ) ;
#28964 = CARTESIAN_POINT ( 'NONE',  ( 0.000000000000000000, 8.128228055638880178, 16.94522934049213347 ) ) ;
#28965 = ORIENTED_EDGE ( 'NONE', *, *, #2694, .T. ) ;
#28966 = ORIENTED_EDGE ( 'NONE', *, *, #27735, .T. ) ;
#28967 = VERTEX_POINT ( 'NONE', #18630 ) ;
#28968 = AXIS2_PLACEMENT_3D ( 'NONE', #18310, #20635, #10220 ) ;
#28969 = ADVANCED_FACE ( 'NONE', ( #23504 ), #4794, .F. ) ;
#28970 = CARTESIAN_POINT ( 'NONE',  ( 0.000000000000000000, -2.710505431213761085E-17, -45.00000000000000000 ) ) ;
#28971 = CARTESIAN_POINT ( 'NONE',  ( -37.88768952767750875, -112.0245472910329880, 3.527725545821551290 ) ) ;
#28972 = DIRECTION ( 'NONE',  ( 0.000000000000000000, 0.01157912003310095431, 0.9999329597424314597 ) ) ;
#28973 = FACE_OUTER_BOUND ( 'NONE', #30441, .T. ) ;
#28974 = ORIENTED_EDGE ( 'NONE', *, *, #29058, .F. ) ;
#28975 = ORIENTED_EDGE ( 'NONE', *, *, #5738, .F. ) ;
#28976 = CARTESIAN_POINT ( 'NONE',  ( -35.50000000000000000, -112.6882700046066645, -2.599147725882136939 ) ) ;
#28977 = CIRCLE ( 'NONE', #27831, 11.00000000000000000 ) ;
#28978 = AXIS2_PLACEMENT_3D ( 'NONE', #34487, #15727, #2085 ) ;
#28979 = DIRECTION ( 'NONE',  ( 0.000000000000000000, 0.000000000000000000, 1.000000000000000000 ) ) ;
#28980 = CARTESIAN_POINT ( 'NONE',  ( 7.999999999999992895, -29.60891106212763191, -37.14118181634798788 ) ) ;
#28981 = EDGE_LOOP ( 'NONE', ( #8739, #14429, #34919, #8125, #34777 ) ) ;
#28982 = CARTESIAN_POINT ( 'NONE',  ( -38.00000000000000711, -114.9929510916434339, 11.73841344789285657 ) ) ;
#28983 = CARTESIAN_POINT ( 'NONE',  ( -34.50000000000000000, -114.9929510916434339, 10.56126450660895699 ) ) ;
#28984 = DIRECTION ( 'NONE',  ( 0.000000000000000000, -1.000000000000000000, 0.000000000000000000 ) ) ;
#28985 = CARTESIAN_POINT ( 'NONE',  ( -36.24999999999983658, -114.9929510916434339, 13.11852480586264669 ) ) ;
#28986 = CYLINDRICAL_SURFACE ( 'NONE', #35270, 20.00000000000000355 ) ;
#28987 = CARTESIAN_POINT ( 'NONE',  ( -35.95093014754292682, -113.9929510916434339, 14.11777216781842625 ) ) ;
#28988 = CARTESIAN_POINT ( 'NONE',  ( 0.000000000000000000, 0.000000000000000000, -55.89999999999999858 ) ) ;
#28989 = LINE ( 'NONE', #1989, #26470 ) ;
#28990 = DIRECTION ( 'NONE',  ( -1.000000000000000000, 0.000000000000000000, 0.000000000000000000 ) ) ;
#28991 = ORIENTED_EDGE ( 'NONE', *, *, #35264, .T. ) ;
#28992 = DIRECTION ( 'NONE',  ( -1.226634733346697831E-16, -0.9659258262890664248, -0.2588190451025275673 ) ) ;
#28993 = CYLINDRICAL_SURFACE ( 'NONE', #19218, 2.999999999999988898 ) ;
#28994 = ORIENTED_EDGE ( 'NONE', *, *, #26909, .F. ) ;
#28995 = CARTESIAN_POINT ( 'NONE',  ( -35.50000000000000711, -114.9929510916434339, 11.91443571948719971 ) ) ;
#28996 = ORIENTED_EDGE ( 'NONE', *, *, #32341, .T. ) ;
#28997 = DIRECTION ( 'NONE',  ( -1.000000000000000000, 0.000000000000000000, 0.000000000000000000 ) ) ;
#28998 = ORIENTED_EDGE ( 'NONE', *, *, #12717, .T. ) ;
#28999 = DIRECTION ( 'NONE',  ( 0.000000000000000000, 0.000000000000000000, -1.000000000000000000 ) ) ;
#29000 = ORIENTED_EDGE ( 'NONE', *, *, #15574, .F. ) ;
#29001 = AXIS2_PLACEMENT_3D ( 'NONE', #17428, #15256, #12225 ) ;
#29002 = AXIS2_PLACEMENT_3D ( 'NONE', #26118, #26301, #1637 ) ;
#29003 = CARTESIAN_POINT ( 'NONE',  ( -34.50000000000000000, -113.0140978167139991, 0.8595926474015699315 ) ) ;
#29004 = CARTESIAN_POINT ( 'NONE',  ( -55.00000000000000000, 0.000000000000000000, 0.000000000000000000 ) ) ;
#29005 = DIRECTION ( 'NONE',  ( -1.000000000000000000, 0.000000000000000000, 0.000000000000000000 ) ) ;
#29006 = ORIENTED_EDGE ( 'NONE', *, *, #9713, .T. ) ;
#29007 = CARTESIAN_POINT ( 'NONE',  ( -37.76916472181487450, -111.9754527089670404, 7.034774454178450931 ) ) ;
#29008 = LINE ( 'NONE', #25961, #24552 ) ;
#29009 = ADVANCED_FACE ( 'NONE', ( #26206 ), #1544, .F. ) ;
#29010 = CARTESIAN_POINT ( 'NONE',  ( -35.50000000000000711, -116.0012805033554883, -0.7876962586524312027 ) ) ;
#29011 = ORIENTED_EDGE ( 'NONE', *, *, #35571, .F. ) ;
#29012 = ORIENTED_EDGE ( 'NONE', *, *, #30183, .T. ) ;
#29013 = EDGE_CURVE ( 'NONE', #26850, #33784, #16265, .T. ) ;
#29014 = DIRECTION ( 'NONE',  ( 0.000000000000000000, -1.000000000000000000, 0.000000000000000000 ) ) ;
#29015 =( NAMED_UNIT ( * ) SI_UNIT ( $, .STERADIAN. ) SOLID_ANGLE_UNIT ( ) );
#29016 = CARTESIAN_POINT ( 'NONE',  ( 4.000000000000003553, 13.61301047812928111, 3.268936481846215880 ) ) ;
#29017 = VERTEX_POINT ( 'NONE', #16452 ) ;
#29018 = VERTEX_POINT ( 'NONE', #32858 ) ;
#29019 = CARTESIAN_POINT ( 'NONE',  ( -34.50000000000000000, -113.1451905347060460, 2.905063584339864668 ) ) ;
#29020 = CARTESIAN_POINT ( 'NONE',  ( -35.50000000000000711, -113.6318576702834804, 1.956056246348823580 ) ) ;
#29021 = EDGE_CURVE ( 'NONE', #26745, #14077, #12481, .T. ) ;
#29022 = DIRECTION ( 'NONE',  ( 1.000000000000000000, 0.000000000000000000, 0.000000000000000000 ) ) ;
#29023 = ORIENTED_EDGE ( 'NONE', *, *, #698, .T. ) ;
#29024 = ORIENTED_EDGE ( 'NONE', *, *, #16723, .F. ) ;
#29025 = DIRECTION ( 'NONE',  ( 0.000000000000000000, 0.000000000000000000, -1.000000000000000000 ) ) ;
#29026 = EDGE_CURVE ( 'NONE', #1317, #8507, #30157, .T. ) ;
#29027 = CIRCLE ( 'NONE', #23842, 0.5000000000000004441 ) ;
#29028 = CARTESIAN_POINT ( 'NONE',  ( -38.00000000000000711, -113.9929510916434339, 12.26648026267477221 ) ) ;
#29029 = AXIS2_PLACEMENT_3D ( 'NONE', #23911, #21529, #26617 ) ;
#29030 = CARTESIAN_POINT ( 'NONE',  ( 0.000000000000000000, -10.46102064772325413, -19.35373470438994659 ) ) ;
#29031 = CARTESIAN_POINT ( 'NONE',  ( -35.50000000000000000, -113.9929510916434339, 10.94631322572069365 ) ) ;
#29032 = CIRCLE ( 'NONE', #28465, 4.000000000000000000 ) ;
#29033 = CARTESIAN_POINT ( 'NONE',  ( -35.74814306589956203, -115.9929510916434481, 13.05539834812772781 ) ) ;
#29034 = LINE ( 'NONE', #6525, #7816 ) ;
#29035 = DIRECTION ( 'NONE',  ( -1.000000000000000000, 0.000000000000000000, 0.000000000000000000 ) ) ;
#29036 = VERTEX_POINT ( 'NONE', #8178 ) ;
#29037 = LINE ( 'NONE', #28861, #34984 ) ;
#29038 = LINE ( 'NONE', #1865, #26614 ) ;
#29039 = DIRECTION ( 'NONE',  ( 1.000000000000000000, 0.000000000000000000, 0.000000000000000000 ) ) ;
#29040 = ADVANCED_FACE ( 'NONE', ( #22384 ), #5843, .T. ) ;
#29041 = AXIS2_PLACEMENT_3D ( 'NONE', #33905, #33722, #3671 ) ;
#29042 = ORIENTED_EDGE ( 'NONE', *, *, #16342, .F. ) ;
#29043 = CARTESIAN_POINT ( 'NONE',  ( 0.000000000000000000, 0.000000000000000000, 49.10000000000000142 ) ) ;
#29044 = CARTESIAN_POINT ( 'NONE',  ( -35.50000000000000711, -114.8057644833805568, -1.624782352598427959 ) ) ;
#29045 = CARTESIAN_POINT ( 'NONE',  ( 0.000000000000000000, -6.085920226791118992, 15.78165944574518775 ) ) ;
#29046 = CONTEXT_DEPENDENT_SHAPE_REPRESENTATION ( #9435, #24511 ) ;
#29047 = DIRECTION ( 'NONE',  ( -1.000000000000000000, -1.836970198721030181E-16, 0.000000000000000000 ) ) ;
#29048 = CARTESIAN_POINT ( 'NONE',  ( 8.000000000000000000, 5.482169781018835231, 16.00140663693125376 ) ) ;
#29049 = VERTEX_POINT ( 'NONE', #33212 ) ;
#29050 = CLOSED_SHELL ( 'NONE', ( #4692, #11099, #19041, #259, #25335, #9622, #80, #27722, #2331, #11877, #26481, #30453, #23727, #705, #31075, #33316 ) ) ;
#29051 = LINE ( 'NONE', #12854, #17607 ) ;
#29052 = ADVANCED_FACE ( 'NONE', ( #3151 ), #24584, .F. ) ;
#29053 = AXIS2_PLACEMENT_3D ( 'NONE', #9644, #6400, #26204 ) ;
#29054 = CARTESIAN_POINT ( 'NONE',  ( -35.50000000000000000, -113.2372261171341563, 2.916049522752222511 ) ) ;
#29055 = CYLINDRICAL_SURFACE ( 'NONE', #8813, 9.499000000000000554 ) ;
#29056 = VERTEX_POINT ( 'NONE', #86 ) ;
#29057 = ORIENTED_EDGE ( 'NONE', *, *, #28040, .F. ) ;
#29058 = EDGE_CURVE ( 'NONE', #11436, #28348, #995, .T. ) ;
#29059 = CARTESIAN_POINT ( 'NONE',  ( -37.47347596530441649, -114.9754527089670262, 4.972274454178449155 ) ) ;
#29060 = ADVANCED_FACE ( 'NONE', ( #8006 ), #27109, .T. ) ;
#29061 = CIRCLE ( 'NONE', #11795, 3.799999999999999822 ) ;
#29062 = VERTEX_POINT ( 'NONE', #19508 ) ;
#29063 = ORIENTED_EDGE ( 'NONE', *, *, #30371, .T. ) ;
#29064 = CARTESIAN_POINT ( 'NONE',  ( -35.50000000000000000, -115.0140978167138712, -0.4997823525984417259 ) ) ;
#29065 = AXIS2_PLACEMENT_3D ( 'NONE', #10688, #5123, #2254 ) ;
#29066 = EDGE_CURVE ( 'NONE', #29835, #30763, #18990, .T. ) ;
#29067 = DIRECTION ( 'NONE',  ( 1.112002228190253556E-16, -6.938893903907203726E-17, -1.000000000000000000 ) ) ;
#29068 = EDGE_CURVE ( 'NONE', #26887, #26849, #13091, .T. ) ;
#29069 = CARTESIAN_POINT ( 'NONE',  ( 0.000000000000000000, -5.363026430117185051, 9.919332006307207905 ) ) ;
#29070 = AXIS2_PLACEMENT_3D ( 'NONE', #1816, #1636, #31864 ) ;
#29071 = CARTESIAN_POINT ( 'NONE',  ( -35.50000000000000711, -114.9929510916434339, 10.55026311463432087 ) ) ;
#29072 = DIRECTION ( 'NONE',  ( -1.000000000000000000, 0.000000000000000000, 0.000000000000000000 ) ) ;
#29073 = CARTESIAN_POINT ( 'NONE',  ( -35.97545865737298953, -114.9929510916434339, 14.11837420659365705 ) ) ;
#29074 = CARTESIAN_POINT ( 'NONE',  ( 0.000000000000000000, 13.85708833599969303, 45.43276465116672114 ) ) ;
#29075 = PRODUCT ( 'circlip for shafts normal_din_Circlip DIN 471 - 8 x 0.8', 'circlip for shafts normal_din_Circlip DIN 471 - 8 x 0.8', '', ( #27863 ) ) ;
#29076 = CIRCLE ( 'NONE', #35411, 22.00000000000000000 ) ;
#29077 = CARTESIAN_POINT ( 'NONE',  ( 0.000000000000000000, 12.96676809804168862, -13.60411018104304048 ) ) ;
#29078 = EDGE_LOOP ( 'NONE', ( #11138, #2597, #21673, #34666 ) ) ;
#29079 = CARTESIAN_POINT ( 'NONE',  ( -35.91854304697312728, -115.9929510916434481, 13.11211614918345703 ) ) ;
#29080 = CARTESIAN_POINT ( 'NONE',  ( -35.50000000000000711, -116.0140978167138712, -0.4997823525984418369 ) ) ;
#29081 = CARTESIAN_POINT ( 'NONE',  ( -3.799999999999999822, 4.653657836759942730E-16, -44.50000000000000000 ) ) ;
#29082 = CARTESIAN_POINT ( 'NONE',  ( 0.000000000000000000, -2.710505431213761085E-17, -45.10000000000000142 ) ) ;
#29083 = AXIS2_PLACEMENT_3D ( 'NONE', #31020, #3140, #33540 ) ;
#29084 = EDGE_CURVE ( 'NONE', #34283, #13349, #19332, .T. ) ;
#29085 = AXIS2_PLACEMENT_3D ( 'NONE', #12127, #11424, #25466 ) ;
#29086 = PLANE ( 'NONE',  #17065 ) ;
#29087 = VERTEX_POINT ( 'NONE', #27283 ) ;
#29088 = CARTESIAN_POINT ( 'NONE',  ( 8.000000000000000000, -12.46108038583322930, 15.64357617738992801 ) ) ;
#29089 = DIRECTION ( 'NONE',  ( 0.000000000000000000, -8.881784197001252323E-16, 1.000000000000000000 ) ) ;
#29090 = ADVANCED_FACE ( 'NONE', ( #11241 ), #5153, .T. ) ;
#29091 = DIRECTION ( 'NONE',  ( -1.000000000000000000, 0.000000000000000000, 0.000000000000000000 ) ) ;
#29092 = CARTESIAN_POINT ( 'NONE',  ( 7.999999999999992895, 38.92705108641771261, -27.21837053747755419 ) ) ;
#29093 = VERTEX_POINT ( 'NONE', #5673 ) ;
#29094 = EDGE_CURVE ( 'NONE', #10066, #13424, #21865, .T. ) ;
#29095 = CARTESIAN_POINT ( 'NONE',  ( -36.64504884055823908, -115.0245472910329880, 6.284774454178449155 ) ) ;
#29096 = DIRECTION ( 'NONE',  ( -1.000000000000000000, 0.000000000000000000, 0.000000000000000000 ) ) ;
#29097 = DIRECTION ( 'NONE',  ( 0.000000000000000000, -0.8090169943749534465, 0.5877852522924650325 ) ) ;
#29098 = ORIENTED_EDGE ( 'NONE', *, *, #21194, .T. ) ;
#29099 = CIRCLE ( 'NONE', #11278, 52.00000000000000711 ) ;
#29100 = ORIENTED_EDGE ( 'NONE', *, *, #17253, .F. ) ;
#29101 = SURFACE_SIDE_STYLE ('',( #7306 ) ) ;
#29102 = DIRECTION ( 'NONE',  ( -1.000000000000000000, 0.000000000000000000, 0.000000000000000000 ) ) ;
#29103 = ORIENTED_EDGE ( 'NONE', *, *, #3137, .F. ) ;
#29104 = EDGE_CURVE ( 'NONE', #28558, #22834, #11352, .T. ) ;
#29105 = CARTESIAN_POINT ( 'NONE',  ( -34.00000000000000000, -113.9407375970686758, 8.496475545821549957 ) ) ;
#29106 = EDGE_CURVE ( 'NONE', #15493, #9389, #2983, .T. ) ;
#29107 = ORIENTED_EDGE ( 'NONE', *, *, #19792, .F. ) ;
#29108 = DIRECTION ( 'NONE',  ( -1.000000000000000000, 0.000000000000000000, 0.000000000000000000 ) ) ;
#29109 = ORIENTED_EDGE ( 'NONE', *, *, #20357, .T. ) ;
#29110 = DIRECTION ( 'NONE',  ( -1.000000000000000000, 0.000000000000000000, 0.000000000000000000 ) ) ;
#29111 = AXIS2_PLACEMENT_3D ( 'NONE', #32102, #15516, #12668 ) ;
#29112 = CARTESIAN_POINT ( 'NONE',  ( 8.000000000000007105, -9.433698091065020108, -1.111908866155191022 ) ) ;
#29113 = STYLED_ITEM ( 'NONE', ( #25768 ), #22248 ) ;
#29114 = AXIS2_PLACEMENT_3D ( 'NONE', #32186, #12750, #23912 ) ;
#29115 = EDGE_CURVE ( 'NONE', #12825, #22745, #33196, .T. ) ;
#29116 = DIRECTION ( 'NONE',  ( -1.000000000000000000, 0.000000000000000000, 0.000000000000000000 ) ) ;
#29117 = EDGE_LOOP ( 'NONE', ( #33332, #28831, #17821, #18248 ) ) ;
#29118 = ORIENTED_EDGE ( 'NONE', *, *, #25532, .T. ) ;
#29119 = AXIS2_PLACEMENT_3D ( 'NONE', #31786, #22965, #7120 ) ;
#29120 = CARTESIAN_POINT ( 'NONE',  ( -4.000000000000000000, 0.000000000000000000, 55.00000000000000000 ) ) ;
#29121 = DIRECTION ( 'NONE',  ( 0.000000000000000000, 0.000000000000000000, 1.000000000000000000 ) ) ;
#29122 = ORIENTED_EDGE ( 'NONE', *, *, #5407, .F. ) ;
#29123 = DIRECTION ( 'NONE',  ( -1.000000000000000000, -1.836970198721029934E-16, -0.000000000000000000 ) ) ;
#29124 = COLOUR_RGB ( '', 0.40784314, 0.44705882, 0.49803922) ;
#29125 = PLANE ( 'NONE',  #19944 ) ;
#29126 = CARTESIAN_POINT ( 'NONE',  ( 8.000000000000000000, 10.62435788049461571, -13.16139124467909483 ) ) ;
#29127 = CARTESIAN_POINT ( 'NONE',  ( -37.46093750000000711, -115.9929510916434481, 14.11852480586265024 ) ) ;
#29128 = CARTESIAN_POINT ( 'NONE',  ( 7.999999999999992895, -46.11014828289849277, 9.022736828080537563 ) ) ;
#29129 = CARTESIAN_POINT ( 'NONE',  ( -37.88768952767750164, -115.9754527089670262, 4.972274454178449155 ) ) ;
#29130 = CARTESIAN_POINT ( 'NONE',  ( -34.50015059926905536, -115.9929510916434481, 12.64306614848962518 ) ) ;
#29131 = CARTESIAN_POINT ( 'NONE',  ( 8.000000000000007105, -3.268936481846215880, 13.61301047812921183 ) ) ;
#29132 = EDGE_CURVE ( 'NONE', #6246, #26231, #16500, .T. ) ;
#29133 = DIRECTION ( 'NONE',  ( 0.000000000000000000, 0.5000000000000008882, -0.8660254037844382635 ) ) ;
#29134 = CIRCLE ( 'NONE', #14742, 22.00000000000000000 ) ;
#29135 = CARTESIAN_POINT ( 'NONE',  ( 7.999999999999992895, 11.46872990052381880, 45.56340405422447049 ) ) ;
#29136 = DIRECTION ( 'NONE',  ( -1.000000000000000000, 0.000000000000000000, 0.000000000000000000 ) ) ;
#29137 = EDGE_CURVE ( 'NONE', #13147, #14425, #17661, .T. ) ;
#29138 = EDGE_CURVE ( 'NONE', #32964, #35140, #25282, .T. ) ;
#29139 = CARTESIAN_POINT ( 'NONE',  ( -46.00000000000000000, -25.98076211353320275, 84.99999999999992895 ) ) ;
#29140 = CARTESIAN_POINT ( 'NONE',  ( -55.00000000000000000, 7.347880794884122694E-16, 76.00000000000001421 ) ) ;
#29141 = ORIENTED_EDGE ( 'NONE', *, *, #23228, .F. ) ;
#29142 = CARTESIAN_POINT ( 'NONE',  ( -39.02454729103295961, -113.2308352781851539, 4.840225545821551734 ) ) ;
#29143 =( GEOMETRIC_REPRESENTATION_CONTEXT ( 3 ) GLOBAL_UNCERTAINTY_ASSIGNED_CONTEXT ( ( #12514 ) ) GLOBAL_UNIT_ASSIGNED_CONTEXT ( ( #1096, #31519, #29185 ) ) REPRESENTATION_CONTEXT ( 'NONE', 'WORKASPACE' ) );
#29144 = LINE ( 'NONE', #23732, #5472 ) ;
#29145 = AXIS2_PLACEMENT_3D ( 'NONE', #4666, #29851, #18318 ) ;
#29146 = CARTESIAN_POINT ( 'NONE',  ( -35.50000000000000000, -113.1291422947505936, 0.8889500704178361357 ) ) ;
#29147 = EDGE_LOOP ( 'NONE', ( #26183, #14345 ) ) ;
#29148 = ORIENTED_EDGE ( 'NONE', *, *, #30171, .F. ) ;
#29149 = AXIS2_PLACEMENT_3D ( 'NONE', #10371, #13595, #13255 ) ;
#29150 = CARTESIAN_POINT ( 'NONE',  ( 50.00005079999999680, 3.872983346207416133, -1.000000000000000000 ) ) ;
#29151 = CARTESIAN_POINT ( 'NONE',  ( 0.000000000000000000, 34.03046037009304570, -33.13733193845769165 ) ) ;
#29152 = ORIENTED_EDGE ( 'NONE', *, *, #29480, .T. ) ;
#29153 = EDGE_CURVE ( 'NONE', #2022, #32250, #19950, .T. ) ;
#29154 = ORIENTED_EDGE ( 'NONE', *, *, #26628, .T. ) ;
#29155 = ADVANCED_FACE ( 'NONE', ( #12301 ), #14282, .T. ) ;
#29157 = ORIENTED_EDGE ( 'NONE', *, *, #35066, .T. ) ;
#29156 = AXIS2_PLACEMENT_3D ( 'NONE', #21464, #10141, #18417 ) ;
#29158 = AXIS2_PLACEMENT_3D ( 'NONE', #13773, #2981, #32485 ) ;
#29159 = CARTESIAN_POINT ( 'NONE',  ( 0.000000000000000000, -51.93417535146740960, -2.615612846549736581 ) ) ;
#29160 = CARTESIAN_POINT ( 'NONE',  ( 7.999999999999992895, -3.840921266750157326, 47.34345070675169609 ) ) ;
#29161 = CARTESIAN_POINT ( 'NONE',  ( -29.99999999999998579, -25.98076211353321696, 84.99999999999995737 ) ) ;
#29162 = DIRECTION ( 'NONE',  ( 0.000000000000000000, 0.000000000000000000, -1.000000000000000000 ) ) ;
#29163 = AXIS2_PLACEMENT_3D ( 'NONE', #9144, #680, #34002 ) ;
#29164 = ORIENTED_EDGE ( 'NONE', *, *, #14635, .T. ) ;
#29165 = EDGE_LOOP ( 'NONE', ( #3762, #27381, #11256, #20870 ) ) ;
#29166 = CARTESIAN_POINT ( 'NONE',  ( -35.50000000000000711, -112.0651520602111191, -0.9469505670458575608 ) ) ;
#29167 = VECTOR ( 'NONE', #2266, 1000.000000000000000 ) ;
#29168 = FACE_OUTER_BOUND ( 'NONE', #7757, .T. ) ;
#29169 = DIRECTION ( 'NONE',  ( 1.000000000000000000, 0.000000000000000000, 0.000000000000000000 ) ) ;
#29170 = VERTEX_POINT ( 'NONE', #25641 ) ;
#29171 = DIRECTION ( 'NONE',  ( 1.000000000000000000, 0.000000000000000000, 0.000000000000000000 ) ) ;
#29172 = AXIS2_PLACEMENT_3D ( 'NONE', #7144, #17940, #20271 ) ;
#29173 = CIRCLE ( 'NONE', #5575, 47.49900000000003075 ) ;
#29174 = CARTESIAN_POINT ( 'NONE',  ( 0.000000000000000000, -17.56975900509168298, -9.555290079479433984 ) ) ;
#29175 = CARTESIAN_POINT ( 'NONE',  ( -34.50000000000000000, -114.9929510916434339, 12.53051367006571581 ) ) ;
#29176 = AXIS2_PLACEMENT_3D ( 'NONE', #5320, #33031, #8344 ) ;
#29177 = CARTESIAN_POINT ( 'NONE',  ( 0.000000000000000000, 0.000000000000000000, 35.10000000000000142 ) ) ;
#29178 = CIRCLE ( 'NONE', #15294, 22.00000000000000000 ) ;
#29179 = CARTESIAN_POINT ( 'NONE',  ( -35.98364338251434447, -114.9929510916434339, 13.11827392651456314 ) ) ;
#29180 = CARTESIAN_POINT ( 'NONE',  ( 8.000000000000007105, -7.613867765417531075, 5.679790370316011305 ) ) ;
#29181 = CARTESIAN_POINT ( 'NONE',  ( -34.50000000000000000, -114.1861579685891712, 9.524983039397698192 ) ) ;
#29182 = DIRECTION ( 'NONE',  ( -1.000000000000000000, 0.000000000000000000, 0.000000000000000000 ) ) ;
#29183 = ADVANCED_FACE ( 'NONE', ( #33379 ), #8880, .T. ) ;
#29184 = CARTESIAN_POINT ( 'NONE',  ( -37.99899697755054717, -114.9929510916434339, 12.65121853911336736 ) ) ;
#29185 =( NAMED_UNIT ( * ) SI_UNIT ( $, .STERADIAN. ) SOLID_ANGLE_UNIT ( ) );
#29186 = EDGE_LOOP ( 'NONE', ( #4687, #12241, #14498, #29540 ) ) ;
#29187 = CARTESIAN_POINT ( 'NONE',  ( 0.000000000000000000, -6.860320204751044315, -13.89802171851389900 ) ) ;
#29188 = DIRECTION ( 'NONE',  ( -0.000000000000000000, 0.1736481776669234200, 0.9848077530122093526 ) ) ;
#29189 = EDGE_CURVE ( 'NONE', #30241, #20113, #14782, .T. ) ;
#29190 = ORIENTED_EDGE ( 'NONE', *, *, #11651, .T. ) ;
#29191 = CARTESIAN_POINT ( 'NONE',  ( -35.98364338251434447, -114.9929510916434339, 13.11827392651456314 ) ) ;
#29192 = ORIENTED_EDGE ( 'NONE', *, *, #14732, .F. ) ;
#29193 = LINE ( 'NONE', #17646, #4832 ) ;
#29194 = CARTESIAN_POINT ( 'NONE',  ( 3.799999999999999822, -2.710505431213761085E-17, -30.90000000000000568 ) ) ;
#29195 = CIRCLE ( 'NONE', #15927, 20.00000000000000711 ) ;
#29196 = ORIENTED_EDGE ( 'NONE', *, *, #5587, .F. ) ;
#29197 = DIRECTION ( 'NONE',  ( -1.000000000000000000, 0.000000000000000000, 0.000000000000000000 ) ) ;
#29198 = ORIENTED_EDGE ( 'NONE', *, *, #9242, .T. ) ;
#29199 = AXIS2_PLACEMENT_3D ( 'NONE', #16581, #5620, #25229 ) ;
#29200 = CARTESIAN_POINT ( 'NONE',  ( -34.50000000000000000, -113.0140978167138712, 0.3752176474015639918 ) ) ;
#29201 = DIRECTION ( 'NONE',  ( 1.000000000000000000, 0.000000000000000000, 0.000000000000000000 ) ) ;
#29202 = DIRECTION ( 'NONE',  ( 1.000000000000000000, 0.000000000000000000, 0.000000000000000000 ) ) ;
#29203 = ORIENTED_EDGE ( 'NONE', *, *, #14081, .F. ) ;
#29204 = CARTESIAN_POINT ( 'NONE',  ( -40.02454729103296671, -115.1833782841879525, 2.159774454178448710 ) ) ;
#29205 = AXIS2_PLACEMENT_3D ( 'NONE', #9247, #20200, #31208 ) ;
#29206 = AXIS2_PLACEMENT_3D ( 'NONE', #21429, #26686, #4896 ) ;
#29207 = LINE ( 'NONE', #18377, #24578 ) ;
#29208 = CARTESIAN_POINT ( 'NONE',  ( -35.50000000000000711, -116.0140978167138712, -0.4685323525984310677 ) ) ;
#29209 = ORIENTED_EDGE ( 'NONE', *, *, #33586, .F. ) ;
#29210 = VERTEX_POINT ( 'NONE', #30857 ) ;
#29211 = CARTESIAN_POINT ( 'NONE',  ( 70.00001200000001234, -21.98076211353320630, 84.47640122440162713 ) ) ;
#29212 = CYLINDRICAL_SURFACE ( 'NONE', #24186, 12.99999999999999822 ) ;
#29213 = ORIENTED_EDGE ( 'NONE', *, *, #17697, .T. ) ;
#29214 = ORIENTED_EDGE ( 'NONE', *, *, #9420, .F. ) ;
#29215 = CARTESIAN_POINT ( 'NONE',  ( -34.50000000000000000, -112.9813730236132585, -1.624774171495860786 ) ) ;
#29216 = CYLINDRICAL_SURFACE ( 'NONE', #19624, 52.00000000000000711 ) ;
#29217 = ORIENTED_EDGE ( 'NONE', *, *, #28766, .T. ) ;
#29218 = VERTEX_POINT ( 'NONE', #6194 ) ;
#29219 = DIRECTION ( 'NONE',  ( 1.000000000000000000, -5.339440136655842133E-16, -1.047965281155519420E-16 ) ) ;
#29220 = AXIS2_PLACEMENT_3D ( 'NONE', #20911, #31908, #26158 ) ;
#29221 = CARTESIAN_POINT ( 'NONE',  ( -34.50000000000000000, -113.9929510916434339, 10.50625754673586876 ) ) ;
#29222 = DIRECTION ( 'NONE',  ( 0.000000000000000000, 0.000000000000000000, -1.000000000000000000 ) ) ;
#29223 = CARTESIAN_POINT ( 'NONE',  ( -38.00000000000000711, -113.9929510916434339, 11.73841344789285657 ) ) ;
#29224 = CIRCLE ( 'NONE', #33246, 10.99999999999999645 ) ;
#29225 = AXIS2_PLACEMENT_3D ( 'NONE', #16726, #27737, #6111 ) ;
#29226 = CARTESIAN_POINT ( 'NONE',  ( -35.97955704204053262, -115.9929510916434481, 13.11812344617474402 ) ) ;
#29227 = DIRECTION ( 'NONE',  ( -1.000000000000000000, 0.000000000000000000, 0.000000000000000000 ) ) ;
#29228 = CARTESIAN_POINT ( 'NONE',  ( -21.15833593587365513, -27.48076211353314591, 80.99999999999987210 ) ) ;
#29229 = EDGE_CURVE ( 'NONE', #3338, #34725, #7896, .T. ) ;
#29230 = ORIENTED_EDGE ( 'NONE', *, *, #10106, .T. ) ;
#29231 = CARTESIAN_POINT ( 'NONE',  ( 1.498621416870376644, -3.629901386362130586E-16, -4.980000000000000426 ) ) ;
#29232 = LINE ( 'NONE', #31564, #17352 ) ;
#29233 = CIRCLE ( 'NONE', #18290, 10.99999999999999822 ) ;
#29234 = LINE ( 'NONE', #20567, #22604 ) ;
#29235 = VERTEX_POINT ( 'NONE', #27983 ) ;
#29236 = CARTESIAN_POINT ( 'NONE',  ( 0.000000000000000000, 0.000000000000000000, 0.000000000000000000 ) ) ;
#29237 = CARTESIAN_POINT ( 'NONE',  ( -35.50000000000000711, -112.0140978167138712, 0.6252176474015680441 ) ) ;
#29238 = DIRECTION ( 'NONE',  ( 1.032573497605238773E-16, -6.938893903907203726E-17, -1.000000000000000000 ) ) ;
#29239 = EDGE_CURVE ( 'NONE', #8797, #17557, #30903, .T. ) ;
#29240 = DIRECTION ( 'NONE',  ( -1.000000000000000000, 5.339440136655843119E-16, 0.000000000000000000 ) ) ;
#29241 = DIRECTION ( 'NONE',  ( -0.000000000000000000, 0.000000000000000000, -1.000000000000000000 ) ) ;
#29242 = ORIENTED_EDGE ( 'NONE', *, *, #15238, .T. ) ;
#29243 = CARTESIAN_POINT ( 'NONE',  ( -34.49999999999998579, -1.387778780781445676E-14, 110.0000000000000000 ) ) ;
#29244 = CARTESIAN_POINT ( 'NONE',  ( -34.50000000000000000, -116.7615919857705080, -1.632210089000343700 ) ) ;
#29245 = DIRECTION ( 'NONE',  ( 0.000000000000000000, 0.000000000000000000, 1.000000000000000000 ) ) ;
#29246 = ORIENTED_EDGE ( 'NONE', *, *, #3533, .F. ) ;
#29247 = VERTEX_POINT ( 'NONE', #19845 ) ;
#29248 = CARTESIAN_POINT ( 'NONE',  ( -36.02454729103298092, -114.4734759653044307, 3.097274454178448710 ) ) ;
#29249 = VECTOR ( 'NONE', #21268, 1000.000000000000000 ) ;
#29250 =( NAMED_UNIT ( * ) SI_UNIT ( $, .STERADIAN. ) SOLID_ANGLE_UNIT ( ) );
#29251 = CARTESIAN_POINT ( 'NONE',  ( 8.000000000000000000, -6.336799421339700977, -16.31134495048491573 ) ) ;
#29252 = ORIENTED_EDGE ( 'NONE', *, *, #33464, .F. ) ;
#29253 = ORIENTED_EDGE ( 'NONE', *, *, #34721, .T. ) ;
#29254 = CARTESIAN_POINT ( 'NONE',  ( -35.50000000000000000, -115.0140978167138712, -0.6247823525984408377 ) ) ;
#29255 = CYLINDRICAL_SURFACE ( 'NONE', #30978, 22.00000000000000000 ) ;
#29256 = CARTESIAN_POINT ( 'NONE',  ( 0.000000000000000000, 0.000000000000000000, 0.000000000000000000 ) ) ;
#29257 = ADVANCED_BREP_SHAPE_REPRESENTATION ( '', ( #22248, #21307 ), #27126 ) ;
#29258 = CARTESIAN_POINT ( 'NONE',  ( -38.00000068757622529, -114.9929510916434339, 12.61439929482944855 ) ) ;
#29259 = DIRECTION ( 'NONE',  ( 1.000000000000000000, -0.000000000000000000, 0.000000000000000000 ) ) ;
#29260 = CARTESIAN_POINT ( 'NONE',  ( -34.50000000000000000, -114.9929510916434339, 12.57451923796416082 ) ) ;
#29261 = DIRECTION ( 'NONE',  ( -1.000000000000000000, 0.000000000000000000, 0.000000000000000000 ) ) ;
#29262 = EDGE_CURVE ( 'NONE', #30657, #2467, #17154, .T. ) ;
#29263 = ADVANCED_FACE ( 'NONE', ( #3504, #11761 ), #25826, .F. ) ;
#29264 = CARTESIAN_POINT ( 'NONE',  ( 39.30000000000000426, -10.99999999999999112, 0.000000000000000000 ) ) ;
#29265 = EDGE_LOOP ( 'NONE', ( #5535, #2153, #8545, #360 ) ) ;
#29266 = CARTESIAN_POINT ( 'NONE',  ( -36.31249999999994316, -115.9929510916434481, 13.11852480586264846 ) ) ;
#29267 = CARTESIAN_POINT ( 'NONE',  ( -35.50000000000000711, -114.3474311500471430, -1.624782352598427959 ) ) ;
#29268 = DIRECTION ( 'NONE',  ( 0.000000000000000000, 0.000000000000000000, 1.000000000000000000 ) ) ;
#29269 = CARTESIAN_POINT ( 'NONE',  ( 4.000000000000003553, -19.83898331853694685, 9.508666619816580123 ) ) ;
#29270 = DIRECTION ( 'NONE',  ( -1.000000000000000000, -0.000000000000000000, 0.000000000000000000 ) ) ;
#29271 = EDGE_LOOP ( 'NONE', ( #31399, #15886 ) ) ;
#29272 = VECTOR ( 'NONE', #17847, 1000.000000000000000 ) ;
#29273 = DIRECTION ( 'NONE',  ( -1.000000000000000000, -1.836970198721029934E-16, -0.000000000000000000 ) ) ;
#29274 = DIRECTION ( 'NONE',  ( -1.000000000000000000, 0.000000000000000000, 0.000000000000000000 ) ) ;
#29275 = CARTESIAN_POINT ( 'NONE',  ( -50.00000000000000000, -2.775557561562891351E-14, 110.0000000000000000 ) ) ;
#29276 = CARTESIAN_POINT ( 'NONE',  ( -39.49999999999999289, -14.67619866229204284, 93.25874355921412473 ) ) ;
#29277 = ORIENTED_EDGE ( 'NONE', *, *, #143, .T. ) ;
#29278 = ADVANCED_FACE ( 'NONE', ( #19672 ), #14453, .T. ) ;
#29279 = CARTESIAN_POINT ( 'NONE',  ( -37.05926240293133134, -115.0000000000000000, 4.878524454178448266 ) ) ;
#29280 = DIRECTION ( 'NONE',  ( 0.000000000000000000, 0.000000000000000000, -1.000000000000000000 ) ) ;
#29281 = CARTESIAN_POINT ( 'NONE',  ( 0.000000000000000000, 1.347111479062088405E-15, -11.00000000000000000 ) ) ;
#29282 = ADVANCED_FACE ( 'NONE', ( #31030 ), #23872, .F. ) ;
#29283 = EDGE_LOOP ( 'NONE', ( #11296, #22696, #2050, #12796 ) ) ;
#29284 = ORIENTED_EDGE ( 'NONE', *, *, #21, .T. ) ;
#29285 = DIRECTION ( 'NONE',  ( -1.000000000000000000, -1.734723475976807094E-16, 0.000000000000000000 ) ) ;
#29286 = DIRECTION ( 'NONE',  ( -0.000000000000000000, 1.000000000000000000, 0.000000000000000000 ) ) ;
#29287 = ORIENTED_EDGE ( 'NONE', *, *, #17852, .T. ) ;
#29288 = CARTESIAN_POINT ( 'NONE',  ( -38.30190309005061522, -111.0245472910330022, 6.527725545821552622 ) ) ;
#29289 = ORIENTED_EDGE ( 'NONE', *, *, #312, .F. ) ;
#29290 = ORIENTED_EDGE ( 'NONE', *, *, #16121, .T. ) ;
#29291 = EDGE_LOOP ( 'NONE', ( #12790, #13199, #22039, #7375 ) ) ;
#29292 = DIRECTION ( 'NONE',  ( -1.000000000000000000, 0.000000000000000000, 0.000000000000000000 ) ) ;
#29293 = EDGE_CURVE ( 'NONE', #17460, #2675, #19381, .T. ) ;
#29294 = DIRECTION ( 'NONE',  ( -1.000000000000000000, 0.000000000000000000, 0.000000000000000000 ) ) ;
#29295 = ORIENTED_EDGE ( 'NONE', *, *, #2779, .F. ) ;
#29296 = VERTEX_POINT ( 'NONE', #27034 ) ;
#29297 = CIRCLE ( 'NONE', #31575, 14.00000000000000000 ) ;
#29298 = DIRECTION ( 'NONE',  ( -1.000000000000000000, 0.000000000000000000, 0.000000000000000000 ) ) ;
#29299 = CYLINDRICAL_SURFACE ( 'NONE', #27007, 15.49899999999998457 ) ;
#29301 = VERTEX_POINT ( 'NONE', #15661 ) ;
#29300 = CIRCLE ( 'NONE', #4022, 7.199999999999993960 ) ;
#29302 = DIRECTION ( 'NONE',  ( 0.000000000000000000, 0.000000000000000000, 1.000000000000000000 ) ) ;
#29303 = VECTOR ( 'NONE', #34205, 1000.000000000000000 ) ;
#29304 = CARTESIAN_POINT ( 'NONE',  ( 6.896599878636562764, -12.98179148322720167, -1.200000000000006617 ) ) ;
#29305 = CARTESIAN_POINT ( 'NONE',  ( 65.00000000000001421, 55.12602127901487847, 78.31438535856030114 ) ) ;
#29306 = CARTESIAN_POINT ( 'NONE',  ( -35.98977351030467986, -115.9929510916434481, 14.11852173794918563 ) ) ;
#29307 = ADVANCED_FACE ( 'NONE', ( #32072 ), #21252, .T. ) ;
#29308 = EDGE_CURVE ( 'NONE', #10764, #31128, #11909, .T. ) ;
#29309 = CARTESIAN_POINT ( 'NONE',  ( -2.000000000000001776, 0.000000000000000000, 0.000000000000000000 ) ) ;
#29310 = CARTESIAN_POINT ( 'NONE',  ( -35.62769128460905677, -115.4561184093552413, 7.691024454178449155 ) ) ;
#29311 = ADVANCED_FACE ( 'NONE', ( #2015 ), #18378, .T. ) ;
#29312 = CARTESIAN_POINT ( 'NONE',  ( -34.50000000000000000, -115.9929510916434481, 12.39849696637031684 ) ) ;
#29313 = DIRECTION ( 'NONE',  ( -0.000000000000000000, 0.000000000000000000, -1.000000000000000000 ) ) ;
#29314 = DIRECTION ( 'NONE',  ( -1.000000000000000000, 0.000000000000000000, 0.000000000000000000 ) ) ;
#29315 = DIRECTION ( 'NONE',  ( -1.000000000000000000, -0.000000000000000000, -0.000000000000000000 ) ) ;
#29316 = DIRECTION ( 'NONE',  ( 0.000000000000000000, 0.000000000000000000, -1.000000000000000000 ) ) ;
#29317 = DIRECTION ( 'NONE',  ( -1.000000000000000000, -0.000000000000000000, 0.000000000000000000 ) ) ;
#29318 = CARTESIAN_POINT ( 'NONE',  ( 8.000000000000000000, -13.60411018104326963, 12.96676809804144348 ) ) ;
#29319 = ORIENTED_EDGE ( 'NONE', *, *, #7618, .T. ) ;
#29320 = ADVANCED_FACE ( 'NONE', ( #10640 ), #19083, .T. ) ;
#29321 = CARTESIAN_POINT ( 'NONE',  ( -35.81662171581203324, -110.9754527089670546, 8.215225545821551734 ) ) ;
#29322 = CYLINDRICAL_SURFACE ( 'NONE', #12946, 4.000000000000003553 ) ;
#29323 = CARTESIAN_POINT ( 'NONE',  ( -35.50000000000000000, -113.0256022645180707, 0.8765908897032291813 ) ) ;
#29324 = EDGE_CURVE ( 'NONE', #6382, #35356, #32248, .T. ) ;
#29325 = ORIENTED_EDGE ( 'NONE', *, *, #13057, .F. ) ;
#29326 = CIRCLE ( 'NONE', #32756, 20.00000000000001066 ) ;
#29327 = VERTEX_POINT ( 'NONE', #18728 ) ;
#29328 = DIRECTION ( 'NONE',  ( -1.000000000000000000, -0.000000000000000000, -0.000000000000000000 ) ) ;
#29329 = VERTEX_POINT ( 'NONE', #7573 ) ;
#29330 = ORIENTED_EDGE ( 'NONE', *, *, #27117, .T. ) ;
#29331 = MECHANICAL_DESIGN_GEOMETRIC_PRESENTATION_REPRESENTATION (  '', ( #24727 ), #9181 ) ;
#29332 = ORIENTED_EDGE ( 'NONE', *, *, #34360, .T. ) ;
#29333 = AXIS2_PLACEMENT_3D ( 'NONE', #35456, #35285, #29691 ) ;
#29334 = VERTEX_POINT ( 'NONE', #35143 ) ;
#29335 = CYLINDRICAL_SURFACE ( 'NONE', #30928, 11.00000000000001066 ) ;
#29336 = LINE ( 'NONE', #32028, #6770 ) ;
#29337 = DIRECTION ( 'NONE',  ( -1.000000000000000000, 0.000000000000000000, 0.000000000000000000 ) ) ;
#29338 = EDGE_CURVE ( 'NONE', #15438, #1317, #3318, .T. ) ;
#29339 = DIRECTION ( 'NONE',  ( 0.000000000000000000, 0.000000000000000000, 1.000000000000000000 ) ) ;
#29340 = ORIENTED_EDGE ( 'NONE', *, *, #11929, .F. ) ;
#29341 = VERTEX_POINT ( 'NONE', #21596 ) ;
#29342 = CARTESIAN_POINT ( 'NONE',  ( -35.50000000000000711, -113.8159288351371714, 1.978028123174813802 ) ) ;
#29343 = EDGE_CURVE ( 'NONE', #21628, #4187, #12504, .T. ) ;
#29344 = CARTESIAN_POINT ( 'NONE',  ( 5.400000000000071410, 0.9999999999999662492, -32.00000000000000000 ) ) ;
#29345 = VECTOR ( 'NONE', #6923, 1000.000000000000000 ) ;
#29346 = PLANE ( 'NONE',  #6903 ) ;
#29347 = EDGE_LOOP ( 'NONE', ( #25858, #26278, #31851, #3719 ) ) ;
#29348 = CARTESIAN_POINT ( 'NONE',  ( 4.000000000000000000, -17.56975900509168298, -9.555290079479433984 ) ) ;
#29349 = AXIS2_PLACEMENT_3D ( 'NONE', #27546, #18890, #2533 ) ;
#29350 = CARTESIAN_POINT ( 'NONE',  ( 8.000000000000000000, 10.62435788049443808, 13.16139124467922272 ) ) ;
#29351 = CARTESIAN_POINT ( 'NONE',  ( -34.50000000000000000, -114.9929501463477663, 10.50247632894551231 ) ) ;
#29352 = CYLINDRICAL_SURFACE ( 'NONE', #27502, 3.799999999999999822 ) ;
#29353 = EDGE_CURVE ( 'NONE', #440, #10254, #29559, .T. ) ;
#29354 = CARTESIAN_POINT ( 'NONE',  ( -36.03906250000000000, -114.9929510916434339, 13.11852480586264669 ) ) ;
#29355 = CARTESIAN_POINT ( 'NONE',  ( 0.000000000000000000, 0.000000000000000000, 0.000000000000000000 ) ) ;
#29356 = VECTOR ( 'NONE', #25465, 1000.000000000000000 ) ;
#29357 = CIRCLE ( 'NONE', #26477, 10.50000000000000178 ) ;
#29358 = EDGE_CURVE ( 'NONE', #30249, #28744, #29907, .T. ) ;
#29359 = CARTESIAN_POINT ( 'NONE',  ( -34.50000000000000000, -114.0743172650041686, 9.508870970061893857 ) ) ;
#29360 = CYLINDRICAL_SURFACE ( 'NONE', #4418, 3.799999999999999822 ) ;
#29361 = DIRECTION ( 'NONE',  ( -1.174092375852890260E-15, 4.222049128630259891E-16, 1.000000000000000000 ) ) ;
#29362 =( LENGTH_UNIT ( ) NAMED_UNIT ( * ) SI_UNIT ( .MILLI., .METRE. ) );
#29363 = ORIENTED_EDGE ( 'NONE', *, *, #28431, .F. ) ;
#29364 = DIRECTION ( 'NONE',  ( -1.000000000000000000, 0.000000000000000000, 0.000000000000000000 ) ) ;
#29365 = DIRECTION ( 'NONE',  ( -1.734723475976807094E-16, 0.4999999999999989453, 0.8660254037844392627 ) ) ;
#29366 = VERTEX_POINT ( 'NONE', #18910 ) ;
#29367 = CARTESIAN_POINT ( 'NONE',  ( -37.54084996655477369, -114.9929510916434339, 13.11692036158760466 ) ) ;
#29368 = VERTEX_POINT ( 'NONE', #7745 ) ;
#29369 = CARTESIAN_POINT ( 'NONE',  ( -38.97545270896704039, -113.1123104723225197, 6.847274454178450931 ) ) ;
#29370 = FACE_OUTER_BOUND ( 'NONE', #31403, .T. ) ;
#29371 = VERTEX_POINT ( 'NONE', #29732 ) ;
#29372 = ORIENTED_EDGE ( 'NONE', *, *, #26420, .F. ) ;
#29373 = CARTESIAN_POINT ( 'NONE',  ( 0.000000000000000000, 0.000000000000000000, -50.00000000000000000 ) ) ;
#29374 = AXIS2_PLACEMENT_3D ( 'NONE', #31632, #15231, #12739 ) ;
#29375 = ORIENTED_EDGE ( 'NONE', *, *, #10617, .T. ) ;
#29376 = CARTESIAN_POINT ( 'NONE',  ( -37.76916472181487450, -111.9754527089670404, 8.534774454178448266 ) ) ;
#29377 = AXIS2_PLACEMENT_3D ( 'NONE', #35082, #21364, #8567 ) ;
#29378 = LINE ( 'NONE', #26680, #2161 ) ;
#29379 = CARTESIAN_POINT ( 'NONE',  ( -6.938893903907228378E-15, 0.7408941433508786645, -1.200000000000006617 ) ) ;
#29380 = VERTEX_POINT ( 'NONE', #5075 ) ;
#29381 = VERTEX_POINT ( 'NONE', #2377 ) ;
#29382 = DIRECTION ( 'NONE',  ( 0.000000000000000000, 0.5877852522924739143, -0.8090169943749468962 ) ) ;
#29383 = AXIS2_PLACEMENT_3D ( 'NONE', #31546, #6870, #17843 ) ;
#29384 = SURFACE_STYLE_FILL_AREA ( #27039 ) ;
#29385 = EDGE_CURVE ( 'NONE', #14203, #24982, #23793, .T. ) ;
#29386 = AXIS2_PLACEMENT_3D ( 'NONE', #12945, #35105, #12769 ) ;
#29387 = CARTESIAN_POINT ( 'NONE',  ( 8.000000000000007105, 0.000000000000000000, 0.000000000000000000 ) ) ;
#29388 = ORIENTED_EDGE ( 'NONE', *, *, #6680, .T. ) ;
#29389 = ORIENTED_EDGE ( 'NONE', *, *, #34791, .T. ) ;
#29390 = CARTESIAN_POINT ( 'NONE',  ( -34.50000000000000000, -111.0140978167138570, 0.7189676474015717078 ) ) ;
#29391 = EDGE_CURVE ( 'NONE', #35140, #28899, #24329, .T. ) ;
#29392 = PRODUCT_DEFINITION_SHAPE ( 'NONE', 'NONE',  #35627 ) ;
#29393 = DIRECTION ( 'NONE',  ( 1.000000000000000000, 0.000000000000000000, 0.000000000000000000 ) ) ;
#29394 = ORIENTED_EDGE ( 'NONE', *, *, #1703, .F. ) ;
#29395 = VERTEX_POINT ( 'NONE', #35492 ) ;
#29396 = CARTESIAN_POINT ( 'NONE',  ( -35.50000000000000711, -114.1091535596544873, 9.513028657562415447 ) ) ;
#29397 = CARTESIAN_POINT ( 'NONE',  ( -34.50000000000000000, -113.9948283797722439, 10.50648163149984171 ) ) ;
#29398 = CARTESIAN_POINT ( 'NONE',  ( 8.000000000000007105, 5.679790370316031733, 7.613867765417614564 ) ) ;
#29399 = DIRECTION ( 'NONE',  ( 0.000000000000000000, 0.000000000000000000, 1.000000000000000000 ) ) ;
#29400 = CARTESIAN_POINT ( 'NONE',  ( -37.50818044754229419, -113.9929510916434339, 13.11847460610629845 ) ) ;
#29401 = CARTESIAN_POINT ( 'NONE',  ( -37.56526046546249376, -115.9929510916434481, 13.11451721564129258 ) ) ;
#29402 = DIRECTION ( 'NONE',  ( -1.000000000000000000, 0.000000000000000000, 0.000000000000000000 ) ) ;
#29403 = CYLINDRICAL_SURFACE ( 'NONE', #3173, 22.00000000000000000 ) ;
#29404 = ORIENTED_EDGE ( 'NONE', *, *, #24916, .T. ) ;
#29405 = CIRCLE ( 'NONE', #1832, 1.000000000000000888 ) ;
#29406 = DIRECTION ( 'NONE',  ( 0.000000000000000000, 0.000000000000000000, 1.000000000000000000 ) ) ;
#29407 = DIRECTION ( 'NONE',  ( 0.000000000000000000, 0.000000000000000000, 1.000000000000000000 ) ) ;
#29408 = DIRECTION ( 'NONE',  ( 1.000000000000000000, -5.339440136655842133E-16, -1.047965281155519420E-16 ) ) ;
#29409 = ORIENTED_EDGE ( 'NONE', *, *, #8909, .T. ) ;
#29410 = LINE ( 'NONE', #31913, #4391 ) ;
#29411 = CARTESIAN_POINT ( 'NONE',  ( -35.50000000000000711, -114.9307644833806137, -1.624782352598427959 ) ) ;
#29412 = DIRECTION ( 'NONE',  ( -1.000000000000000000, 0.000000000000000000, 0.000000000000000000 ) ) ;
#29413 = DIRECTION ( 'NONE',  ( 1.110223024625156540E-16, 1.000000000000000000, 0.000000000000000000 ) ) ;
#29414 = FACE_OUTER_BOUND ( 'NONE', #8360, .T. ) ;
#29415 = ORIENTED_EDGE ( 'NONE', *, *, #31762, .T. ) ;
#29416 = DIRECTION ( 'NONE',  ( 0.000000000000000000, 0.000000000000000000, -1.000000000000000000 ) ) ;
#29417 = CARTESIAN_POINT ( 'NONE',  ( -35.50000000000000000, -113.0974311500471714, -2.624782352598442614 ) ) ;
#29418 = CARTESIAN_POINT ( 'NONE',  ( 7.999999999999992895, 36.06787431788677623, 37.45808914225502662 ) ) ;
#29419 = ORIENTED_EDGE ( 'NONE', *, *, #34825, .F. ) ;
#29420 = ORIENTED_EDGE ( 'NONE', *, *, #8269, .F. ) ;
#29421 = CARTESIAN_POINT ( 'NONE',  ( -37.05926240293133134, -115.0000000000000000, 7.878524454178450043 ) ) ;
#29422 = CARTESIAN_POINT ( 'NONE',  ( 8.000000000000007105, -11.27190672109268377, 0.3151488735047419665 ) ) ;
#29423 = ORIENTED_EDGE ( 'NONE', *, *, #35444, .F. ) ;
#29424 = ORIENTED_EDGE ( 'NONE', *, *, #13421, .T. ) ;
#29425 = CARTESIAN_POINT ( 'NONE',  ( -34.50000000000000000, -113.0140978167138712, 0.8752176474015934682 ) ) ;
#29426 = EDGE_CURVE ( 'NONE', #29329, #17886, #32040, .T. ) ;
#29427 = CIRCLE ( 'NONE', #23687, 8.000000000000010658 ) ;
#29428 = CIRCLE ( 'NONE', #23667, 4.800000000000005151 ) ;
#29429 = CARTESIAN_POINT ( 'NONE',  ( -42.49999999999999289, -23.26666049839546702, 88.29903810567660116 ) ) ;
#29430 = DIRECTION ( 'NONE',  ( 0.000000000000000000, 0.9510565162951545304, -0.3090169943749448977 ) ) ;
#29431 = CARTESIAN_POINT ( 'NONE',  ( -35.50000000000000000, -113.9929510916434623, 10.50625754673586876 ) ) ;
#29432 = CARTESIAN_POINT ( 'NONE',  ( -90.00000000000002842, 1.297889732222515536E-15, 6.765000000000052083 ) ) ;
#29433 = CARTESIAN_POINT ( 'NONE',  ( 0.000000000000000000, 14.30000000000000071, 3.000000000000002665 ) ) ;
#29434 = EDGE_CURVE ( 'NONE', #26484, #35307, #27385, .T. ) ;
#29435 = CARTESIAN_POINT ( 'NONE',  ( -34.50000000000000000, -112.1403507321855528, -1.128496220798856253 ) ) ;
#29436 = CARTESIAN_POINT ( 'NONE',  ( -35.93867112612154813, -114.9929510916434339, 14.11732072679899197 ) ) ;
#29437 = CARTESIAN_POINT ( 'NONE',  ( 0.000000000000000000, 12.46108038583334299, -15.64357617738982142 ) ) ;
#29438 = MECHANICAL_DESIGN_GEOMETRIC_PRESENTATION_REPRESENTATION (  '', ( #3582 ), #23700 ) ;
#29439 = DIRECTION ( 'NONE',  ( -1.000000000000000000, 0.000000000000000000, 0.000000000000000000 ) ) ;
#29440 = VERTEX_POINT ( 'NONE', #16897 ) ;
#29441 = CARTESIAN_POINT ( 'NONE',  ( -36.00585935943765747, -115.9929510916434481, 13.11852578240983291 ) ) ;
#29442 = CARTESIAN_POINT ( 'NONE',  ( -35.50000000000000711, -115.0795240838853886, -1.623175561345890472 ) ) ;
#29443 =( NAMED_UNIT ( * ) SI_UNIT ( $, .STERADIAN. ) SOLID_ANGLE_UNIT ( ) );
#29444 = CARTESIAN_POINT ( 'NONE',  ( 4.000000000000000000, 12.46108038583314936, 15.64357617739001860 ) ) ;
#29445 = DIRECTION ( 'NONE',  ( -1.000000000000000000, 0.000000000000000000, 0.000000000000000000 ) ) ;
#29446 = ORIENTED_EDGE ( 'NONE', *, *, #32159, .F. ) ;
#29447 = CARTESIAN_POINT ( 'NONE',  ( -90.00000000000002842, 0.000000000000000000, 6.938893903907228378E-15 ) ) ;
#29448 = LINE ( 'NONE', #26753, #27917 ) ;
#29449 = DIRECTION ( 'NONE',  ( 0.000000000000000000, 0.000000000000000000, 1.000000000000000000 ) ) ;
#29450 = CARTESIAN_POINT ( 'NONE',  ( 8.000000000000000000, 14.87816164169115218, 4.342730381189920941 ) ) ;
#29451 = AXIS2_PLACEMENT_3D ( 'NONE', #23708, #9486, #34700 ) ;
#29452 =( GEOMETRIC_REPRESENTATION_CONTEXT ( 3 ) GLOBAL_UNCERTAINTY_ASSIGNED_CONTEXT ( ( #28631 ) ) GLOBAL_UNIT_ASSIGNED_CONTEXT ( ( #30444, #25032, #11519 ) ) REPRESENTATION_CONTEXT ( 'NONE', 'WORKASPACE' ) );
#29453 = CARTESIAN_POINT ( 'NONE',  ( -35.99999999999999289, -114.0592624029313242, 7.503524454178450043 ) ) ;
#29454 = VECTOR ( 'NONE', #10019, 1000.000000000000000 ) ;
#29455 = LINE ( 'NONE', #32149, #27343 ) ;
#29456 = DIRECTION ( 'NONE',  ( 0.000000000000000000, 0.000000000000000000, -1.000000000000000000 ) ) ;
#29457 = ORIENTED_EDGE ( 'NONE', *, *, #3046, .T. ) ;
#29458 = ADVANCED_FACE ( 'NONE', ( #22485 ), #21958, .T. ) ;
#29459 = ORIENTED_EDGE ( 'NONE', *, *, #19865, .F. ) ;
#29460 = DIRECTION ( 'NONE',  ( 1.000000000000000000, -0.000000000000000000, -0.000000000000000000 ) ) ;
#29461 = DIRECTION ( 'NONE',  ( -1.000000000000000000, 0.000000000000000000, 0.000000000000000000 ) ) ;
#29462 = CARTESIAN_POINT ( 'NONE',  ( -9.999999999999994671, 0.000000000000000000, 0.000000000000000000 ) ) ;
#29463 = ORIENTED_EDGE ( 'NONE', *, *, #6169, .F. ) ;
#29464 = CARTESIAN_POINT ( 'NONE',  ( -37.05926240293131713, -112.0000000000000142, 9.621475545821551734 ) ) ;
#29465 = EDGE_LOOP ( 'NONE', ( #20440, #25753 ) ) ;
#29466 =( LENGTH_UNIT ( ) NAMED_UNIT ( * ) SI_UNIT ( .MILLI., .METRE. ) );
#29468 = ORIENTED_EDGE ( 'NONE', *, *, #15238, .F. ) ;
#29467 = AXIS2_PLACEMENT_3D ( 'NONE', #17148, #25276, #8875 ) ;
#29469 = ORIENTED_EDGE ( 'NONE', *, *, #19777, .T. ) ;
#29470 = CARTESIAN_POINT ( 'NONE',  ( -4.000000000000000000, -2.710505431213761085E-17, 54.99999999999999289 ) ) ;
#29471 = ADVANCED_FACE ( 'NONE', ( #11166, #33475 ), #32955, .F. ) ;
#29472 = ADVANCED_FACE ( 'NONE', ( #30258 ), #22654, .F. ) ;
#29473 = AXIS2_PLACEMENT_3D ( 'NONE', #2658, #35599, #30017 ) ;
#29474 = CARTESIAN_POINT ( 'NONE',  ( 7.999999999999992895, 0.000000000000000000, 0.000000000000000000 ) ) ;
#29475 = EDGE_LOOP ( 'NONE', ( #34503, #6418, #2956, #12661 ) ) ;
#29476 = ORIENTED_EDGE ( 'NONE', *, *, #9946, .T. ) ;
#29477 = DIRECTION ( 'NONE',  ( -1.000000000000000000, -0.000000000000000000, -0.000000000000000000 ) ) ;
#29478 = AXIS2_PLACEMENT_3D ( 'NONE', #19459, #3447, #27919 ) ;
#29479 = DIRECTION ( 'NONE',  ( -1.000000000000000000, 0.000000000000000000, 0.000000000000000000 ) ) ;
#29480 = EDGE_CURVE ( 'NONE', #27160, #4061, #11348, .T. ) ;
#29481 = ORIENTED_EDGE ( 'NONE', *, *, #21144, .T. ) ;
#29482 = CIRCLE ( 'NONE', #15080, 13.99999999999999645 ) ;
#29483 = CARTESIAN_POINT ( 'NONE',  ( 50.00000000000000000, 0.000000000000000000, 0.000000000000000000 ) ) ;
#29484 = DIRECTION ( 'NONE',  ( -1.000000000000000000, 0.000000000000000000, 0.000000000000000000 ) ) ;
#29485 = DIRECTION ( 'NONE',  ( -1.000000000000000000, 0.000000000000000000, 0.000000000000000000 ) ) ;
#29486 = DIRECTION ( 'NONE',  ( 1.226634733346697831E-16, 0.2588190451025240701, -0.9659258262890673130 ) ) ;
#29487 = CARTESIAN_POINT ( 'NONE',  ( -38.45611840935523418, -115.3723087153909432, 8.066024454178448266 ) ) ;
#29488 = CARTESIAN_POINT ( 'NONE',  ( -34.50000000000000000, -115.9929510916434481, 11.91443571948720148 ) ) ;
#29489 = FACE_OUTER_BOUND ( 'NONE', #23924, .T. ) ;
#29490 = CARTESIAN_POINT ( 'NONE',  ( 8.000000000000000000, -18.48663108841361336, 3.384281271887747078 ) ) ;
#29491 = AXIS2_PLACEMENT_3D ( 'NONE', #18936, #21278, #15690 ) ;
#29492 = FACE_OUTER_BOUND ( 'NONE', #5581, .T. ) ;
#29493 = CARTESIAN_POINT ( 'NONE',  ( 0.000000000000000000, 7.317194182740155206, 18.61340026142654125 ) ) ;
#29494 = LINE ( 'NONE', #16131, #11851 ) ;
#29495 = CARTESIAN_POINT ( 'NONE',  ( 0.000000000000000000, 0.000000000000000000, 0.000000000000000000 ) ) ;
#29496 = EDGE_LOOP ( 'NONE', ( #5542, #15781, #5291, #20771 ) ) ;
#29497 = CARTESIAN_POINT ( 'NONE',  ( -36.94073759706868287, -115.9999999999999858, 5.871475545821550845 ) ) ;
#29498 = CARTESIAN_POINT ( 'NONE',  ( 0.000000000000000000, 15.17386234660384581, 15.92965478239621824 ) ) ;
#29499 = ADVANCED_FACE ( 'NONE', ( #13867 ), #8, .T. ) ;
#29500 = CARTESIAN_POINT ( 'NONE',  ( 3.872983346207517386, -1.000000000000028644, 65.00000000000000000 ) ) ;
#29501 = EDGE_LOOP ( 'NONE', ( #8508, #33135, #12220, #5018 ) ) ;
#29502 = ORIENTED_EDGE ( 'NONE', *, *, #13775, .F. ) ;
#29503 = CIRCLE ( 'NONE', #32369, 3.799999999999999822 ) ;
#29504 = DIRECTION ( 'NONE',  ( -0.000000000000000000, 2.543449303551180694E-16, -1.000000000000000000 ) ) ;
#29505 = AXIS2_PLACEMENT_3D ( 'NONE', #33324, #8649, #27586 ) ;
#29506 = DIRECTION ( 'NONE',  ( 0.000000000000000000, 0.000000000000000000, 1.000000000000000000 ) ) ;
#29507 = ORIENTED_EDGE ( 'NONE', *, *, #16313, .F. ) ;
#29508 = VECTOR ( 'NONE', #8712, 1000.000000000000000 ) ;
#29509 = ORIENTED_EDGE ( 'NONE', *, *, #6432, .T. ) ;
#29510 = EDGE_LOOP ( 'NONE', ( #3434, #14909, #7194, #22131 ) ) ;
#29511 = ADVANCED_FACE ( 'NONE', ( #8460 ), #7340, .T. ) ;
#29512 = CARTESIAN_POINT ( 'NONE',  ( 0.000000000000000000, -41.20225022064654041, 23.63323037071388200 ) ) ;
#29513 = EDGE_CURVE ( 'NONE', #18380, #18157, #17109, .T. ) ;
#29514 = CARTESIAN_POINT ( 'NONE',  ( -37.88768952767750875, -112.0245472910329880, 9.527725545821553510 ) ) ;
#29515 = ADVANCED_FACE ( 'NONE', ( #19765 ), #24678, .F. ) ;
#29516 = DIRECTION ( 'NONE',  ( 1.000000000000000000, 0.000000000000000000, 0.000000000000000000 ) ) ;
#29517 = CARTESIAN_POINT ( 'NONE',  ( -55.00000000000000000, -2.775557561562891351E-14, 110.0000000000000000 ) ) ;
#29518 = VERTEX_POINT ( 'NONE', #25213 ) ;
#29519 = ORIENTED_EDGE ( 'NONE', *, *, #8411, .T. ) ;
#29520 = AXIS2_PLACEMENT_3D ( 'NONE', #19219, #19403, #15985 ) ;
#29521 = CARTESIAN_POINT ( 'NONE',  ( -35.50000000000000711, -112.8655373925166572, 1.864575885149403423 ) ) ;
#29522 = CIRCLE ( 'NONE', #3074, 7.199999999999993072 ) ;
#29523 = DIRECTION ( 'NONE',  ( -1.000000000000000000, -0.000000000000000000, -0.000000000000000000 ) ) ;
#29524 = EDGE_CURVE ( 'NONE', #29876, #35108, #11514, .T. ) ;
#29525 = CARTESIAN_POINT ( 'NONE',  ( -34.49999999999998579, -25.98076211353322051, 84.99999999999992895 ) ) ;
#29526 = ORIENTED_EDGE ( 'NONE', *, *, #21550, .T. ) ;
#29527 = CARTESIAN_POINT ( 'NONE',  ( -55.00000000000000000, -25.98076211353320275, 84.99999999999994316 ) ) ;
#29528 = ADVANCED_FACE ( 'NONE', ( #28089 ), #5769, .T. ) ;
#29529 = CARTESIAN_POINT ( 'NONE',  ( -34.50000000000000000, -113.8159288351371714, 1.978028123174813802 ) ) ;
#29530 = CARTESIAN_POINT ( 'NONE',  ( -34.50300906734827322, -114.9929510916434339, 12.71660600561482468 ) ) ;
#29531 = VECTOR ( 'NONE', #24614, 1000.000000000000000 ) ;
#29532 = DIRECTION ( 'NONE',  ( 0.000000000000000000, 0.000000000000000000, -1.000000000000000000 ) ) ;
#29533 = CARTESIAN_POINT ( 'NONE',  ( -37.97447287825094975, -114.9929510916434339, 12.77960891308616809 ) ) ;
#29534 = DIRECTION ( 'NONE',  ( -1.000000000000000000, 0.000000000000000000, -0.000000000000000000 ) ) ;
#29535 = AXIS2_PLACEMENT_3D ( 'NONE', #15168, #11962, #26176 ) ;
#29536 = CARTESIAN_POINT ( 'NONE',  ( -34.50000000000000000, -114.2305202833893816, 9.534416457224700991 ) ) ;
#29537 = DIRECTION ( 'NONE',  ( -1.000000000000000000, -0.000000000000000000, 0.000000000000000000 ) ) ;
#29538 = CARTESIAN_POINT ( 'NONE',  ( -38.00000000000000711, -114.9929510916434339, 11.73841344789285657 ) ) ;
#29539 = CARTESIAN_POINT ( 'NONE',  ( -35.00000000000000000, -114.0000000000000853, 2.000000000000001776 ) ) ;
#29540 = ORIENTED_EDGE ( 'NONE', *, *, #22769, .F. ) ;
#29541 = LINE ( 'NONE', #7018, #23296 ) ;
#29542 = LINE ( 'NONE', #12970, #16898 ) ;
#29543 = VERTEX_POINT ( 'NONE', #33307 ) ;
#29544 = CARTESIAN_POINT ( 'NONE',  ( -37.42187499999997158, -114.9929510916434339, 13.11852480586264669 ) ) ;
#29545 = ORIENTED_EDGE ( 'NONE', *, *, #10425, .F. ) ;
#29546 = CARTESIAN_POINT ( 'NONE',  ( -35.81662171581204746, -117.0245472910329738, 1.784774454178449155 ) ) ;
#29547 = CARTESIAN_POINT ( 'NONE',  ( 0.000000000000000000, -9.508666619816789733, 19.83898331853681896 ) ) ;
#29548 = ADVANCED_FACE ( 'NONE', ( #19599 ), #17078, .T. ) ;
#29549 = ORIENTED_EDGE ( 'NONE', *, *, #23614, .T. ) ;
#29550 = CIRCLE ( 'NONE', #18030, 20.00000000000000000 ) ;
#29551 = EDGE_LOOP ( 'NONE', ( #6735, #32431, #14382, #10759 ) ) ;
#29552 = EDGE_CURVE ( 'NONE', #27214, #11860, #6766, .T. ) ;
#29553 = DIRECTION ( 'NONE',  ( 0.000000000000000000, 0.000000000000000000, 1.000000000000000000 ) ) ;
#29554 = ADVANCED_FACE ( 'NONE', ( #3250 ), #534, .T. ) ;
#29555 = ORIENTED_EDGE ( 'NONE', *, *, #21592, .F. ) ;
#29556 = CARTESIAN_POINT ( 'NONE',  ( -35.69809690994938478, -111.0245472910330022, 2.722274454178449155 ) ) ;
#29557 = LINE ( 'NONE', #35142, #27464 ) ;
#29558 = AXIS2_PLACEMENT_3D ( 'NONE', #21248, #17251, #33470 ) ;
#29559 = LINE ( 'NONE', #32598, #1589 ) ;
#29560 = EDGE_LOOP ( 'NONE', ( #17448, #28304, #23769, #1958 ) ) ;
#29561 = EDGE_LOOP ( 'NONE', ( #6913, #16109 ) ) ;
#29562 = EDGE_CURVE ( 'NONE', #14640, #18916, #29791, .T. ) ;
#29563 = DIRECTION ( 'NONE',  ( 0.000000000000000000, 0.000000000000000000, 1.000000000000000000 ) ) ;
#29564 = EDGE_CURVE ( 'NONE', #21331, #31396, #8493, .T. ) ;
#29565 =( NAMED_UNIT ( * ) PLANE_ANGLE_UNIT ( ) SI_UNIT ( $, .RADIAN. ) );
#29566 = DIRECTION ( 'NONE',  ( -1.000000000000000000, 0.000000000000000000, 0.000000000000000000 ) ) ;
#29567 = EDGE_LOOP ( 'NONE', ( #23142, #18146, #18960, #20423 ) ) ;
#29568 = EDGE_LOOP ( 'NONE', ( #22495, #33078, #27789, #20982 ) ) ;
#29569 = CARTESIAN_POINT ( 'NONE',  ( -34.50000000000000000, -112.8115600290184801, 2.865251044451027074 ) ) ;
#29570 = AXIS2_PLACEMENT_3D ( 'NONE', #32913, #16513, #13993 ) ;
#29571 = DIRECTION ( 'NONE',  ( -1.000000000000000000, 0.000000000000000000, -0.000000000000000000 ) ) ;
#29572 = VERTEX_POINT ( 'NONE', #17967 ) ;
#29573 = CARTESIAN_POINT ( 'NONE',  ( -35.50000000000000711, -114.9912366357066986, 10.44580456020104720 ) ) ;
#29574 = EDGE_CURVE ( 'NONE', #19482, #11865, #3970, .T. ) ;
#29575 = CARTESIAN_POINT ( 'NONE',  ( -34.50000000000000000, -113.9929510916434339, 10.50763272073269405 ) ) ;
#29576 = LINE ( 'NONE', #24344, #26969 ) ;
#29577 = DIRECTION ( 'NONE',  ( -1.000000000000000000, 0.000000000000000000, 0.000000000000000000 ) ) ;
#29578 = CARTESIAN_POINT ( 'NONE',  ( -38.00000000000000711, -113.9929510916434339, 12.44250253426875119 ) ) ;
#29579 = CARTESIAN_POINT ( 'NONE',  ( -35.93473953453761993, -115.9929510916434481, 13.11451721564123396 ) ) ;
#29580 = CARTESIAN_POINT ( 'NONE',  ( -34.49999999999998579, -1.387778780781445676E-14, 110.0000000000000000 ) ) ;
#29582 = VECTOR ( 'NONE', #35271, 1000.000000000000000 ) ;
#29581 = DIRECTION ( 'NONE',  ( 4.662936703425629071E-15, -1.000000000000000000, 4.222049128630314618E-16 ) ) ;
#29583 = VERTEX_POINT ( 'NONE', #882 ) ;
#29584 = DIRECTION ( 'NONE',  ( -1.734723475976807094E-16, 1.000000000000000000, -0.000000000000000000 ) ) ;
#29585 = DIRECTION ( 'NONE',  ( 1.541976423090495387E-16, -1.000000000000000000, 0.000000000000000000 ) ) ;
#29586 = DIRECTION ( 'NONE',  ( -1.000000000000000000, 0.000000000000000000, 0.000000000000000000 ) ) ;
#29587 = EDGE_CURVE ( 'NONE', #29784, #14247, #33838, .T. ) ;
#29588 = ORIENTED_EDGE ( 'NONE', *, *, #19633, .F. ) ;
#29589 = DIRECTION ( 'NONE',  ( 0.000000000000000000, -1.000000000000000000, 0.000000000000000000 ) ) ;
#29590 = EDGE_CURVE ( 'NONE', #32739, #15054, #31135, .T. ) ;
#29591 = CARTESIAN_POINT ( 'NONE',  ( -35.50000000000000711, -113.0557643173828524, -1.624792769101735868 ) ) ;
#29592 = CARTESIAN_POINT ( 'NONE',  ( 7.999999999999992895, -6.109652351742118626, 46.58570277113506819 ) ) ;
#29593 = CARTESIAN_POINT ( 'NONE',  ( -35.50100302244946704, -114.9929510916434339, 12.65121853911337269 ) ) ;
#29594 = DIRECTION ( 'NONE',  ( -1.000000000000000000, 0.000000000000000000, 0.000000000000000000 ) ) ;
#29595 = ORIENTED_EDGE ( 'NONE', *, *, #24034, .T. ) ;
#29596 = CARTESIAN_POINT ( 'NONE',  ( 2.000000000000001776, 0.000000000000000000, 0.000000000000000000 ) ) ;
#29597 = CARTESIAN_POINT ( 'NONE',  ( -35.50000000000000000, -112.8832452823708792, -2.621568770093253953 ) ) ;
#29598 = ORIENTED_EDGE ( 'NONE', *, *, #35012, .T. ) ;
#29599 = VERTEX_POINT ( 'NONE', #9346 ) ;
#29600 = EDGE_CURVE ( 'NONE', #7845, #17749, #6637, .T. ) ;
#29601 = CARTESIAN_POINT ( 'NONE',  ( -35.99999999999999289, -114.0592624029313242, 9.003524454178446490 ) ) ;
#29602 = EDGE_CURVE ( 'NONE', #10254, #8278, #13696, .T. ) ;
#29603 = LINE ( 'NONE', #4942, #29637 ) ;
#29604 = ORIENTED_EDGE ( 'NONE', *, *, #22875, .F. ) ;
#29605 = ORIENTED_EDGE ( 'NONE', *, *, #18321, .F. ) ;
#29606 = CARTESIAN_POINT ( 'NONE',  ( -34.50000000000000000, -114.3474311500471572, -0.6247823525984269599 ) ) ;
#29607 = AXIS2_PLACEMENT_3D ( 'NONE', #3918, #1201, #33794 ) ;
#29608 = AXIS2_PLACEMENT_3D ( 'NONE', #18317, #7861, #26792 ) ;
#29609 = CARTESIAN_POINT ( 'NONE',  ( 7.999999999999992895, 0.000000000000000000, 0.000000000000000000 ) ) ;
#29610 = AXIS2_PLACEMENT_3D ( 'NONE', #21771, #19071, #15071 ) ;
#29611 = CARTESIAN_POINT ( 'NONE',  ( 4.000000000000003553, -30.03615769709763228, 42.44795908868979950 ) ) ;
#29612 = CARTESIAN_POINT ( 'NONE',  ( -37.37500000000009237, -114.9929510916434339, 13.11852480586264669 ) ) ;
#29613 = DIRECTION ( 'NONE',  ( -1.000000000000000000, 0.000000000000000000, 0.000000000000000000 ) ) ;
#29614 = CARTESIAN_POINT ( 'NONE',  ( 0.000000000000000000, 34.03046037009256963, 33.13733193845818903 ) ) ;
#29615 = CARTESIAN_POINT ( 'NONE',  ( -34.50000000000000000, -113.2224311500466030, -1.624782352598427959 ) ) ;
#29616 = VECTOR ( 'NONE', #27233, 1000.000000000000000 ) ;
#29617 = CARTESIAN_POINT ( 'NONE',  ( -10.00000000000000000, 0.000000000000000000, 0.000000000000000000 ) ) ;
#29618 = CARTESIAN_POINT ( 'NONE',  ( 4.000000000000003553, 36.06787431788733045, -37.45808914225451502 ) ) ;
#29619 = VERTEX_POINT ( 'NONE', #3601 ) ;
#29620 = CARTESIAN_POINT ( 'NONE',  ( -37.46874999999995737, -115.9929510916434481, 13.11852480586264846 ) ) ;
#29621 = LINE ( 'NONE', #24925, #21119 ) ;
#29622 =( NAMED_UNIT ( * ) SI_UNIT ( $, .STERADIAN. ) SOLID_ANGLE_UNIT ( ) );
#29623 = CARTESIAN_POINT ( 'NONE',  ( -39.49999999999999289, -13.10640646055107084, 90.70096189432331357 ) ) ;
#29624 = CARTESIAN_POINT ( 'NONE',  ( -1.479000000000008752, 1.339905674773393496E-15, 6.984000000000015085 ) ) ;
#29625 = ORIENTED_EDGE ( 'NONE', *, *, #107, .T. ) ;
#29626 = CARTESIAN_POINT ( 'NONE',  ( -9.999999999999994671, 0.000000000000000000, 0.000000000000000000 ) ) ;
#29627 = CARTESIAN_POINT ( 'NONE',  ( -42.49999999999999289, -27.48076211353329157, 98.91941090707497608 ) ) ;
#29628 = EDGE_CURVE ( 'NONE', #35092, #11309, #11938, .T. ) ;
#29629 = AXIS2_PLACEMENT_3D ( 'NONE', #8569, #16305, #11455 ) ;
#29630 = DIRECTION ( 'NONE',  ( 0.000000000000000000, -1.000000000000000000, 0.000000000000000000 ) ) ;
#29631 = DIRECTION ( 'NONE',  ( -1.000000000000000000, 0.000000000000000000, 0.000000000000000000 ) ) ;
#29632 = DIRECTION ( 'NONE',  ( 0.000000000000000000, 0.000000000000000000, 1.000000000000000000 ) ) ;
#29633 = LINE ( 'NONE', #24231, #22269 ) ;
#29634 = CIRCLE ( 'NONE', #33616, 10.99999999999999645 ) ;
#29635 = ORIENTED_EDGE ( 'NONE', *, *, #1104, .F. ) ;
#29636 = ORIENTED_EDGE ( 'NONE', *, *, #23894, .F. ) ;
#29637 = VECTOR ( 'NONE', #16418, 1000.000000000000000 ) ;
#29638 = DIRECTION ( 'NONE',  ( -1.000000000000000000, 0.000000000000000000, 0.000000000000000000 ) ) ;
#29639 = DIRECTION ( 'NONE',  ( 0.000000000000000000, 0.000000000000000000, 1.000000000000000000 ) ) ;
#29640 = DIRECTION ( 'NONE',  ( -1.000000000000000000, 0.000000000000000000, 0.000000000000000000 ) ) ;
#29641 = ORIENTED_EDGE ( 'NONE', *, *, #35455, .T. ) ;
#29642 = CARTESIAN_POINT ( 'NONE',  ( -37.88768952767750875, -112.0245472910329880, 6.527725545821550845 ) ) ;
#29643 = EDGE_LOOP ( 'NONE', ( #26635, #16862, #22399, #29904 ) ) ;
#29644 = AXIS2_PLACEMENT_3D ( 'NONE', #26838, #18537, #15287 ) ;
#29645 = ORIENTED_EDGE ( 'NONE', *, *, #15666, .F. ) ;
#29646 = ORIENTED_EDGE ( 'NONE', *, *, #31673, .T. ) ;
#29647 = CARTESIAN_POINT ( 'NONE',  ( 8.000000000000000000, -11.11653975335780942, -12.74840161668743299 ) ) ;
#29648 = DIRECTION ( 'NONE',  ( 0.000000000000000000, 0.000000000000000000, 1.000000000000000000 ) ) ;
#29649 = ORIENTED_EDGE ( 'NONE', *, *, #304, .T. ) ;
#29650 = ORIENTED_EDGE ( 'NONE', *, *, #22256, .F. ) ;
#29651 = CARTESIAN_POINT ( 'NONE',  ( 7.999999999999992895, -44.61570720899105424, 14.73072383765550164 ) ) ;
#29652 = CARTESIAN_POINT ( 'NONE',  ( 3.799999999999999822, 4.382607293638566128E-16, -45.10000000000000142 ) ) ;
#29653 = CARTESIAN_POINT ( 'NONE',  ( -4.000000000000000000, -2.710505431213761085E-17, 45.99999999999998579 ) ) ;
#29654 = DIRECTION ( 'NONE',  ( 1.084202172485497655E-16, -6.938893903907204958E-17, -1.000000000000000000 ) ) ;
#29655 = DIRECTION ( 'NONE',  ( 0.000000000000000000, 0.000000000000000000, 1.000000000000000000 ) ) ;
#29656 = CARTESIAN_POINT ( 'NONE',  ( 1.600000000000004086, -12.74999999999999822, 0.000000000000000000 ) ) ;
#29657 = CARTESIAN_POINT ( 'NONE',  ( -38.45611840935523418, -115.3723087153909432, 6.566024454178448266 ) ) ;
#29658 = CARTESIAN_POINT ( 'NONE',  ( -34.50000000000000000, -115.9926080209513657, 10.46845107750242398 ) ) ;
#29659 = CARTESIAN_POINT ( 'NONE',  ( 46.00000000000000000, 1.347111479062088405E-15, 11.00000000000000000 ) ) ;
#29660 = CARTESIAN_POINT ( 'NONE',  ( 7.999999999999992895, -17.50309955389642269, 43.60271849949356948 ) ) ;
#29661 = AXIS2_PLACEMENT_3D ( 'NONE', #15594, #2142, #12748 ) ;
#29662 = CARTESIAN_POINT ( 'NONE',  ( -1.000000000000014655, -5.408326913195881325, -0.7999999999999951594 ) ) ;
#29663 = DIRECTION ( 'NONE',  ( 0.000000000000000000, -0.9510565162951565288, 0.3090169943749383474 ) ) ;
#29664 = ADVANCED_FACE ( 'NONE', ( #28433 ), #14735, .F. ) ;
#29665 = DIRECTION ( 'NONE',  ( -1.000000000000000000, 0.000000000000000000, 0.000000000000000000 ) ) ;
#29666 = SURFACE_SIDE_STYLE ('',( #1953 ) ) ;
#29667 = ORIENTED_EDGE ( 'NONE', *, *, #18035, .F. ) ;
#29668 = CARTESIAN_POINT ( 'NONE',  ( -40.02454729103296671, -112.8166217158120332, 9.340225545821551734 ) ) ;
#29669 = DIRECTION ( 'NONE',  ( 0.000000000000000000, 0.000000000000000000, 1.000000000000000000 ) ) ;
#29670 = DIRECTION ( 'NONE',  ( -1.000000000000000000, 0.000000000000000000, 0.000000000000000000 ) ) ;
#29671 = ORIENTED_EDGE ( 'NONE', *, *, #32332, .T. ) ;
#29672 = ORIENTED_EDGE ( 'NONE', *, *, #34184, .F. ) ;
#29673 = CARTESIAN_POINT ( 'NONE',  ( 0.000000000000000000, 0.000000000000000000, 55.00000000000000000 ) ) ;
#29674 = AXIS2_PLACEMENT_3D ( 'NONE', #34811, #21455, #9953 ) ;
#29675 = CARTESIAN_POINT ( 'NONE',  ( -9.999999999999994671, 0.000000000000000000, 0.000000000000000000 ) ) ;
#29676 = ORIENTED_EDGE ( 'NONE', *, *, #2985, .T. ) ;
#29677 = ADVANCED_FACE ( 'NONE', ( #12045 ), #9703, .T. ) ;
#29678 = EDGE_LOOP ( 'NONE', ( #14866, #34239, #3858, #13065 ) ) ;
#29679 = AXIS2_PLACEMENT_3D ( 'NONE', #28150, #25089, #14273 ) ;
#29680 = AXIS2_PLACEMENT_3D ( 'NONE', #16978, #11764, #20030 ) ;
#29681 = VECTOR ( 'NONE', #23323, 1000.000000000000000 ) ;
#29682 = DIRECTION ( 'NONE',  ( 0.000000000000000000, -1.000000000000000000, -2.423959199780483078E-15 ) ) ;
#29683 = CARTESIAN_POINT ( 'NONE',  ( 8.000000000000000000, 16.59870953437685515, -3.253005020243678214 ) ) ;
#29684 = DIRECTION ( 'NONE',  ( 1.000000000000000000, 0.000000000000000000, 0.000000000000000000 ) ) ;
#29685 = CYLINDRICAL_SURFACE ( 'NONE', #31703, 47.49900000000001654 ) ;
#29687 = VERTEX_POINT ( 'NONE', #20302 ) ;
#29686 = VECTOR ( 'NONE', #34714, 1000.000000000000000 ) ;
#29688 = EDGE_LOOP ( 'NONE', ( #8986, #8581, #28055, #11189 ) ) ;
#29689 = CARTESIAN_POINT ( 'NONE',  ( -35.50000000000000711, -112.0250551866464548, 1.025914454044489332 ) ) ;
#29690 = DIRECTION ( 'NONE',  ( -1.000000000000000000, -1.836970198721029934E-16, -0.000000000000000000 ) ) ;
#29691 = DIRECTION ( 'NONE',  ( 0.000000000000000000, 0.000000000000000000, 1.000000000000000000 ) ) ;
#29692 = EDGE_LOOP ( 'NONE', ( #19685, #13184, #28172, #4324 ) ) ;
#29693 = CYLINDRICAL_SURFACE ( 'NONE', #14336, 20.00000000000000355 ) ;
#29694 = EDGE_CURVE ( 'NONE', #33209, #17384, #28624, .T. ) ;
#29695 = AXIS2_PLACEMENT_3D ( 'NONE', #35467, #16170, #32932 ) ;
#29696 = CARTESIAN_POINT ( 'NONE',  ( -34.50000000000000000, -112.0140978167138712, -0.4685323525984295134 ) ) ;
#29697 = CARTESIAN_POINT ( 'NONE',  ( -34.50000000000000000, -114.9929510916434339, 10.59426868253284226 ) ) ;
#29698 = VECTOR ( 'NONE', #20525, 1000.000000000000000 ) ;
#29699 = LINE ( 'NONE', #27184, #32116 ) ;
#29700 = CARTESIAN_POINT ( 'NONE',  ( -35.50000000000000000, -113.9929510916435049, 10.50625754673586876 ) ) ;
#29701 = CARTESIAN_POINT ( 'NONE',  ( 7.999999999999992895, 0.000000000000000000, 0.000000000000000000 ) ) ;
#29702 = CARTESIAN_POINT ( 'NONE',  ( -39.00000000000000000, -113.9929510916434339, 12.39849696637031151 ) ) ;
#29703 = DIRECTION ( 'NONE',  ( -0.000000000000000000, 0.000000000000000000, -1.000000000000000000 ) ) ;
#29704 = AXIS2_PLACEMENT_3D ( 'NONE', #27758, #373, #3098 ) ;
#29705 = AXIS2_PLACEMENT_3D ( 'NONE', #21004, #2145, #24269 ) ;
#29706 = DIRECTION ( 'NONE',  ( 2.668805347656627171E-16, -1.000000000000000000, 0.000000000000000000 ) ) ;
#29707 = DIRECTION ( 'NONE',  ( 0.000000000000000000, 0.000000000000000000, 1.000000000000000000 ) ) ;
#29708 = ORIENTED_EDGE ( 'NONE', *, *, #17657, .T. ) ;
#29709 = AXIS2_PLACEMENT_3D ( 'NONE', #7478, #34864, #2285 ) ;
#29710 = CARTESIAN_POINT ( 'NONE',  ( 3.799999999999999822, -2.710505431213761085E-17, 45.99999999999998579 ) ) ;
#29711 = DIRECTION ( 'NONE',  ( -1.000000000000000000, -0.000000000000000000, -0.000000000000000000 ) ) ;
#29712 = EDGE_CURVE ( 'NONE', #7659, #9761, #35554, .T. ) ;
#29713 = ORIENTED_EDGE ( 'NONE', *, *, #7688, .T. ) ;
#29714 = ADVANCED_FACE ( 'NONE', ( #1247 ), #25563, .T. ) ;
#29715 = CARTESIAN_POINT ( 'NONE',  ( -38.00000000000000711, -114.9929510916434339, 12.53051367006571937 ) ) ;
#29716 = EDGE_LOOP ( 'NONE', ( #33895, #24112, #5985, #15128 ) ) ;
#29717 = ADVANCED_FACE ( 'NONE', ( #12230 ), #20484, .T. ) ;
#29718 = CARTESIAN_POINT ( 'NONE',  ( -37.76916472181487450, -111.9754527089670404, 5.534774454178449155 ) ) ;
#29719 = CARTESIAN_POINT ( 'NONE',  ( 3.160591952521676795, -3.281206521718066149, -0.7999999999999951594 ) ) ;
#29720 = AXIS2_PLACEMENT_3D ( 'NONE', #7860, #13628, #11279 ) ;
#29721 = ORIENTED_EDGE ( 'NONE', *, *, #4921, .F. ) ;
#29722 = ORIENTED_EDGE ( 'NONE', *, *, #35542, .T. ) ;
#29723 = DIRECTION ( 'NONE',  ( 0.000000000000000000, 1.000000000000000000, 0.000000000000000000 ) ) ;
#29724 = DIRECTION ( 'NONE',  ( 0.000000000000000000, 0.000000000000000000, 1.000000000000000000 ) ) ;
#29725 = EDGE_CURVE ( 'NONE', #27299, #5721, #26274, .T. ) ;
#29726 = ORIENTED_EDGE ( 'NONE', *, *, #30015, .F. ) ;
#29727 = CARTESIAN_POINT ( 'NONE',  ( -35.69809690994938478, -111.0245472910330022, 4.222274454178449155 ) ) ;
#29728 = EDGE_CURVE ( 'NONE', #34766, #35237, #20559, .T. ) ;
#29729 = CIRCLE ( 'NONE', #25715, 7.000000000000006217 ) ;
#29730 = DIRECTION ( 'NONE',  ( 0.000000000000000000, 0.000000000000000000, -1.000000000000000000 ) ) ;
#29731 = AXIS2_PLACEMENT_3D ( 'NONE', #14616, #14439, #22546 ) ;
#29732 = CARTESIAN_POINT ( 'NONE',  ( 0.000000000000000000, 9.744342220503382279, 46.48873837489803407 ) ) ;
#29733 = ORIENTED_EDGE ( 'NONE', *, *, #5363, .T. ) ;
#29734 = ORIENTED_EDGE ( 'NONE', *, *, #32420, .F. ) ;
#29735 = DIRECTION ( 'NONE',  ( 0.000000000000000000, 0.000000000000000000, 1.000000000000000000 ) ) ;
#29736 = AXIS2_PLACEMENT_3D ( 'NONE', #20417, #20242, #6760 ) ;
#29737 = CARTESIAN_POINT ( 'NONE',  ( -55.00000000000000000, 0.000000000000000000, 70.00000000000000000 ) ) ;
#29738 = ORIENTED_EDGE ( 'NONE', *, *, #8229, .T. ) ;
#29739 = ORIENTED_EDGE ( 'NONE', *, *, #29962, .F. ) ;
#29740 = CARTESIAN_POINT ( 'NONE',  ( -34.50000000000000000, -111.0687598768285369, 1.355111303971038073 ) ) ;
#29741 = AXIS2_PLACEMENT_3D ( 'NONE', #19204, #13466, #30204 ) ;
#29742 = STYLED_ITEM ( 'NONE', ( #9298 ), #34226 ) ;
#29743 = CYLINDRICAL_SURFACE ( 'NONE', #16186, 12.99999999999999822 ) ;
#29744 = ORIENTED_EDGE ( 'NONE', *, *, #7312, .F. ) ;
#29745 = AXIS2_PLACEMENT_3D ( 'NONE', #28302, #28665, #9030 ) ;
#29746 = CARTESIAN_POINT ( 'NONE',  ( -35.50000000000000711, -114.9927795562974069, 10.48735431211914815 ) ) ;
#29747 = EDGE_CURVE ( 'NONE', #24508, #31889, #12533, .T. ) ;
#29748 = CARTESIAN_POINT ( 'NONE',  ( -34.50000000000000000, -113.9929510916434339, 10.59426868253284226 ) ) ;
#29749 = CARTESIAN_POINT ( 'NONE',  ( -34.50000000000000000, -116.0140978167138712, 0.8752176474015622709 ) ) ;
#29750 = DIRECTION ( 'NONE',  ( -1.000000000000000000, 0.000000000000000000, 0.000000000000000000 ) ) ;
#29751 = CARTESIAN_POINT ( 'NONE',  ( -34.50000000000000000, -113.9929510916434339, 10.50625754673586876 ) ) ;
#29752 = CARTESIAN_POINT ( 'NONE',  ( -37.54084996655477369, -115.9929510916434481, 13.11692036158760466 ) ) ;
#29753 = AXIS2_PLACEMENT_3D ( 'NONE', #25142, #22589, #28196 ) ;
#29754 = DIRECTION ( 'NONE',  ( -1.000000000000000000, 0.000000000000000000, 0.000000000000000000 ) ) ;
#29755 = CARTESIAN_POINT ( 'NONE',  ( 7.999999999999992895, -41.20225022064655462, 23.63323037071389621 ) ) ;
#29756 = CIRCLE ( 'NONE', #1017, 17.49900000000001299 ) ;
#29757 = EDGE_CURVE ( 'NONE', #31746, #17882, #13116, .T. ) ;
#29758 = EDGE_CURVE ( 'NONE', #6633, #18320, #10225, .T. ) ;
#29759 = ORIENTED_EDGE ( 'NONE', *, *, #2370, .T. ) ;
#29760 = EDGE_CURVE ( 'NONE', #4678, #6546, #22874, .T. ) ;
#29761 = DIRECTION ( 'NONE',  ( 0.000000000000000000, 0.000000000000000000, 1.000000000000000000 ) ) ;
#29762 = DIRECTION ( 'NONE',  ( 0.000000000000000000, 0.000000000000000000, 1.000000000000000000 ) ) ;
#29763 = CYLINDRICAL_SURFACE ( 'NONE', #13987, 20.00000000000000355 ) ;
#29764 = CIRCLE ( 'NONE', #23429, 8.000000000000000000 ) ;
#29765 = ORIENTED_EDGE ( 'NONE', *, *, #1753, .F. ) ;
#29766 = CIRCLE ( 'NONE', #25726, 8.000000000000007105 ) ;
#29767 = DIRECTION ( 'NONE',  ( -1.000000000000000000, 0.000000000000000000, 0.000000000000000000 ) ) ;
#29768 = CARTESIAN_POINT ( 'NONE',  ( -35.50000000000000000, -113.0140978167138712, -0.1247823525984260717 ) ) ;
#29769 = DIRECTION ( 'NONE',  ( -1.000000000000000000, 0.000000000000000000, -0.000000000000000000 ) ) ;
#29770 = CIRCLE ( 'NONE', #6745, 7.199999999999993072 ) ;
#29771 = AXIS2_PLACEMENT_3D ( 'NONE', #7833, #26949, #21334 ) ;
#29772 = CARTESIAN_POINT ( 'NONE',  ( -35.50000000000000711, -114.9928438774171582, 10.49113435197128652 ) ) ;
#29773 = LINE ( 'NONE', #2413, #20504 ) ;
#29774 = EDGE_CURVE ( 'NONE', #13787, #27224, #21718, .T. ) ;
#29775 = EDGE_LOOP ( 'NONE', ( #2745, #130, #13750, #25278 ) ) ;
#29776 = FACE_OUTER_BOUND ( 'NONE', #21206, .T. ) ;
#29777 = CARTESIAN_POINT ( 'NONE',  ( -35.50000000000000000, -112.8690837874180062, 2.872105769100646189 ) ) ;
#29778 = ORIENTED_EDGE ( 'NONE', *, *, #12817, .T. ) ;
#29779 = ORIENTED_EDGE ( 'NONE', *, *, #33690, .F. ) ;
#29780 = CARTESIAN_POINT ( 'NONE',  ( -35.97545270896702618, -113.6450488405582604, 5.909774454178450931 ) ) ;
#29781 =( LENGTH_UNIT ( ) NAMED_UNIT ( * ) SI_UNIT ( .MILLI., .METRE. ) );
#29782 = AXIS2_PLACEMENT_3D ( 'NONE', #28327, #3674, #600 ) ;
#29783 = DIRECTION ( 'NONE',  ( -1.000000000000000000, 0.000000000000000000, 0.000000000000000000 ) ) ;
#29784 = VERTEX_POINT ( 'NONE', #2163 ) ;
#29785 = VERTEX_POINT ( 'NONE', #15976 ) ;
#29786 = CARTESIAN_POINT ( 'NONE',  ( -34.50000000000000000, -113.0140978167138712, -0.6247823525979733228 ) ) ;
#29787 = DIRECTION ( 'NONE',  ( -1.000000000000000000, 0.000000000000000000, 0.000000000000000000 ) ) ;
#29788 = CIRCLE ( 'NONE', #7276, 3.799999999999999822 ) ;
#29789 = VECTOR ( 'NONE', #7548, 1000.000000000000000 ) ;
#29790 = CARTESIAN_POINT ( 'NONE',  ( 8.000000000000007105, -0.3151488735047419665, 11.27190672109269798 ) ) ;
#29791 = CIRCLE ( 'NONE', #2206, 14.70000000000000107 ) ;
#29792 = ADVANCED_FACE ( 'NONE', ( #26993 ), #9872, .T. ) ;
#29793 = CARTESIAN_POINT ( 'NONE',  ( -4.000000000000000000, 0.000000000000000000, 60.90000000000001279 ) ) ;
#29794 = CIRCLE ( 'NONE', #15391, 19.99999999999998579 ) ;
#29795 = CARTESIAN_POINT ( 'NONE',  ( -35.50000000000000000, -113.9697269463297431, 10.50348536859153370 ) ) ;
#29796 = ADVANCED_FACE ( 'NONE', ( #18337 ), #4509, .T. ) ;
#29797 = CARTESIAN_POINT ( 'NONE',  ( -90.00000000000002842, 0.000000000000000000, 6.938893903907228378E-15 ) ) ;
#29798 = CARTESIAN_POINT ( 'NONE',  ( 8.000000000000000000, 11.19999565274250308, 10.71350075272077973 ) ) ;
#29799 = CARTESIAN_POINT ( 'NONE',  ( -34.50000000000000000, -112.0221129971568104, -0.7553032835231431319 ) ) ;
#29800 = FACE_OUTER_BOUND ( 'NONE', #31382, .T. ) ;
#29801 = ADVANCED_FACE ( 'NONE', ( #2338 ), #29335, .T. ) ;
#29802 = DIRECTION ( 'NONE',  ( 0.000000000000000000, 0.000000000000000000, 1.000000000000000000 ) ) ;
#29803 = ORIENTED_EDGE ( 'NONE', *, *, #34012, .F. ) ;
#29804 = CARTESIAN_POINT ( 'NONE',  ( -37.54084996655477369, -115.9929510916434481, 13.11692036158760466 ) ) ;
#29805 = LINE ( 'NONE', #13411, #34960 ) ;
#29806 = DIRECTION ( 'NONE',  ( -1.000000000000000000, -0.000000000000000000, -0.000000000000000000 ) ) ;
#29807 = EDGE_CURVE ( 'NONE', #26196, #8972, #21021, .T. ) ;
#29808 = CARTESIAN_POINT ( 'NONE',  ( 112.0000000000000000, 81.48267994499606459, 30.15054357219658954 ) ) ;
#29809 = LINE ( 'NONE', #13586, #28012 ) ;
#29810 = ORIENTED_EDGE ( 'NONE', *, *, #14610, .F. ) ;
#29811 = CARTESIAN_POINT ( 'NONE',  ( 0.000000000000000000, 49.25004636492388954, 16.68630974939777545 ) ) ;
#29812 = CARTESIAN_POINT ( 'NONE',  ( 0.000000000000000000, 6.109652351742432153, -46.58570277113502556 ) ) ;
#29813 = DIRECTION ( 'NONE',  ( 0.000000000000000000, 0.000000000000000000, 1.000000000000000000 ) ) ;
#29814 = CARTESIAN_POINT ( 'NONE',  ( 50.00005079999999680, 0.000000000000000000, 4.000000000000000000 ) ) ;
#29815 = AXIS2_PLACEMENT_3D ( 'NONE', #21037, #4157, #20320 ) ;
#29816 = AXIS2_PLACEMENT_3D ( 'NONE', #24610, #25310, #3177 ) ;
#29817 = LINE ( 'NONE', #5155, #6073 ) ;
#29818 = DIRECTION ( 'NONE',  ( 1.000000000000000000, 0.000000000000000000, 0.000000000000000000 ) ) ;
#29819 = ORIENTED_EDGE ( 'NONE', *, *, #4605, .T. ) ;
#29820 = ORIENTED_EDGE ( 'NONE', *, *, #5934, .T. ) ;
#29821 = AXIS2_PLACEMENT_3D ( 'NONE', #9666, #20263, #3926 ) ;
#29822 = DIRECTION ( 'NONE',  ( 0.000000000000000000, 0.000000000000000000, 1.000000000000000000 ) ) ;
#29823 = DIRECTION ( 'NONE',  ( -1.000000000000000000, 0.000000000000000000, 0.000000000000000000 ) ) ;
#29824 = DIRECTION ( 'NONE',  ( -0.000000000000000000, 0.000000000000000000, -1.000000000000000000 ) ) ;
#29825 = ORIENTED_EDGE ( 'NONE', *, *, #32604, .F. ) ;
#29826 = CARTESIAN_POINT ( 'NONE',  ( -35.00000000000000000, -113.9407375970686900, 8.496475545821551734 ) ) ;
#29827 = ORIENTED_EDGE ( 'NONE', *, *, #28035, .T. ) ;
#29828 = AXIS2_PLACEMENT_3D ( 'NONE', #1922, #15392, #6584 ) ;
#29829 = ORIENTED_EDGE ( 'NONE', *, *, #16524, .F. ) ;
#29830 = VERTEX_POINT ( 'NONE', #31839 ) ;
#29831 = DIRECTION ( 'NONE',  ( 0.000000000000000000, 0.000000000000000000, 1.000000000000000000 ) ) ;
#29832 = EDGE_CURVE ( 'NONE', #14042, #4708, #15386, .T. ) ;
#29833 = FACE_BOUND ( 'NONE', #28155, .T. ) ;
#29834 = VERTEX_POINT ( 'NONE', #29512 ) ;
#29835 = VERTEX_POINT ( 'NONE', #29866 ) ;
#29836 = EDGE_CURVE ( 'NONE', #20467, #8283, #1788, .T. ) ;
#29837 = CARTESIAN_POINT ( 'NONE',  ( 8.000000000000000000, 0.000000000000000000, 0.000000000000000000 ) ) ;
#29838 = LINE ( 'NONE', #32515, #8024 ) ;
#29839 = AXIS2_PLACEMENT_3D ( 'NONE', #13492, #1984, #29532 ) ;
#29840 = CARTESIAN_POINT ( 'NONE',  ( 0.000000000000000000, 0.000000000000000000, 0.000000000000000000 ) ) ;
#29841 = CIRCLE ( 'NONE', #19463, 4.000000000000003553 ) ;
#29842 = CYLINDRICAL_SURFACE ( 'NONE', #5067, 22.00000000000000000 ) ;
#29843 = DIRECTION ( 'NONE',  ( -1.000000000000000000, 0.000000000000000000, 0.000000000000000000 ) ) ;
#29844 = CIRCLE ( 'NONE', #26972, 0.1999999999999998723 ) ;
#29845 = CARTESIAN_POINT ( 'NONE',  ( -34.97545270896703329, -113.2308352781851397, 4.409774454178448266 ) ) ;
#29846 = CARTESIAN_POINT ( 'NONE',  ( -37.56132887387857267, -115.9929510916434481, 14.11732072679899197 ) ) ;
#29847 = DIRECTION ( 'NONE',  ( -1.000000000000000000, 0.000000000000000000, 0.000000000000000000 ) ) ;
#29848 = DIRECTION ( 'NONE',  ( -1.783119874454246424E-31, -1.187911941725854497E-31, 1.000000000000000000 ) ) ;
#29849 = CARTESIAN_POINT ( 'NONE',  ( 4.121423858225409909, -12.61643262889541894, 0.000000000000000000 ) ) ;
#29850 = LINE ( 'NONE', #32717, #33065 ) ;
#29851 = DIRECTION ( 'NONE',  ( 0.000000000000000000, 0.000000000000000000, -1.000000000000000000 ) ) ;
#29852 = SURFACE_SIDE_STYLE ('',( #35427 ) ) ;
#29853 = VERTEX_POINT ( 'NONE', #26810 ) ;
#29854 = CARTESIAN_POINT ( 'NONE',  ( -37.88768952767750875, -112.0245472910329880, 3.527725545821551290 ) ) ;
#29855 = CARTESIAN_POINT ( 'NONE',  ( -42.49999999999999289, -14.67619866229190784, 76.74125644078590369 ) ) ;
#29856 = DIRECTION ( 'NONE',  ( 0.000000000000000000, -1.000000000000000000, -1.048062100069320848E-14 ) ) ;
#29857 = DIRECTION ( 'NONE',  ( -1.000000000000000000, -0.000000000000000000, -0.000000000000000000 ) ) ;
#29858 = EDGE_LOOP ( 'NONE', ( #31552, #30483, #22488, #14678 ) ) ;
#29859 = CARTESIAN_POINT ( 'NONE',  ( -34.50000000000000000, -113.1291422947505936, 0.8889500704178361357 ) ) ;
#29860 = EDGE_LOOP ( 'NONE', ( #18237, #22510, #5599, #34341 ) ) ;
#29861 = DIRECTION ( 'NONE',  ( -1.000000000000000000, -0.000000000000000000, -0.000000000000000000 ) ) ;
#29862 = ORIENTED_EDGE ( 'NONE', *, *, #14845, .F. ) ;
#29863 = AXIS2_PLACEMENT_3D ( 'NONE', #20803, #10213, #34344 ) ;
#29864 = ORIENTED_EDGE ( 'NONE', *, *, #26194, .T. ) ;
#29865 = AXIS2_PLACEMENT_3D ( 'NONE', #12285, #26521, #31719 ) ;
#29866 = CARTESIAN_POINT ( 'NONE',  ( 0.000000000000000000, 2.912696353506125657, -21.80633394113447210 ) ) ;
#29867 = FACE_OUTER_BOUND ( 'NONE', #16761, .T. ) ;
#29868 = DIRECTION ( 'NONE',  ( 1.000000000000000000, 0.000000000000000000, 0.000000000000000000 ) ) ;
#29869 = DIRECTION ( 'NONE',  ( -1.000000000000000000, -0.000000000000000000, -0.000000000000000000 ) ) ;
#29870 = EDGE_LOOP ( 'NONE', ( #20213, #14208, #14897, #23882 ) ) ;
#29871 = ORIENTED_EDGE ( 'NONE', *, *, #8821, .T. ) ;
#29872 = CARTESIAN_POINT ( 'NONE',  ( -35.50000000000000711, -112.0140978167138712, 0.3752176474015640473 ) ) ;
#29873 = EDGE_CURVE ( 'NONE', #17998, #18878, #32092, .T. ) ;
#29874 = CARTESIAN_POINT ( 'NONE',  ( -22.99999999999999645, 3.857637417314163478E-15, 0.000000000000000000 ) ) ;
#29875 = FACE_OUTER_BOUND ( 'NONE', #10907, .T. ) ;
#29876 = VERTEX_POINT ( 'NONE', #29159 ) ;
#29877 = CARTESIAN_POINT ( 'NONE',  ( 7.999999999999992895, -11.90021268425586953, 45.45261810511210143 ) ) ;
#29878 = CARTESIAN_POINT ( 'NONE',  ( -34.50000000000000000, -116.0140978167138712, -0.5622823525984409487 ) ) ;
#29879 = CARTESIAN_POINT ( 'NONE',  ( -38.42182118622945808, -114.9929510916434339, 13.81802396319329773 ) ) ;
#29880 = DIRECTION ( 'NONE',  ( 0.000000000000000000, 0.000000000000000000, 1.000000000000000000 ) ) ;
#29881 = CARTESIAN_POINT ( 'NONE',  ( -35.50000000000000000, -113.9929510916434623, 10.50625754673586876 ) ) ;
#29882 = CARTESIAN_POINT ( 'NONE',  ( 7.999999999999992895, -18.53613841426824393, 48.58406706613897796 ) ) ;
#29883 = EDGE_CURVE ( 'NONE', #22477, #33707, #25780, .T. ) ;
#29884 = CARTESIAN_POINT ( 'NONE',  ( -39.00000000000000000, -113.9929510916434339, 12.44250253426875119 ) ) ;
#29885 = CARTESIAN_POINT ( 'NONE',  ( -55.00000000000000000, -2.726571689596996976E-14, 114.0000000000000000 ) ) ;
#29886 = CARTESIAN_POINT ( 'NONE',  ( 0.000000000000000000, 0.000000000000000000, 0.000000000000000000 ) ) ;
#29887 = DIRECTION ( 'NONE',  ( -1.000000000000000000, -0.000000000000000000, 0.000000000000000000 ) ) ;
#29888 = ORIENTED_EDGE ( 'NONE', *, *, #9779, .T. ) ;
#29889 = CIRCLE ( 'NONE', #5175, 3.799999999999999822 ) ;
#29890 = CARTESIAN_POINT ( 'NONE',  ( 0.000000000000000000, 0.000000000000000000, -30.00000000000000000 ) ) ;
#29891 = DIRECTION ( 'NONE',  ( 0.000000000000000000, 0.3090169943749415116, 0.9510565162951555296 ) ) ;
#29892 = ORIENTED_EDGE ( 'NONE', *, *, #22271, .T. ) ;
#29893 = CARTESIAN_POINT ( 'NONE',  ( -37.46874999999996447, -114.9929510916434339, 13.11852480586264669 ) ) ;
#29894 = VERTEX_POINT ( 'NONE', #15611 ) ;
#29895 = AXIS2_PLACEMENT_3D ( 'NONE', #19469, #17953, #33161 ) ;
#29896 = AXIS2_PLACEMENT_3D ( 'NONE', #4145, #20131, #17969 ) ;
#29897 = CARTESIAN_POINT ( 'NONE',  ( -36.11231047232249125, -112.0245472910329880, 4.222274454178449155 ) ) ;
#29898 = CIRCLE ( 'NONE', #16657, 52.00000000000000711 ) ;
#29899 = CARTESIAN_POINT ( 'NONE',  ( 0.000000000000000000, 0.000000000000000000, 50.00000000000000000 ) ) ;
#29900 = EDGE_LOOP ( 'NONE', ( #5425, #19125, #31297, #13874 ) ) ;
#29901 = EDGE_LOOP ( 'NONE', ( #5852, #27035, #20441, #19851 ) ) ;
#29902 = DIRECTION ( 'NONE',  ( -1.000000000000000000, 0.000000000000000000, 0.000000000000000000 ) ) ;
#29903 = PLANE ( 'NONE',  #23792 ) ;
#29904 = ORIENTED_EDGE ( 'NONE', *, *, #17830, .F. ) ;
#29905 = CARTESIAN_POINT ( 'NONE',  ( -39.07941549657749647, -116.1632251905417803, 3.058975545821551734 ) ) ;
#29906 = LINE ( 'NONE', #5074, #18234 ) ;
#29907 = LINE ( 'NONE', #21426, #6182 ) ;
#29908 = ORIENTED_EDGE ( 'NONE', *, *, #8000, .F. ) ;
#29909 = ORIENTED_EDGE ( 'NONE', *, *, #6858, .F. ) ;
#29910 = CARTESIAN_POINT ( 'NONE',  ( 70.00001200000001234, -23.52257523363354252, 81.80133263040720237 ) ) ;
#29911 =( LENGTH_UNIT ( ) NAMED_UNIT ( * ) SI_UNIT ( .MILLI., .METRE. ) );
#29912 = CARTESIAN_POINT ( 'NONE',  ( 5.400000000000085620, -1.000000000000049516, -40.00000000000000000 ) ) ;
#29913 = ORIENTED_EDGE ( 'NONE', *, *, #28698, .T. ) ;
#29914 = ORIENTED_EDGE ( 'NONE', *, *, #11439, .F. ) ;
#29915 = AXIS2_PLACEMENT_3D ( 'NONE', #20986, #31990, #15579 ) ;
#29916 = CARTESIAN_POINT ( 'NONE',  ( -34.50000000000000000, -111.2666036476567655, -1.632210088999287212 ) ) ;
#29917 = EDGE_CURVE ( 'NONE', #11373, #21654, #10251, .T. ) ;
#29918 = ADVANCED_FACE ( 'NONE', ( #15441 ), #35103, .T. ) ;
#29919 = CARTESIAN_POINT ( 'NONE',  ( 8.000000000000000000, 18.62763138773856397, -2.494040418455147456 ) ) ;
#29920 = CIRCLE ( 'NONE', #20681, 20.00000000000000355 ) ;
#29921 = PRODUCT_DEFINITION_FORMATION_WITH_SPECIFIED_SOURCE ( 'ANY', '', #7526, .NOT_KNOWN. ) ;
#29922 = ORIENTED_EDGE ( 'NONE', *, *, #4443, .T. ) ;
#29923 = CARTESIAN_POINT ( 'NONE',  ( -35.50000000000000711, -114.9929510916434339, 10.55026311463432087 ) ) ;
#29924 = CARTESIAN_POINT ( 'NONE',  ( -35.24442919769867899, -113.9929510916434339, 13.92914543265605509 ) ) ;
#29925 = DIRECTION ( 'NONE',  ( -1.000000000000000000, -0.000000000000000000, 0.000000000000000000 ) ) ;
#29926 = DIRECTION ( 'NONE',  ( -1.000000000000000000, -0.000000000000000000, 0.000000000000000000 ) ) ;
#29927 = ADVANCED_FACE ( 'NONE', ( #32377 ), #7698, .T. ) ;
#29928 = CARTESIAN_POINT ( 'NONE',  ( -37.49414064056232831, -113.9929510916434339, 13.11852578240983291 ) ) ;
#29929 = CARTESIAN_POINT ( 'NONE',  ( -38.00000000000000711, -115.9929510916434481, 12.57451923796417681 ) ) ;
#29930 = CARTESIAN_POINT ( 'NONE',  ( 8.000000000000007105, 10.15474465512070168, -9.637487275700989287 ) ) ;
#29931 = LINE ( 'NONE', #15329, #4901 ) ;
#29932 = EDGE_LOOP ( 'NONE', ( #8168, #7839 ) ) ;
#29933 = VECTOR ( 'NONE', #35198, 1000.000000000000000 ) ;
#29934 = DIRECTION ( 'NONE',  ( 0.000000000000000000, 0.9848077530122092416, -0.1736481776669233923 ) ) ;
#29935 = CYLINDRICAL_SURFACE ( 'NONE', #5360, 47.49900000000001654 ) ;
#29936 = CARTESIAN_POINT ( 'NONE',  ( 8.000000000000000000, 16.71027810728549667, 2.620268201066223934 ) ) ;
#29937 = ORIENTED_EDGE ( 'NONE', *, *, #16250, .F. ) ;
#29938 = AXIS2_PLACEMENT_3D ( 'NONE', #26435, #10405, #15593 ) ;
#29939 = CARTESIAN_POINT ( 'NONE',  ( 7.999999999999992895, 17.50309955389674954, -43.60271849949345579 ) ) ;
#29940 = ORIENTED_EDGE ( 'NONE', *, *, #17437, .F. ) ;
#29941 = CARTESIAN_POINT ( 'NONE',  ( -35.50000000000000000, -114.1185248058627053, 1.007048908356900085 ) ) ;
#29942 = DIRECTION ( 'NONE',  ( -1.000000000000000000, -0.000000000000000000, -0.000000000000000000 ) ) ;
#29943 = VECTOR ( 'NONE', #12126, 1000.000000000000000 ) ;
#29944 = AXIS2_PLACEMENT_3D ( 'NONE', #11346, #10991, #16559 ) ;
#29945 = CARTESIAN_POINT ( 'NONE',  ( -35.50000000000000711, -114.9929510916434339, 12.39849696637031506 ) ) ;
#29946 = CYLINDRICAL_SURFACE ( 'NONE', #3292, 7.020000000000045759 ) ;
#29947 = EDGE_CURVE ( 'NONE', #17998, #28739, #13474, .T. ) ;
#29948 = ORIENTED_EDGE ( 'NONE', *, *, #22069, .T. ) ;
#29949 = DIRECTION ( 'NONE',  ( 0.000000000000000000, 0.000000000000000000, 1.000000000000000000 ) ) ;
#29950 = CARTESIAN_POINT ( 'NONE',  ( -35.50000000000000000, -111.2666036476567655, -1.632210088999287212 ) ) ;
#29951 = ORIENTED_EDGE ( 'NONE', *, *, #21374, .T. ) ;
#29952 = ORIENTED_EDGE ( 'NONE', *, *, #7967, .F. ) ;
#29953 = CARTESIAN_POINT ( 'NONE',  ( -37.35495115944176092, -112.9754527089670688, 5.534774454178449155 ) ) ;
#29954 =( NAMED_UNIT ( * ) SI_UNIT ( $, .STERADIAN. ) SOLID_ANGLE_UNIT ( ) );
#29955 = CARTESIAN_POINT ( 'NONE',  ( 8.000000000000000000, -6.085920226790910270, -15.78165944574524637 ) ) ;
#29956 = ORIENTED_EDGE ( 'NONE', *, *, #30477, .T. ) ;
#29957 = ORIENTED_EDGE ( 'NONE', *, *, #9748, .T. ) ;
#29958 = CARTESIAN_POINT ( 'NONE',  ( -34.50000000000000000, -113.0140978167141128, -0.6247823525984907977 ) ) ;
#29959 = DIRECTION ( 'NONE',  ( -1.000000000000000000, -0.000000000000000000, -0.000000000000000000 ) ) ;
#29960 = EDGE_CURVE ( 'NONE', #22165, #2676, #10588, .T. ) ;
#29961 = EDGE_CURVE ( 'NONE', #15563, #33313, #31831, .T. ) ;
#29962 = EDGE_CURVE ( 'NONE', #26423, #25092, #24388, .T. ) ;
#29963 = FACE_BOUND ( 'NONE', #1827, .T. ) ;
#29964 = CARTESIAN_POINT ( 'NONE',  ( 65.00000000000001421, -36.26296008782259861, 84.27446239413865214 ) ) ;
#29965 = CARTESIAN_POINT ( 'NONE',  ( -37.58145695302688694, -114.9929510916434339, 13.11211614918362756 ) ) ;
#29966 = DIRECTION ( 'NONE',  ( -0.000000000000000000, 0.000000000000000000, -1.000000000000000000 ) ) ;
#29967 = DIRECTION ( 'NONE',  ( -1.000000000000000000, 0.000000000000000000, -0.000000000000000000 ) ) ;
#29968 = EDGE_CURVE ( 'NONE', #10771, #18371, #3033, .T. ) ;
#29969 = AXIS2_PLACEMENT_3D ( 'NONE', #2941, #7780, #19287 ) ;
#29970 = CIRCLE ( 'NONE', #1775, 47.49900000000001654 ) ;
#29971 = CARTESIAN_POINT ( 'NONE',  ( -34.50000000000000000, -114.8057644833805568, -1.624782352598427959 ) ) ;
#29972 = ADVANCED_FACE ( 'NONE', ( #24637, #11472 ), #30395, .T. ) ;
#29973 = MECHANICAL_DESIGN_GEOMETRIC_PRESENTATION_REPRESENTATION (  '', ( #20740 ), #22468 ) ;
#29974 = CARTESIAN_POINT ( 'NONE',  ( -34.50015059926905536, -115.9929510916434481, 12.64306614848962518 ) ) ;
#29975 = DIRECTION ( 'NONE',  ( -1.000000000000000000, 0.000000000000000000, 0.000000000000000000 ) ) ;
#29976 = CARTESIAN_POINT ( 'NONE',  ( 7.999999999999992895, -47.22458491092817212, -5.098390039074724100 ) ) ;
#29977 = ORIENTED_EDGE ( 'NONE', *, *, #5135, .T. ) ;
#29978 = CARTESIAN_POINT ( 'NONE',  ( -37.99959864031216483, -115.9929510916434481, 12.63896776382213538 ) ) ;
#29979 = CARTESIAN_POINT ( 'NONE',  ( 7.999999999999992895, -32.32520163883559405, -34.09746168776067776 ) ) ;
#29980 = DIRECTION ( 'NONE',  ( 0.000000000000000000, 0.000000000000000000, -1.000000000000000000 ) ) ;
#29981 = ITEM_DEFINED_TRANSFORMATION ( 'NONE', 'NONE', #32256,  #21307 ) ;
#29982 = DIRECTION ( 'NONE',  ( 0.000000000000000000, 0.000000000000000000, 1.000000000000000000 ) ) ;
#29983 = ORIENTED_EDGE ( 'NONE', *, *, #18957, .F. ) ;
#29984 = CARTESIAN_POINT ( 'NONE',  ( 4.000000000000000000, 4.898587196589412829E-16, 35.10000000000000142 ) ) ;
#29985 = DIRECTION ( 'NONE',  ( 0.000000000000000000, -0.6427876096865295930, -0.7660444431189862291 ) ) ;
#29986 = CARTESIAN_POINT ( 'NONE',  ( 50.00000000000000000, 0.000000000000000000, 70.00000000000000000 ) ) ;
#29987 = DIRECTION ( 'NONE',  ( -1.000000000000000000, 0.000000000000000000, 0.000000000000000000 ) ) ;
#29988 = VECTOR ( 'NONE', #35418, 1000.000000000000000 ) ;
#29989 = LINE ( 'NONE', #10537, #31370 ) ;
#29990 = CARTESIAN_POINT ( 'NONE',  ( -1.000000000000014655, -5.408326913195881325, 0.000000000000000000 ) ) ;
#29991 = EDGE_CURVE ( 'NONE', #19897, #10552, #135, .T. ) ;
#29992 = EDGE_LOOP ( 'NONE', ( #8461, #24321, #28797, #33653 ) ) ;
#29993 = ORIENTED_EDGE ( 'NONE', *, *, #827, .T. ) ;
#29994 = DIRECTION ( 'NONE',  ( 0.000000000000000000, -0.5877852522924797984, 0.8090169943749425663 ) ) ;
#29995 = CYLINDRICAL_SURFACE ( 'NONE', #30913, 52.00000000000000711 ) ;
#29996 = EDGE_CURVE ( 'NONE', #16003, #2539, #20892, .T. ) ;
#29997 = DIRECTION ( 'NONE',  ( 1.000000000000000000, 0.000000000000000000, 0.000000000000000000 ) ) ;
#29998 = ORIENTED_EDGE ( 'NONE', *, *, #20089, .F. ) ;
#29999 = CARTESIAN_POINT ( 'NONE',  ( -35.00000000000000000, -113.9407375970686900, 5.496475545821551734 ) ) ;
#30000 = EDGE_LOOP ( 'NONE', ( #15578, #23800, #6906, #17079 ) ) ;
#30001 = ADVANCED_FACE ( 'NONE', ( #24986 ), #28389, .T. ) ;
#30002 =( GEOMETRIC_REPRESENTATION_CONTEXT ( 3 ) GLOBAL_UNCERTAINTY_ASSIGNED_CONTEXT ( ( #14977 ) ) GLOBAL_UNIT_ASSIGNED_CONTEXT ( ( #27787, #14075, #55 ) ) REPRESENTATION_CONTEXT ( 'NONE', 'WORKASPACE' ) );
#30003 = VECTOR ( 'NONE', #29869, 1000.000000000000000 ) ;
#30004 = ORIENTED_EDGE ( 'NONE', *, *, #8645, .F. ) ;
#30005 = VERTEX_POINT ( 'NONE', #11303 ) ;
#30006 = DIRECTION ( 'NONE',  ( 1.000000000000000000, 0.000000000000000000, 0.000000000000000000 ) ) ;
#30007 = ADVANCED_FACE ( 'NONE', ( #22441 ), #309, .T. ) ;
#30008 = ADVANCED_FACE ( 'NONE', ( #17036 ), #16325, .T. ) ;
#30009 = DIRECTION ( 'NONE',  ( 1.174092375852885330E-15, 4.222049128630153888E-16, 1.000000000000000000 ) ) ;
#30010 = ORIENTED_EDGE ( 'NONE', *, *, #3606, .T. ) ;
#30011 = ORIENTED_EDGE ( 'NONE', *, *, #33674, .F. ) ;
#30012 = DIRECTION ( 'NONE',  ( -1.000000000000000000, 0.000000000000000000, 0.000000000000000000 ) ) ;
#30013 = CARTESIAN_POINT ( 'NONE',  ( 0.000000000000000000, 47.49120266317496686, -0.8606222198176971538 ) ) ;
#30014 = DIRECTION ( 'NONE',  ( -1.000000000000000000, -0.000000000000000000, -0.000000000000000000 ) ) ;
#30015 = EDGE_CURVE ( 'NONE', #33645, #864, #22065, .T. ) ;
#30016 = CARTESIAN_POINT ( 'NONE',  ( 4.000000000000003553, -51.85248208264515313, -3.914090171286743747 ) ) ;
#30017 = DIRECTION ( 'NONE',  ( 0.000000000000000000, 1.000000000000000000, 3.614007241618346010E-15 ) ) ;
#30018 = CARTESIAN_POINT ( 'NONE',  ( 0.000000000000000000, -17.08890430202781374, 43.76671000081938701 ) ) ;
#30019 = AXIS2_PLACEMENT_3D ( 'NONE', #24160, #20720, #18569 ) ;
#30020 = CARTESIAN_POINT ( 'NONE',  ( -35.93867112612154102, -115.9929510916434481, 14.11732072679899197 ) ) ;
#30022 = CARTESIAN_POINT ( 'NONE',  ( 8.000000000000000000, -19.60123832284014966, -3.973846525876632008 ) ) ;
#30021 = CIRCLE ( 'NONE', #5303, 7.020000000000045759 ) ;
#30023 = CARTESIAN_POINT ( 'NONE',  ( 0.000000000000000000, -11.27190672109268377, 0.3151488735047419665 ) ) ;
#30024 = DIRECTION ( 'NONE',  ( 0.000000000000000000, -0.9848077530122096857, 0.1736481776669208388 ) ) ;
#30025 = DIRECTION ( 'NONE',  ( -1.000000000000000000, 0.000000000000000000, 0.000000000000000000 ) ) ;
#30026 = CYLINDRICAL_SURFACE ( 'NONE', #30272, 7.199999999999994849 ) ;
#30027 = CARTESIAN_POINT ( 'NONE',  ( 4.000000000000003553, -25.61928775981012762, -45.25098998563503727 ) ) ;
#30028 = ORIENTED_EDGE ( 'NONE', *, *, #11492, .T. ) ;
#30029 = CARTESIAN_POINT ( 'NONE',  ( -38.45611840935523418, -112.6276912846090568, 9.433975545821551734 ) ) ;
#30030 = DIRECTION ( 'NONE',  ( 0.000000000000000000, -1.000000000000000000, 0.000000000000000000 ) ) ;
#30031 = CARTESIAN_POINT ( 'NONE',  ( 8.000000000000007105, -5.908880290975456973, -9.604183132802479150 ) ) ;
#30032 = DIRECTION ( 'NONE',  ( 1.000000000000000000, -0.000000000000000000, 0.000000000000000000 ) ) ;
#30033 = ADVANCED_FACE ( 'NONE', ( #22272 ), #21738, .T. ) ;
#30034 = ORIENTED_EDGE ( 'NONE', *, *, #14848, .T. ) ;
#30035 = PRESENTATION_LAYER_ASSIGNMENT (  '', '', ( #28866 ) ) ;
#30036 = VERTEX_POINT ( 'NONE', #32732 ) ;
#30037 = EDGE_CURVE ( 'NONE', #26487, #13043, #26185, .T. ) ;
#30038 = FILL_AREA_STYLE ('',( #10589 ) ) ;
#30039 = DIRECTION ( 'NONE',  ( -1.000000000000000000, 0.000000000000000000, 0.000000000000000000 ) ) ;
#30040 = ORIENTED_EDGE ( 'NONE', *, *, #28436, .F. ) ;
#30041 = EDGE_LOOP ( 'NONE', ( #9865, #30048, #20927, #12585 ) ) ;
#30042 = FACE_OUTER_BOUND ( 'NONE', #19607, .T. ) ;
#30043 = TOROIDAL_SURFACE ( 'NONE', #12224, 6.983999999999990216, 0.04099999999999958539 ) ;
#30044 = LINE ( 'NONE', #19396, #6211 ) ;
#30045 = ADVANCED_FACE ( 'NONE', ( #30042 ), #16859, .T. ) ;
#30046 = APPLICATION_PROTOCOL_DEFINITION ( 'draft international standard', 'automotive_design', 1998, #17894 ) ;
#30047 = CARTESIAN_POINT ( 'NONE',  ( -6.938893903907228378E-15, 0.7408941433508786645, 0.000000000000000000 ) ) ;
#30048 = ORIENTED_EDGE ( 'NONE', *, *, #17857, .F. ) ;
#30049 = ORIENTED_EDGE ( 'NONE', *, *, #21370, .T. ) ;
#30050 = CARTESIAN_POINT ( 'NONE',  ( 8.000000000000000000, 0.000000000000000000, 0.000000000000000000 ) ) ;
#30051 = FACE_OUTER_BOUND ( 'NONE', #1269, .T. ) ;
#30052 = VERTEX_POINT ( 'NONE', #26452 ) ;
#30053 = CARTESIAN_POINT ( 'NONE',  ( -46.00000000000000000, 0.000000000000000000, 81.00000000000001421 ) ) ;
#30054 = CARTESIAN_POINT ( 'NONE',  ( -34.50000000000000000, -116.0140978167138712, -0.3747823525984422255 ) ) ;
#30055 = CARTESIAN_POINT ( 'NONE',  ( -37.42187499999997158, -114.9929510916434339, 14.11852480586264846 ) ) ;
#30056 = CARTESIAN_POINT ( 'NONE',  ( 7.999999999999992895, -19.74581912682874929, 48.10512059033388255 ) ) ;
#30057 = CARTESIAN_POINT ( 'NONE',  ( -38.00000000000000711, -114.9929510916434339, 12.44250253426874941 ) ) ;
#30058 = CARTESIAN_POINT ( 'NONE',  ( -21.15833593587365513, -21.76666049839546346, 85.70096189432329936 ) ) ;
#30059 = CARTESIAN_POINT ( 'NONE',  ( -36.07812499999994316, -114.9929510916434339, 14.11852480586264846 ) ) ;
#30060 = CARTESIAN_POINT ( 'NONE',  ( 50.00000000000000000, 0.000000000000000000, 0.000000000000000000 ) ) ;
#30061 = CARTESIAN_POINT ( 'NONE',  ( 4.000000000000000000, -12.46108038583323285, 15.64357617738992801 ) ) ;
#30062 = SURFACE_STYLE_FILL_AREA ( #3897 ) ;
#30063 = DIRECTION ( 'NONE',  ( 0.000000000000000000, -0.9822872507286865007, -0.1873813145857356477 ) ) ;
#30064 = DIRECTION ( 'NONE',  ( 0.000000000000000000, 0.000000000000000000, 1.000000000000000000 ) ) ;
#30065 = CARTESIAN_POINT ( 'NONE',  ( 0.000000000000000000, 5.363026430117226795, 9.919332006307262972 ) ) ;
#30066 = VECTOR ( 'NONE', #33727, 1000.000000000000000 ) ;
#30067 = ORIENTED_EDGE ( 'NONE', *, *, #14799, .F. ) ;
#30068 = DIRECTION ( 'NONE',  ( 0.000000000000000000, 0.000000000000000000, 1.000000000000000000 ) ) ;
#30069 = VERTEX_POINT ( 'NONE', #14168 ) ;
#30070 = CARTESIAN_POINT ( 'NONE',  ( -34.97545270896703329, -113.2308352781851539, 5.909774454178449155 ) ) ;
#30071 = FACE_OUTER_BOUND ( 'NONE', #12824, .T. ) ;
#30072 = ORIENTED_EDGE ( 'NONE', *, *, #9901, .T. ) ;
#30073 = ORIENTED_EDGE ( 'NONE', *, *, #35286, .T. ) ;
#30074 = EDGE_CURVE ( 'NONE', #10171, #26362, #8920, .T. ) ;
#30075 = CARTESIAN_POINT ( 'NONE',  ( -34.49999999999998579, -15.39406523420381490, 87.83669687932935233 ) ) ;
#30076 = DIRECTION ( 'NONE',  ( -1.000000000000000000, 0.000000000000000000, 0.000000000000000000 ) ) ;
#30077 = ORIENTED_EDGE ( 'NONE', *, *, #4761, .T. ) ;
#30078 = CARTESIAN_POINT ( 'NONE',  ( -34.83677480945821259, -116.0794154965774965, 2.683975545821551734 ) ) ;
#30079 = AXIS2_PLACEMENT_3D ( 'NONE', #17867, #28862, #34996 ) ;
#30080 = CARTESIAN_POINT ( 'NONE',  ( 7.999999999999992895, -43.83938735307256707, -18.28286404005846677 ) ) ;
#30081 = CARTESIAN_POINT ( 'NONE',  ( -9.999999999999994671, 0.000000000000000000, 0.000000000000000000 ) ) ;
#30083 = ORIENTED_EDGE ( 'NONE', *, *, #22742, .T. ) ;
#30082 = VECTOR ( 'NONE', #11950, 1000.000000000000000 ) ;
#30084 = ORIENTED_EDGE ( 'NONE', *, *, #18799, .F. ) ;
#30085 = VECTOR ( 'NONE', #112, 1000.000000000000000 ) ;
#30086 = DIRECTION ( 'NONE',  ( -0.000000000000000000, 1.000000000000000000, 0.000000000000000000 ) ) ;
#30087 = DIRECTION ( 'NONE',  ( -1.000000000000000000, 0.000000000000000000, 0.000000000000000000 ) ) ;
#30088 = ORIENTED_EDGE ( 'NONE', *, *, #35025, .T. ) ;
#30089 = ORIENTED_EDGE ( 'NONE', *, *, #954, .T. ) ;
#30090 = CARTESIAN_POINT ( 'NONE',  ( -34.50000000000000000, -111.0168437565048691, 0.9961850632443862708 ) ) ;
#30091 = AXIS2_PLACEMENT_3D ( 'NONE', #14583, #27931, #30985 ) ;
#30092 = CIRCLE ( 'NONE', #13406, 10.99999999999999822 ) ;
#30093 = CARTESIAN_POINT ( 'NONE',  ( -44.00000000000000000, 0.000000000000000000, 0.000000000000000000 ) ) ;
#30094 = ORIENTED_EDGE ( 'NONE', *, *, #2663, .F. ) ;
#30095 = CARTESIAN_POINT ( 'NONE',  ( -35.50000000000000711, -114.9929510916434339, 10.53376102667243508 ) ) ;
#30096 = CARTESIAN_POINT ( 'NONE',  ( -34.50000000000000000, -113.9929510916434339, 11.73841344789270202 ) ) ;
#30097 = LINE ( 'NONE', #5091, #30975 ) ;
#30098 = CARTESIAN_POINT ( 'NONE',  ( -3.799999999999999822, 4.653657836759942730E-16, -55.89999999999999858 ) ) ;
#30099 = CARTESIAN_POINT ( 'NONE',  ( -34.54793860109200665, -113.9929510916434339, 13.00730889637958221 ) ) ;
#30100 = CARTESIAN_POINT ( 'NONE',  ( -37.98325232167028531, -114.9929510916434339, 14.04194344061727406 ) ) ;
#30101 = CARTESIAN_POINT ( 'NONE',  ( -35.50000000000000711, -114.1414532730574507, 9.517316564499758158 ) ) ;
#30102 = DIRECTION ( 'NONE',  ( 0.000000000000000000, 0.000000000000000000, 1.000000000000000000 ) ) ;
#30103 = VECTOR ( 'NONE', #11826, 999.9999999999998863 ) ;
#30104 = CARTESIAN_POINT ( 'NONE',  ( 50.00005079999998969, 0.000000000000000000, 0.000000000000000000 ) ) ;
#30105 = ORIENTED_EDGE ( 'NONE', *, *, #1005, .T. ) ;
#30106 = LINE ( 'NONE', #13728, #14339 ) ;
#30107 = DIRECTION ( 'NONE',  ( -1.000000000000000000, 0.000000000000000000, 0.000000000000000000 ) ) ;
#30108 = DIRECTION ( 'NONE',  ( 1.000000000000000000, -0.000000000000000000, 0.000000000000000000 ) ) ;
#30109 = ORIENTED_EDGE ( 'NONE', *, *, #19236, .F. ) ;
#30110 = CARTESIAN_POINT ( 'NONE',  ( 8.000000000000000000, 5.400000000000000355, 0.000000000000000000 ) ) ;
#30111 = ORIENTED_EDGE ( 'NONE', *, *, #1180, .T. ) ;
#30112 = EDGE_CURVE ( 'NONE', #2115, #24515, #32118, .T. ) ;
#30113 = AXIS2_PLACEMENT_3D ( 'NONE', #8562, #16483, #19533 ) ;
#30114 = CARTESIAN_POINT ( 'NONE',  ( -35.50000000000000711, -116.0140978167138712, 0.8752176474015622709 ) ) ;
#30115 = CYLINDRICAL_SURFACE ( 'NONE', #32252, 3.799999999999999822 ) ;
#30116 = ADVANCED_FACE ( 'NONE', ( #3732 ), #14685, .T. ) ;
#30117 = CARTESIAN_POINT ( 'NONE',  ( -36.25098837183129774, -113.3347980657956242, 4.316024454178448266 ) ) ;
#30118 = VECTOR ( 'NONE', #23454, 1000.000000000000000 ) ;
#30119 = CARTESIAN_POINT ( 'NONE',  ( -35.50005019975638021, -114.9929510916434339, 12.62670525340498529 ) ) ;
#30120 = LINE ( 'NONE', #30299, #32609 ) ;
#30121 = ORIENTED_EDGE ( 'NONE', *, *, #30171, .T. ) ;
#30122 = CARTESIAN_POINT ( 'NONE',  ( -35.50000000000000000, -111.0301281775997353, -0.8858242144478579716 ) ) ;
#30123 = EDGE_LOOP ( 'NONE', ( #27351, #26989 ) ) ;
#30124 = ORIENTED_EDGE ( 'NONE', *, *, #20118, .F. ) ;
#30125 = CARTESIAN_POINT ( 'NONE',  ( -36.02454729103298092, -114.4734759653044307, 7.597274454178449155 ) ) ;
#30126 = EDGE_CURVE ( 'NONE', #18547, #34626, #28220, .T. ) ;
#30127 = SURFACE_STYLE_FILL_AREA ( #21650 ) ;
#30128 = CARTESIAN_POINT ( 'NONE',  ( 50.00005079999999680, 3.872983346207429900, 1.000000000000003109 ) ) ;
#30129 = VERTEX_POINT ( 'NONE', #31930 ) ;
#30130 = ORIENTED_EDGE ( 'NONE', *, *, #15823, .F. ) ;
#30131 = CARTESIAN_POINT ( 'NONE',  ( -34.50000000000000000, -113.0140978167140702, 0.8752176474015694874 ) ) ;
#30132 = CARTESIAN_POINT ( 'NONE',  ( 4.000000000000000000, 4.898587196589412829E-16, 55.00000000000000000 ) ) ;
#30133 = CARTESIAN_POINT ( 'NONE',  ( 50.00005079999999680, 5.400000000000000355, -0.9999999999999985567 ) ) ;
#30134 = CARTESIAN_POINT ( 'NONE',  ( 0.000000000000000000, 0.000000000000000000, 36.00000000000000000 ) ) ;
#30135 = AXIS2_PLACEMENT_3D ( 'NONE', #2157, #35438, #27334 ) ;
#30136 = CARTESIAN_POINT ( 'NONE',  ( -35.50000000000000000, -113.9929510916434339, 12.56351784598954424 ) ) ;
#30137 = VECTOR ( 'NONE', #23856, 1000.000000000000000 ) ;
#30138 = DIRECTION ( 'NONE',  ( -1.000000000000000000, 0.000000000000000000, 0.000000000000000000 ) ) ;
#30139 = CARTESIAN_POINT ( 'NONE',  ( 7.999999999999992895, 0.000000000000000000, -1.000000000000000888 ) ) ;
#30140 = CARTESIAN_POINT ( 'NONE',  ( -34.50000000000000000, -113.0557643173828524, -1.624792769101735868 ) ) ;
#30141 = EDGE_CURVE ( 'NONE', #13559, #8148, #20084, .T. ) ;
#30142 = CARTESIAN_POINT ( 'NONE',  ( -38.99879592093640213, -115.9929510916434481, 12.67985367974111277 ) ) ;
#30143 = UNCERTAINTY_MEASURE_WITH_UNIT (LENGTH_MEASURE( 1.000000000000000082E-05 ), #17750, 'distance_accuracy_value', 'NONE');
#30144 = CARTESIAN_POINT ( 'NONE',  ( 0.9999999999999870104, -5.408326913195881325, -0.7999999999999951594 ) ) ;
#30145 = ADVANCED_BREP_SHAPE_REPRESENTATION ( '', ( #22365, #21307 ), #12169 ) ;
#30146 = CARTESIAN_POINT ( 'NONE',  ( 0.000000000000000000, 0.000000000000000000, 0.000000000000000000 ) ) ;
#30147 = ORIENTED_EDGE ( 'NONE', *, *, #2752, .T. ) ;
#30148 = CARTESIAN_POINT ( 'NONE',  ( -37.53269373325071712, -115.9929510916434481, 13.11752178341324360 ) ) ;
#30149 = FACE_OUTER_BOUND ( 'NONE', #707, .T. ) ;
#30150 = CARTESIAN_POINT ( 'NONE',  ( 8.000000000000000000, 17.56975900509189970, -9.555290079479078713 ) ) ;
#30151 = CARTESIAN_POINT ( 'NONE',  ( 0.000000000000000000, -26.17370628620627215, -39.63700417846191471 ) ) ;
#30152 = FACE_OUTER_BOUND ( 'NONE', #1293, .T. ) ;
#30153 = ORIENTED_EDGE ( 'NONE', *, *, #631, .F. ) ;
#30154 = CARTESIAN_POINT ( 'NONE',  ( 0.000000000000000000, -2.710505431213761085E-17, 55.00000000000000000 ) ) ;
#30155 = DIRECTION ( 'NONE',  ( 0.000000000000000000, 0.000000000000000000, -1.000000000000000000 ) ) ;
#30156 = ADVANCED_FACE ( 'NONE', ( #15530 ), #28390, .T. ) ;
#30157 = LINE ( 'NONE', #13776, #32603 ) ;
#30158 = CARTESIAN_POINT ( 'NONE',  ( 50.00000000000000711, 6.123233995736780087E-16, 5.000000000000011546 ) ) ;
#30159 = ADVANCED_FACE ( 'NONE', ( #4770 ), #23838, .T. ) ;
#30160 = EDGE_CURVE ( 'NONE', #6684, #32280, #6610, .T. ) ;
#30161 = CARTESIAN_POINT ( 'NONE',  ( -3.799999999999999822, 4.653657836759942730E-16, 50.00000000000000000 ) ) ;
#30162 = FACE_OUTER_BOUND ( 'NONE', #4674, .T. ) ;
#30163 = ORIENTED_EDGE ( 'NONE', *, *, #34394, .F. ) ;
#30164 = AXIS2_PLACEMENT_3D ( 'NONE', #33833, #22480, #30253 ) ;
#30165 = FACE_OUTER_BOUND ( 'NONE', #19541, .T. ) ;
#30166 = AXIS2_PLACEMENT_3D ( 'NONE', #16352, #32408, #35473 ) ;
#30167 = CARTESIAN_POINT ( 'NONE',  ( -21.15833593587365513, -31.68172400785665488, 97.87435565298206086 ) ) ;
#30168 = DIRECTION ( 'NONE',  ( -1.000000000000000000, -1.836970198721029934E-16, -0.000000000000000000 ) ) ;
#30169 = VERTEX_POINT ( 'NONE', #30916 ) ;
#30170 = CARTESIAN_POINT ( 'NONE',  ( -35.62769128460905677, -112.5438815906447729, 5.308975545821551734 ) ) ;
#30171 = EDGE_CURVE ( 'NONE', #3309, #1992, #25703, .T. ) ;
#30172 = ORIENTED_EDGE ( 'NONE', *, *, #34838, .T. ) ;
#30173 = EDGE_CURVE ( 'NONE', #14501, #28112, #15799, .T. ) ;
#30174 = CIRCLE ( 'NONE', #13005, 8.000000000000008882 ) ;
#30175 = ORIENTED_EDGE ( 'NONE', *, *, #19613, .T. ) ;
#30176 = EDGE_LOOP ( 'NONE', ( #22849, #13128, #13224, #27336 ) ) ;
#30177 = CARTESIAN_POINT ( 'NONE',  ( -21.15833593587365513, -39.98076211353324538, 86.49999999999991473 ) ) ;
#30178 = PLANE ( 'NONE',  #28291 ) ;
#30179 = EDGE_LOOP ( 'NONE', ( #22932, #1109, #5238, #6152 ) ) ;
#30180 = CARTESIAN_POINT ( 'NONE',  ( -35.50000000000000711, -114.0000000000003411, 9.500000000000035527 ) ) ;
#30181 = DIRECTION ( 'NONE',  ( 0.000000000000000000, -1.000000000000000000, 0.000000000000000000 ) ) ;
#30182 = DIRECTION ( 'NONE',  ( 0.000000000000000000, 0.000000000000000000, 1.000000000000000000 ) ) ;
#30183 = EDGE_CURVE ( 'NONE', #584, #20267, #11637, .T. ) ;
#30184 = DIRECTION ( 'NONE',  ( -1.000000000000000000, 0.000000000000000000, 0.000000000000000000 ) ) ;
#30185 = CARTESIAN_POINT ( 'NONE',  ( 6.071532165918824830E-15, 1.000000000000000000, -22.00000000000000000 ) ) ;
#30186 = VECTOR ( 'NONE', #7653, 1000.000000000000000 ) ;
#30187 = VECTOR ( 'NONE', #15242, 1000.000000000000000 ) ;
#30188 = PRODUCT_DEFINITION ( 'UNKNOWN', '', #24728, #22016 ) ;
#30189 = CARTESIAN_POINT ( 'NONE',  ( 0.000000000000000000, 14.71414642875970635, -9.471478019454975694 ) ) ;
#30190 = CARTESIAN_POINT ( 'NONE',  ( -35.75562914091914024, -115.9929510916434481, 14.09929883582542409 ) ) ;
#30191 = CARTESIAN_POINT ( 'NONE',  ( 7.999999999999992895, 15.49408907645234734, -44.90087086784577508 ) ) ;
#30192 = CIRCLE ( 'NONE', #14644, 3.799999999999999822 ) ;
#30193 = CARTESIAN_POINT ( 'NONE',  ( 0.000000000000000000, -3.753907720749058541, 8.725776631572749409 ) ) ;
#30194 = FACE_OUTER_BOUND ( 'NONE', #6865, .T. ) ;
#30195 = CARTESIAN_POINT ( 'NONE',  ( -34.49999999999998579, -28.69486372867102020, 88.29903810567654432 ) ) ;
#30196 = AXIS2_PLACEMENT_3D ( 'NONE', #24554, #2786, #33004 ) ;
#30197 = DIRECTION ( 'NONE',  ( -1.000000000000000000, 0.000000000000000000, 0.000000000000000000 ) ) ;
#30198 = ORIENTED_EDGE ( 'NONE', *, *, #22659, .T. ) ;
#30199 = EDGE_CURVE ( 'NONE', #14563, #33633, #7206, .T. ) ;
#30200 = EDGE_CURVE ( 'NONE', #3813, #25880, #293, .T. ) ;
#30201 = CARTESIAN_POINT ( 'NONE',  ( -38.99999999999999289, -114.0592624029313242, 9.246475545821551734 ) ) ;
#30202 = DIRECTION ( 'NONE',  ( 1.000000000000000000, 0.000000000000000000, 0.000000000000000000 ) ) ;
#30203 = DIRECTION ( 'NONE',  ( 1.000000000000000000, 0.000000000000000000, 0.000000000000000000 ) ) ;
#30204 = DIRECTION ( 'NONE',  ( 0.000000000000000000, 0.2486898871648483555, 0.9685831611286328524 ) ) ;
#30205 = ORIENTED_EDGE ( 'NONE', *, *, #19670, .F. ) ;
#30206 = VECTOR ( 'NONE', #30627, 1000.000000000000000 ) ;
#30207 = ORIENTED_EDGE ( 'NONE', *, *, #1143, .T. ) ;
#30208 = DIRECTION ( 'NONE',  ( -1.000000000000000000, 0.000000000000000000, 0.000000000000000000 ) ) ;
#30209 = DIRECTION ( 'NONE',  ( 0.000000000000000000, -0.9929510916431035783, 0.1185248058626076212 ) ) ;
#30210 = ORIENTED_EDGE ( 'NONE', *, *, #27073, .T. ) ;
#30211 = VERTEX_POINT ( 'NONE', #6591 ) ;
#30212 = EDGE_CURVE ( 'NONE', #24774, #9394, #6054, .T. ) ;
#30213 = AXIS2_PLACEMENT_3D ( 'NONE', #9281, #30583, #2714 ) ;
#30214 = DIRECTION ( 'NONE',  ( 0.000000000000000000, 0.000000000000000000, -1.000000000000000000 ) ) ;
#30215 = AXIS2_PLACEMENT_3D ( 'NONE', #1364, #23503, #20778 ) ;
#30216 = DIRECTION ( 'NONE',  ( 1.000000000000000000, -0.000000000000000000, 0.000000000000000000 ) ) ;
#30217 = EDGE_CURVE ( 'NONE', #9536, #27440, #32496, .T. ) ;
#30218 = CARTESIAN_POINT ( 'NONE',  ( 50.00000000000000000, 10.00000000000000888, 120.0000000000000000 ) ) ;
#30219 = ORIENTED_EDGE ( 'NONE', *, *, #28565, .F. ) ;
#30220 = ORIENTED_EDGE ( 'NONE', *, *, #19171, .F. ) ;
#30221 = CIRCLE ( 'NONE', #23316, 7.199999999999992184 ) ;
#30222 = DIRECTION ( 'NONE',  ( -1.000000000000000000, -0.000000000000000000, -0.000000000000000000 ) ) ;
#30223 = CARTESIAN_POINT ( 'NONE',  ( 7.999999999999992895, 12.30077720129095731, 50.52416135122086871 ) ) ;
#30224 = VERTEX_POINT ( 'NONE', #33799 ) ;
#30225 = FACE_OUTER_BOUND ( 'NONE', #9135, .T. ) ;
#30226 = ADVANCED_FACE ( 'NONE', ( #12861, #9125 ), #14873, .T. ) ;
#30227 = VECTOR ( 'NONE', #31521, 1000.000000000000000 ) ;
#30228 = CARTESIAN_POINT ( 'NONE',  ( -34.50000000000000000, -113.0974311500471714, -1.624782352598427959 ) ) ;
#30229 = EDGE_CURVE ( 'NONE', #28288, #19816, #10150, .T. ) ;
#30230 = CARTESIAN_POINT ( 'NONE',  ( -38.99924736195578134, -114.9929510916434339, 12.66759465831984777 ) ) ;
#30231 = EDGE_CURVE ( 'NONE', #31659, #20295, #16955, .T. ) ;
#30232 = CARTESIAN_POINT ( 'NONE',  ( -35.50000000000000000, -113.9929510916434339, 10.50625754673577994 ) ) ;
#30233 = CARTESIAN_POINT ( 'NONE',  ( 0.000000000000000000, 13.61301047812926690, 3.268936481846202113 ) ) ;
#30234 = CARTESIAN_POINT ( 'NONE',  ( -35.80421860361284558, -114.9929510916434339, 14.10650203519841916 ) ) ;
#30235 = FACE_OUTER_BOUND ( 'NONE', #25914, .T. ) ;
#30236 = CARTESIAN_POINT ( 'NONE',  ( 0.000000000000000000, 0.000000000000000000, 0.000000000000000000 ) ) ;
#30237 = CARTESIAN_POINT ( 'NONE',  ( -23.00000000000000000, 13.00000000000000533, 1.592040838891559293E-15 ) ) ;
#30238 = CYLINDRICAL_SURFACE ( 'NONE', #2665, 3.799999999999999822 ) ;
#30239 = DIRECTION ( 'NONE',  ( 0.000000000000000000, -1.000000000000000000, 0.000000000000000000 ) ) ;
#30240 = VECTOR ( 'NONE', #12887, 1000.000000000000000 ) ;
#30241 = VERTEX_POINT ( 'NONE', #13042 ) ;
#30242 = CARTESIAN_POINT ( 'NONE',  ( -38.00000000000000711, -114.9929510916434339, 10.85830208992306822 ) ) ;
#30243 = ORIENTED_EDGE ( 'NONE', *, *, #264, .F. ) ;
#30244 = EDGE_CURVE ( 'NONE', #32535, #12307, #10872, .T. ) ;
#30245 = CARTESIAN_POINT ( 'NONE',  ( -35.69809690994938478, -111.0245472910330022, 7.222274454178449155 ) ) ;
#30246 = EDGE_CURVE ( 'NONE', #20111, #8462, #20393, .T. ) ;
#30247 = FACE_OUTER_BOUND ( 'NONE', #19036, .T. ) ;
#30248 = CIRCLE ( 'NONE', #2092, 45.00000000000000000 ) ;
#30249 = VERTEX_POINT ( 'NONE', #8318 ) ;
#30250 = ORIENTED_EDGE ( 'NONE', *, *, #7135, .F. ) ;
#30251 = CIRCLE ( 'NONE', #22661, 5.000000000000011546 ) ;
#30252 = CARTESIAN_POINT ( 'NONE',  ( -4.121423858225413461, -12.61643262889540473, -1.200000000000006617 ) ) ;
#30253 = DIRECTION ( 'NONE',  ( 1.000000000000000000, -4.528031003192420052E-15, -1.174092375852883160E-15 ) ) ;
#30254 = ORIENTED_EDGE ( 'NONE', *, *, #33323, .T. ) ;
#30255 = CARTESIAN_POINT ( 'NONE',  ( -38.18337828418795965, -110.9754527089670546, 8.534774454178448266 ) ) ;
#30256 = VECTOR ( 'NONE', #6444, 1000.000000000000000 ) ;
#30257 = DIRECTION ( 'NONE',  ( -1.000000000000000000, -0.000000000000000000, 0.000000000000000000 ) ) ;
#30258 = FACE_OUTER_BOUND ( 'NONE', #18563, .T. ) ;
#30259 = ORIENTED_EDGE ( 'NONE', *, *, #25481, .T. ) ;
#30260 = ORIENTED_EDGE ( 'NONE', *, *, #31984, .T. ) ;
#30261 = CARTESIAN_POINT ( 'NONE',  ( 8.000000000000000000, 19.60123832284022782, -3.973846525876241653 ) ) ;
#30262 =( NAMED_UNIT ( * ) PLANE_ANGLE_UNIT ( ) SI_UNIT ( $, .RADIAN. ) );
#30263 = CYLINDRICAL_SURFACE ( 'NONE', #21885, 0.9999999999999974465 ) ;
#30264 = EDGE_LOOP ( 'NONE', ( #17151, #22702 ) ) ;
#30265 = EDGE_LOOP ( 'NONE', ( #11210, #4680, #9895, #3563 ) ) ;
#30266 = CARTESIAN_POINT ( 'NONE',  ( -34.50000000000000000, -117.0140814545088688, -0.6738694770610542673 ) ) ;
#30267 = AXIS2_PLACEMENT_3D ( 'NONE', #28507, #3861, #1149 ) ;
#30268 = FACE_OUTER_BOUND ( 'NONE', #2887, .T. ) ;
#30269 = ORIENTED_EDGE ( 'NONE', *, *, #14284, .T. ) ;
#30270 = CARTESIAN_POINT ( 'NONE',  ( -36.03125000000004263, -114.9929510916434339, 13.11852480586264669 ) ) ;
#30271 = AXIS2_PLACEMENT_3D ( 'NONE', #726, #25049, #21983 ) ;
#30272 = AXIS2_PLACEMENT_3D ( 'NONE', #121, #22422, #21902 ) ;
#30273 = ADVANCED_FACE ( 'NONE', ( #18604 ), #2067, .T. ) ;
#30274 = CIRCLE ( 'NONE', #26264, 8.000000000000007105 ) ;
#30275 = EDGE_CURVE ( 'NONE', #3989, #26766, #3750, .T. ) ;
#30276 = CARTESIAN_POINT ( 'NONE',  ( -34.80050084267116972, -113.9929510916434339, 13.54034599209289347 ) ) ;
#30277 = CYLINDRICAL_SURFACE ( 'NONE', #18900, 6.765000000000044977 ) ;
#30278 = CARTESIAN_POINT ( 'NONE',  ( 5.400000000000003020, 1.000000000000000888, -30.00000000000000000 ) ) ;
#30279 = CARTESIAN_POINT ( 'NONE',  ( -34.50000000000000000, -113.9929510916434339, 10.50625754673588474 ) ) ;
#30280 = CARTESIAN_POINT ( 'NONE',  ( 7.999999999999992895, 44.25018368420744252, 27.31155879685197263 ) ) ;
#30281 = AXIS2_PLACEMENT_3D ( 'NONE', #22350, #27943, #6502 ) ;
#30282 = CARTESIAN_POINT ( 'NONE',  ( -35.50000000000000711, -114.9929510916434339, 10.68227981832981044 ) ) ;
#30283 = CIRCLE ( 'NONE', #34314, 4.800000000000000711 ) ;
#30284 = FILL_AREA_STYLE_COLOUR ( '', #12451 ) ;
#30285 = SHAPE_REPRESENTATION ( 'circlip for shafts normal_din_Circlip DIN 471 - 22 x 1.2', ( #21307 ), #24211 ) ;
#30286 = CARTESIAN_POINT ( 'NONE',  ( 50.00000000000000000, 0.000000000000000000, 70.00000000000000000 ) ) ;
#30287 = ORIENTED_EDGE ( 'NONE', *, *, #35203, .T. ) ;
#30288 = EDGE_LOOP ( 'NONE', ( #3161, #32155, #17674, #18902 ) ) ;
#30289 = DIRECTION ( 'NONE',  ( 0.000000000000000000, 0.000000000000000000, -1.000000000000000000 ) ) ;
#30290 = DIRECTION ( 'NONE',  ( 0.000000000000000000, 0.000000000000000000, 1.000000000000000000 ) ) ;
#30291 = CIRCLE ( 'NONE', #21627, 4.000000000000000000 ) ;
#30292 = ORIENTED_EDGE ( 'NONE', *, *, #26220, .F. ) ;
#30293 = CARTESIAN_POINT ( 'NONE',  ( 3.799999999999999378, -1.702292157117525034E-14, -0.7999999999999907185 ) ) ;
#30294 = EDGE_LOOP ( 'NONE', ( #20889, #31525, #25422, #27391 ) ) ;
#30295 = AXIS2_PLACEMENT_3D ( 'NONE', #17825, #28825, #9910 ) ;
#30296 = CARTESIAN_POINT ( 'NONE',  ( -35.50000000000000711, -116.0060826362711595, -0.7553032835231661135 ) ) ;
#30297 = PLANE ( 'NONE',  #19574 ) ;
#30298 = CARTESIAN_POINT ( 'NONE',  ( -36.33479806579561000, -114.7490116281687165, 4.691024454178447378 ) ) ;
#30299 = CARTESIAN_POINT ( 'NONE',  ( 4.000000000000003553, -51.19683565102439360, -9.104066087303991139 ) ) ;
#30300 = ORIENTED_EDGE ( 'NONE', *, *, #25173, .F. ) ;
#30301 = AXIS2_PLACEMENT_3D ( 'NONE', #20921, #10136, #4585 ) ;
#30302 = DIRECTION ( 'NONE',  ( 1.000000000000000000, -0.000000000000000000, -0.000000000000000000 ) ) ;
#30303 = CARTESIAN_POINT ( 'NONE',  ( -35.50000000000000000, -116.6134300264884445, -1.853877267570539944 ) ) ;
#30304 = EDGE_LOOP ( 'NONE', ( #30524, #22898, #24412, #7747 ) ) ;
#30305 = ORIENTED_EDGE ( 'NONE', *, *, #26594, .T. ) ;
#30306 = AXIS2_PLACEMENT_3D ( 'NONE', #11277, #22249, #21719 ) ;
#30307 = CARTESIAN_POINT ( 'NONE',  ( -35.54388159064475872, -112.6276912846090568, 4.316024454178448266 ) ) ;
#30308 = PRESENTATION_STYLE_ASSIGNMENT (( #3477 ) ) ;
#30309 = VECTOR ( 'NONE', #9814, 1000.000000000000114 ) ;
#30310 = FACE_OUTER_BOUND ( 'NONE', #3108, .T. ) ;
#30311 = ORIENTED_EDGE ( 'NONE', *, *, #27164, .T. ) ;
#30312 = VERTEX_POINT ( 'NONE', #7614 ) ;
#30313 = CARTESIAN_POINT ( 'NONE',  ( -34.50000000000000000, -112.0140978167138712, 0.7189676474015718188 ) ) ;
#30314 = CARTESIAN_POINT ( 'NONE',  ( -9.999999999999994671, 0.000000000000000000, 0.000000000000000000 ) ) ;
#30315 = DIRECTION ( 'NONE',  ( 0.000000000000000000, 0.000000000000000000, 1.000000000000000000 ) ) ;
#30316 = DIRECTION ( 'NONE',  ( 1.000000000000000000, 1.836970198721029934E-16, 0.000000000000000000 ) ) ;
#30317 = AXIS2_PLACEMENT_3D ( 'NONE', #28595, #3946, #25544 ) ;
#30318 = EDGE_CURVE ( 'NONE', #4713, #19206, #15232, .T. ) ;
#30319 = VECTOR ( 'NONE', #32902, 1000.000000000000000 ) ;
#30320 = CARTESIAN_POINT ( 'NONE',  ( -35.50000000000000000, -113.9929510916434339, 10.52826033068511435 ) ) ;
#30321 = FACE_OUTER_BOUND ( 'NONE', #4556, .T. ) ;
#30322 = LINE ( 'NONE', #24915, #4477 ) ;
#30323 = CARTESIAN_POINT ( 'NONE',  ( -34.50000000000000000, -111.0140978167138570, 0.7502176474015694874 ) ) ;
#30324 = VECTOR ( 'NONE', #17578, 1000.000000000000000 ) ;
#30325 = CARTESIAN_POINT ( 'NONE',  ( -35.50000000000000000, -114.2356323198232673, 8.521029492159460261 ) ) ;
#30326 = FACE_OUTER_BOUND ( 'NONE', #28136, .T. ) ;
#30327 = AXIS2_PLACEMENT_3D ( 'NONE', #27906, #33479, #5426 ) ;
#30328 = CARTESIAN_POINT ( 'NONE',  ( 7.999999999999992895, 6.109652351741788223, 46.58570277113510372 ) ) ;
#30329 = VECTOR ( 'NONE', #16447, 1000.000000000000000 ) ;
#30330 = CARTESIAN_POINT ( 'NONE',  ( 7.999999999999992895, 22.82995208772746665, -41.06517797613640397 ) ) ;
#30332 = VERTEX_POINT ( 'NONE', #56 ) ;
#30331 = STYLED_ITEM ( 'NONE', ( #10007 ), #34287 ) ;
#30333 = EDGE_CURVE ( 'NONE', #10690, #15000, #21469, .T. ) ;
#30334 = CARTESIAN_POINT ( 'NONE',  ( -35.50000000000000711, -114.0650276068786582, 9.507762098804159123 ) ) ;
#30335 = CARTESIAN_POINT ( 'NONE',  ( -1.566204647097432900, -6.822536405429440620, -0.7999999999999951594 ) ) ;
#30336 = DIRECTION ( 'NONE',  ( -1.000000000000000000, 0.000000000000000000, 0.000000000000000000 ) ) ;
#30337 = AXIS2_PLACEMENT_3D ( 'NONE', #263, #19514, #14459 ) ;
#30338 = DIRECTION ( 'NONE',  ( -1.000000000000000000, 5.339440136655853966E-16, 0.000000000000000000 ) ) ;
#30339 = ORIENTED_EDGE ( 'NONE', *, *, #6451, .F. ) ;
#30340 = DIRECTION ( 'NONE',  ( -1.000000000000000000, -0.000000000000000000, 0.000000000000000000 ) ) ;
#30341 = DIRECTION ( 'NONE',  ( -1.000000000000000000, 0.000000000000000000, 0.000000000000000000 ) ) ;
#30342 = DIRECTION ( 'NONE',  ( -1.000000000000000000, 0.000000000000000000, 0.000000000000000000 ) ) ;
#30343 = CARTESIAN_POINT ( 'NONE',  ( 8.000000000000000000, 5.400000000000013678, 5.082197683525802034E-18 ) ) ;
#30344 = ITEM_DEFINED_TRANSFORMATION ( 'NONE', 'NONE', #20660,  #21307 ) ;
#30345 = CARTESIAN_POINT ( 'NONE',  ( 8.000000000000007105, 1.111908866155322695, -9.433698091065103597 ) ) ;
#30346 = CARTESIAN_POINT ( 'NONE',  ( 12.55910585664917711, 0.7408941433508786645, -1.200000000000006617 ) ) ;
#30347 = ORIENTED_EDGE ( 'NONE', *, *, #21810, .T. ) ;
#30348 =( LENGTH_UNIT ( ) NAMED_UNIT ( * ) SI_UNIT ( .MILLI., .METRE. ) );
#30349 = CIRCLE ( 'NONE', #18820, 20.00000000000000711 ) ;
#30350 = DIRECTION ( 'NONE',  ( -1.000000000000000000, -0.000000000000000000, -0.000000000000000000 ) ) ;
#30351 = DIRECTION ( 'NONE',  ( -0.000000000000000000, 0.000000000000000000, -1.000000000000000000 ) ) ;
#30352 = ORIENTED_EDGE ( 'NONE', *, *, #12804, .F. ) ;
#30353 = CARTESIAN_POINT ( 'NONE',  ( -36.25098837183130485, -114.6652019342044184, 2.683975545821551734 ) ) ;
#30354 = ORIENTED_EDGE ( 'NONE', *, *, #19558, .F. ) ;
#30355 = AXIS2_PLACEMENT_3D ( 'NONE', #1425, #17255, #28259 ) ;
#30356 = VERTEX_POINT ( 'NONE', #19128 ) ;
#30357 = ORIENTED_EDGE ( 'NONE', *, *, #12652, .T. ) ;
#30358 = AXIS2_PLACEMENT_3D ( 'NONE', #19559, #27168, #24638 ) ;
#30359 = FACE_OUTER_BOUND ( 'NONE', #2004, .T. ) ;
#30360 = AXIS2_PLACEMENT_3D ( 'NONE', #4501, #6812, #18328 ) ;
#30361 = CARTESIAN_POINT ( 'NONE',  ( 4.000000000000003553, 9.508666619816651178, 19.83898331853691488 ) ) ;
#30362 = EDGE_CURVE ( 'NONE', #4539, #28558, #8146, .T. ) ;
#30363 = FACE_BOUND ( 'NONE', #9841, .T. ) ;
#30364 = FACE_BOUND ( 'NONE', #17347, .T. ) ;
#30365 = EDGE_CURVE ( 'NONE', #20288, #21409, #24464, .T. ) ;
#30366 = DIRECTION ( 'NONE',  ( -1.000000000000000000, 0.000000000000000000, 0.000000000000000000 ) ) ;
#30367 = AXIS2_PLACEMENT_3D ( 'NONE', #962, #22377, #31022 ) ;
#30368 = DIRECTION ( 'NONE',  ( -1.000000000000000000, -0.000000000000000000, -0.000000000000000000 ) ) ;
#30369 = CARTESIAN_POINT ( 'NONE',  ( 8.000000000000000000, -11.19999565274257414, 10.71350075272070512 ) ) ;
#30370 = CARTESIAN_POINT ( 'NONE',  ( 0.000000000000000000, -10.46102064772354723, 19.35373470438981869 ) ) ;
#30371 = EDGE_CURVE ( 'NONE', #9304, #30389, #27080, .T. ) ;
#30372 = CARTESIAN_POINT ( 'NONE',  ( -39.00000000000000000, -115.9929510916434481, 12.59652202191340820 ) ) ;
#30373 = DIRECTION ( 'NONE',  ( -1.000000000000000000, 0.000000000000000000, 0.000000000000000000 ) ) ;
#30374 = AXIS2_PLACEMENT_3D ( 'NONE', #28189, #26021, #22945 ) ;
#30375 = AXIS2_PLACEMENT_3D ( 'NONE', #2508, #16149, #24285 ) ;
#30376 = EDGE_CURVE ( 'NONE', #9296, #15714, #29603, .T. ) ;
#30377 = CARTESIAN_POINT ( 'NONE',  ( -37.49999999999999289, -11.52052244843579309, 112.1848168619253840 ) ) ;
#30378 = VECTOR ( 'NONE', #3482, 1000.000000000000000 ) ;
#30379 = CARTESIAN_POINT ( 'NONE',  ( -10.00000000000000000, 0.000000000000000000, 0.000000000000000000 ) ) ;
#30380 = FACE_OUTER_BOUND ( 'NONE', #21878, .T. ) ;
#30381 = FACE_BOUND ( 'NONE', #750, .T. ) ;
#30382 = CYLINDRICAL_SURFACE ( 'NONE', #13796, 4.980000000000017302 ) ;
#30383 = ORIENTED_EDGE ( 'NONE', *, *, #4006, .F. ) ;
#30384 = CARTESIAN_POINT ( 'NONE',  ( -35.62769128460905677, -112.5438815906447729, 8.308975545821549957 ) ) ;
#30385 = DIRECTION ( 'NONE',  ( -1.000000000000000000, 0.000000000000000000, 0.000000000000000000 ) ) ;
#30386 = CARTESIAN_POINT ( 'NONE',  ( 0.000000000000000000, 0.000000000000000000, 0.000000000000000000 ) ) ;
#30387 = PLANE ( 'NONE',  #31392 ) ;
#30388 = ORIENTED_EDGE ( 'NONE', *, *, #3993, .T. ) ;
#30389 = VERTEX_POINT ( 'NONE', #24731 ) ;
#30390 = DIRECTION ( 'NONE',  ( 0.000000000000000000, -1.000000000000000000, 0.000000000000000000 ) ) ;
#30391 = CARTESIAN_POINT ( 'NONE',  ( -35.00000000000000000, -114.0000000000000853, 2.000000000000001776 ) ) ;
#30392 = ORIENTED_EDGE ( 'NONE', *, *, #15851, .T. ) ;
#30393 = VERTEX_POINT ( 'NONE', #2596 ) ;
#30394 = EDGE_CURVE ( 'NONE', #21828, #30963, #5464, .T. ) ;
#30395 = PLANE ( 'NONE',  #8260 ) ;
#30396 = DIRECTION ( 'NONE',  ( 1.734723475976807094E-16, -1.000000000000000000, 0.000000000000000000 ) ) ;
#30397 = AXIS2_PLACEMENT_3D ( 'NONE', #29647, #27131, #21883 ) ;
#30398 = VECTOR ( 'NONE', #4074, 1000.000000000000000 ) ;
#30399 = APPLICATION_PROTOCOL_DEFINITION ( 'draft international standard', 'automotive_design', 1998, #34480 ) ;
#30400 = DIRECTION ( 'NONE',  ( 0.000000000000000000, 0.000000000000000000, -1.000000000000000000 ) ) ;
#30401 = EDGE_LOOP ( 'NONE', ( #32921, #21332, #7649, #2518 ) ) ;
#30402 = ORIENTED_EDGE ( 'NONE', *, *, #8805, .F. ) ;
#30403 = CIRCLE ( 'NONE', #21773, 4.000000000000000000 ) ;
#30404 = ADVANCED_FACE ( 'NONE', ( #7795 ), #13390, .T. ) ;
#30405 = CYLINDRICAL_SURFACE ( 'NONE', #20273, 5.000000000000011546 ) ;
#30406 = ADVANCED_FACE ( 'NONE', ( #24028 ), #24371, .F. ) ;
#30407 = EDGE_CURVE ( 'NONE', #25593, #22962, #12951, .T. ) ;
#30408 = CARTESIAN_POINT ( 'NONE',  ( -1.000000000000000888, -6.008326913195953800, -0.7999999999999951594 ) ) ;
#30409 = ORIENTED_EDGE ( 'NONE', *, *, #27677, .F. ) ;
#30410 = CYLINDRICAL_SURFACE ( 'NONE', #18948, 4.000000000000000000 ) ;
#30411 = CARTESIAN_POINT ( 'NONE',  ( -34.50000000000000000, -115.5178116849130276, -1.498529437126731034 ) ) ;
#30412 = CARTESIAN_POINT ( 'NONE',  ( -37.49023442168701337, -114.9929510916434339, 14.11852773550420359 ) ) ;
#30413 = CARTESIAN_POINT ( 'NONE',  ( -35.50000000000000000, -113.9929510916434623, 10.50436693183592141 ) ) ;
#30414 = DIRECTION ( 'NONE',  ( 0.000000000000000000, 0.000000000000000000, -1.000000000000000000 ) ) ;
#30415 = ADVANCED_FACE ( 'NONE', ( #30310 ), #16236, .F. ) ;
#30416 = CARTESIAN_POINT ( 'NONE',  ( -34.68937937320795584, -114.9929510916434339, 13.37409560816408671 ) ) ;
#30417 = CYLINDRICAL_SURFACE ( 'NONE', #26854, 17.49900000000000233 ) ;
#30418 = ORIENTED_EDGE ( 'NONE', *, *, #13022, .T. ) ;
#30419 = EDGE_CURVE ( 'NONE', #11413, #14117, #26727, .T. ) ;
#30420 = LINE ( 'NONE', #27716, #12086 ) ;
#30421 = CARTESIAN_POINT ( 'NONE',  ( -29.99999999999999645, -26.00000000000000000, 113.9999999999999858 ) ) ;
#30422 = CARTESIAN_POINT ( 'NONE',  ( 0.000000000000000000, -13.60411018104308667, -12.96676809804163000 ) ) ;
#30423 = DIRECTION ( 'NONE',  ( -1.000000000000000000, -0.000000000000000000, -0.000000000000000000 ) ) ;
#30424 = ORIENTED_EDGE ( 'NONE', *, *, #19446, .T. ) ;
#30425 = CARTESIAN_POINT ( 'NONE',  ( -38.00000000000000711, -114.9929510916434339, 12.17846912687782179 ) ) ;
#30426 = ORIENTED_EDGE ( 'NONE', *, *, #2910, .F. ) ;
#30427 = CARTESIAN_POINT ( 'NONE',  ( -37.05926240293133134, -116.9999999999999858, 6.378524454178448266 ) ) ;
#30428 = CARTESIAN_POINT ( 'NONE',  ( 0.000000000000000000, 0.000000000000000000, 0.000000000000000000 ) ) ;
#30429 = CARTESIAN_POINT ( 'NONE',  ( -35.50000000000000711, -115.8878449012421754, -1.128496220799388494 ) ) ;
#30430 = ORIENTED_EDGE ( 'NONE', *, *, #19334, .F. ) ;
#30431 = VECTOR ( 'NONE', #4774, 1000.000000000000000 ) ;
#30432 = EDGE_LOOP ( 'NONE', ( #34720, #23412, #32726, #29625 ) ) ;
#30433 = DIRECTION ( 'NONE',  ( 0.000000000000000000, -0.8660254037844431485, 0.4999999999999922284 ) ) ;
#30434 = CARTESIAN_POINT ( 'NONE',  ( 8.000000000000000000, -6.085920226791118992, 15.78165944574518775 ) ) ;
#30435 = ORIENTED_EDGE ( 'NONE', *, *, #31485, .F. ) ;
#30436 = EDGE_CURVE ( 'NONE', #26597, #18803, #25601, .T. ) ;
#30437 = DIRECTION ( 'NONE',  ( 0.000000000000000000, 0.000000000000000000, 1.000000000000000000 ) ) ;
#30438 = CARTESIAN_POINT ( 'NONE',  ( -35.00000000000000000, -116.0140978167138712, 0.8752176474015622709 ) ) ;
#30439 = VERTEX_POINT ( 'NONE', #14257 ) ;
#30441 = EDGE_LOOP ( 'NONE', ( #34762, #1972 ) ) ;
#30440 = EDGE_CURVE ( 'NONE', #20040, #22033, #225, .T. ) ;
#30442 = LINE ( 'NONE', #19256, #24012 ) ;
#30443 = EDGE_CURVE ( 'NONE', #7406, #20345, #32521, .T. ) ;
#30444 =( LENGTH_UNIT ( ) NAMED_UNIT ( * ) SI_UNIT ( .MILLI., .METRE. ) );
#30445 = FACE_OUTER_BOUND ( 'NONE', #29992, .T. ) ;
#30446 = ORIENTED_EDGE ( 'NONE', *, *, #31301, .T. ) ;
#30447 = ORIENTED_EDGE ( 'NONE', *, *, #19827, .F. ) ;
#30448 = CARTESIAN_POINT ( 'NONE',  ( -35.50000000000000000, -112.8690837874180062, 2.872105769100646189 ) ) ;
#30449 = EDGE_CURVE ( 'NONE', #32215, #30567, #22746, .T. ) ;
#30450 = VECTOR ( 'NONE', #6219, 1000.000000000000000 ) ;
#30451 = CARTESIAN_POINT ( 'NONE',  ( -1.498621416870293821, 0.000000000000000000, 0.000000000000000000 ) ) ;
#30452 = ORIENTED_EDGE ( 'NONE', *, *, #313, .T. ) ;
#30453 = ADVANCED_FACE ( 'NONE', ( #8510, #13913 ), #11734, .F. ) ;
#30454 = CARTESIAN_POINT ( 'NONE',  ( -35.99386409314529800, -114.9929510916434339, 13.11852378322482515 ) ) ;
#30455 = CIRCLE ( 'NONE', #33301, 52.00000000000000711 ) ;
#30456 = CARTESIAN_POINT ( 'NONE',  ( -34.54793860109200665, -113.9929510916434339, 13.00730889637958221 ) ) ;
#30457 = DIRECTION ( 'NONE',  ( 0.000000000000000000, 0.000000000000000000, -1.000000000000000000 ) ) ;
#30458 = LINE ( 'NONE', #28104, #34071 ) ;
#30459 = CIRCLE ( 'NONE', #7446, 7.199999999999993072 ) ;
#30460 = CARTESIAN_POINT ( 'NONE',  ( -34.50000000000000000, -113.9929510916435049, 10.50625754673586876 ) ) ;
#30462 = CARTESIAN_POINT ( 'NONE',  ( -39.00000000000000711, -114.9929510916434339, 12.39849696637031151 ) ) ;
#30461 = VECTOR ( 'NONE', #23574, 1000.000000000000000 ) ;
#30463 = CARTESIAN_POINT ( 'NONE',  ( -35.50000000000000711, -114.9912366357066986, 10.44580456020104720 ) ) ;
#30464 = CARTESIAN_POINT ( 'NONE',  ( -4.000000000000000000, 0.000000000000000000, -55.00000000000000000 ) ) ;
#30465 = EDGE_LOOP ( 'NONE', ( #24878, #22391, #7829, #6429 ) ) ;
#30466 = ORIENTED_EDGE ( 'NONE', *, *, #31972, .T. ) ;
#30467 = DIRECTION ( 'NONE',  ( 0.000000000000000000, 0.000000000000000000, -1.000000000000000000 ) ) ;
#30468 = DIRECTION ( 'NONE',  ( 0.000000000000000000, -0.6427876096865294819, -0.7660444431189861181 ) ) ;
#30469 = ORIENTED_EDGE ( 'NONE', *, *, #14367, .F. ) ;
#30470 = DIRECTION ( 'NONE',  ( -1.000000000000000000, 0.000000000000000000, 0.000000000000000000 ) ) ;
#30471 = ORIENTED_EDGE ( 'NONE', *, *, #20047, .T. ) ;
#30472 = CARTESIAN_POINT ( 'NONE',  ( -35.50000000000000000, -113.0140978167138712, 0.8752176474015154195 ) ) ;
#30473 = FACE_OUTER_BOUND ( 'NONE', #9609, .T. ) ;
#30474 = CARTESIAN_POINT ( 'NONE',  ( -36.23083527818512550, -116.0245472910329880, 6.284774454178450043 ) ) ;
#30475 = VECTOR ( 'NONE', #19868, 1000.000000000000000 ) ;
#30476 = CARTESIAN_POINT ( 'NONE',  ( -43.99999999999999289, -44.99999999999999289, 0.000000000000000000 ) ) ;
#30477 = EDGE_CURVE ( 'NONE', #22707, #211, #12981, .T. ) ;
#30478 = VERTEX_POINT ( 'NONE', #25072 ) ;
#30479 = AXIS2_PLACEMENT_3D ( 'NONE', #17048, #6260, #16527 ) ;
#30480 = ADVANCED_FACE ( 'NONE', ( #9038 ), #19814, .T. ) ;
#30481 = DIRECTION ( 'NONE',  ( 0.000000000000000000, 0.000000000000000000, -1.000000000000000000 ) ) ;
#30482 = CARTESIAN_POINT ( 'NONE',  ( -35.50000000000000711, -114.0000000000000853, 2.000000000000001776 ) ) ;
#30483 = ORIENTED_EDGE ( 'NONE', *, *, #4281, .F. ) ;
#30484 = VERTEX_POINT ( 'NONE', #28307 ) ;
#30485 = CARTESIAN_POINT ( 'NONE',  ( -35.02454729103298803, -114.8876895276775087, 4.597274454178448266 ) ) ;
#30486 = CIRCLE ( 'NONE', #21831, 52.00000000000000711 ) ;
#30487 = CARTESIAN_POINT ( 'NONE',  ( 0.000000000000000000, 46.87740477351712798, 3.172455868806031809 ) ) ;
#30488 = AXIS2_PLACEMENT_3D ( 'NONE', #21927, #15625, #15986 ) ;
#30489 = DIRECTION ( 'NONE',  ( -1.000000000000000000, 0.000000000000000000, 0.000000000000000000 ) ) ;
#30490 = ORIENTED_EDGE ( 'NONE', *, *, #27088, .T. ) ;
#30491 = EDGE_LOOP ( 'NONE', ( #29107, #10873, #29951, #15514 ) ) ;
#30492 = CARTESIAN_POINT ( 'NONE',  ( -34.50000000000000000, -113.3557509229967764, 1.923098431109107054 ) ) ;
#30493 = CARTESIAN_POINT ( 'NONE',  ( 0.000000000000000000, -2.710505431213761085E-17, 55.00000000000000000 ) ) ;
#30494 = CYLINDRICAL_SURFACE ( 'NONE', #8561, 20.00000000000000355 ) ;
#30495 = CARTESIAN_POINT ( 'NONE',  ( -35.50000000000000000, -113.9929510916433344, 10.50625754673586876 ) ) ;
#30496 = CARTESIAN_POINT ( 'NONE',  ( -55.00000000000000000, 0.000000000000000000, 70.00000000000000000 ) ) ;
#30497 = DIRECTION ( 'NONE',  ( -1.000000000000000000, -0.000000000000000000, 0.000000000000000000 ) ) ;
#30498 = CARTESIAN_POINT ( 'NONE',  ( -34.50000000000000000, -116.0012805033554883, -0.7876962586524312027 ) ) ;
#30499 = CARTESIAN_POINT ( 'NONE',  ( -39.00000000000000000, -115.9929510916434481, 12.59652202191340820 ) ) ;
#30500 = CARTESIAN_POINT ( 'NONE',  ( 8.000000000000000000, -16.94522934049206597, -8.128228055639052485 ) ) ;
#30501 = CIRCLE ( 'NONE', #13817, 22.00000000000000000 ) ;
#30502 = DIRECTION ( 'NONE',  ( 0.000000000000000000, 0.9510565162951521989, 0.3090169943749515036 ) ) ;
#30503 = EDGE_LOOP ( 'NONE', ( #17398, #24686, #26494, #21298 ) ) ;
#30504 = CIRCLE ( 'NONE', #35121, 20.00000000000000711 ) ;
#30505 = CIRCLE ( 'NONE', #14959, 15.49899999999998279 ) ;
#30506 = DIRECTION ( 'NONE',  ( -1.000000000000000000, 0.000000000000000000, 0.000000000000000000 ) ) ;
#30507 = CARTESIAN_POINT ( 'NONE',  ( 7.999999999999992895, -46.11014828289837197, -9.022736828081189486 ) ) ;
#30508 = CARTESIAN_POINT ( 'NONE',  ( 7.999999999999992895, 0.000000000000000000, 0.000000000000000000 ) ) ;
#30509 = ORIENTED_EDGE ( 'NONE', *, *, #10982, .T. ) ;
#30510 = CARTESIAN_POINT ( 'NONE',  ( 23.00000000000000711, 1.230770033143090132E-14, 0.000000000000000000 ) ) ;
#30511 = CARTESIAN_POINT ( 'NONE',  ( 8.000000000000000000, 2.494040418455352182, 18.62763138773848937 ) ) ;
#30512 = CARTESIAN_POINT ( 'NONE',  ( 8.000000000000000000, 6.860320204751340079, -13.89802171851375689 ) ) ;
#30513 = CARTESIAN_POINT ( 'NONE',  ( 0.000000000000000000, -25.61928775981074935, 45.25098998563470332 ) ) ;
#30514 = DIRECTION ( 'NONE',  ( 1.000000000000000000, -0.000000000000000000, -0.000000000000000000 ) ) ;
#30515 = LINE ( 'NONE', #14456, #19329 ) ;
#30516 = VERTEX_POINT ( 'NONE', #579 ) ;
#30517 = EDGE_CURVE ( 'NONE', #22358, #2456, #22181, .T. ) ;
#30518 = CARTESIAN_POINT ( 'NONE',  ( 7.999999999999992895, 35.20873326984128227, -31.88259874183993503 ) ) ;
#30519 = FACE_OUTER_BOUND ( 'NONE', #5031, .T. ) ;
#30520 = ORIENTED_EDGE ( 'NONE', *, *, #32571, .F. ) ;
#30521 = AXIS2_PLACEMENT_3D ( 'NONE', #29350, #21034, #7546 ) ;
#30522 = CARTESIAN_POINT ( 'NONE',  ( -36.25098837183130485, -114.6652019342044184, 4.183975545821551734 ) ) ;
#30523 = ORIENTED_EDGE ( 'NONE', *, *, #25807, .F. ) ;
#30524 = ORIENTED_EDGE ( 'NONE', *, *, #31241, .F. ) ;
#30525 = EDGE_LOOP ( 'NONE', ( #18501, #33657, #21176, #10592 ) ) ;
#30526 = CARTESIAN_POINT ( 'NONE',  ( 8.000000000000007105, -8.725776631572617958, -3.753907720749127819 ) ) ;
#30527 = EDGE_CURVE ( 'NONE', #14196, #3377, #16983, .T. ) ;
#30528 = CIRCLE ( 'NONE', #1205, 7.199999999999995737 ) ;
#30529 = STYLED_ITEM ( 'NONE', ( #10729 ), #12087 ) ;
#30530 = CIRCLE ( 'NONE', #27094, 3.799999999999999822 ) ;
#30531 = CARTESIAN_POINT ( 'NONE',  ( -35.50000000000000711, -116.0124910254613297, -0.6902086197697608894 ) ) ;
#30532 = CARTESIAN_POINT ( 'NONE',  ( 0.000000000000000000, 5.482169781019050170, -16.00140663693117560 ) ) ;
#30533 = AXIS2_PLACEMENT_3D ( 'NONE', #9707, #28972, #4320 ) ;
#30534 = CARTESIAN_POINT ( 'NONE',  ( -35.50000000000000711, -114.0185793162512908, 9.502217742515812304 ) ) ;
#30535 = DIRECTION ( 'NONE',  ( 0.000000000000000000, 0.000000000000000000, 1.000000000000000000 ) ) ;
#30536 = CYLINDRICAL_SURFACE ( 'NONE', #25183, 3.799999999999999822 ) ;
#30537 = CARTESIAN_POINT ( 'NONE',  ( -34.50000000000000000, -114.1302255537607095, 9.515717283514957714 ) ) ;
#30538 = FACE_OUTER_BOUND ( 'NONE', #27377, .T. ) ;
#30539 = CARTESIAN_POINT ( 'NONE',  ( -35.00000000000000000, -114.0592624029316369, 9.003524454178483793 ) ) ;
#30540 = CARTESIAN_POINT ( 'NONE',  ( -36.12500000000014211, -115.9929510916434481, 14.11852480586265024 ) ) ;
#30541 = FACE_OUTER_BOUND ( 'NONE', #11040, .T. ) ;
#30542 = CARTESIAN_POINT ( 'NONE',  ( -6.938893903907228378E-15, 0.7408941433508786645, -1.200000000000006617 ) ) ;
#30543 = FACE_OUTER_BOUND ( 'NONE', #35266, .T. ) ;
#30544 = DIRECTION ( 'NONE',  ( 0.000000000000000000, -0.4999999999999958367, -0.8660254037844410391 ) ) ;
#30545 = CARTESIAN_POINT ( 'NONE',  ( 50.00005079999999680, 5.400000000000000355, 0.9999999999999985567 ) ) ;
#30546 = ORIENTED_EDGE ( 'NONE', *, *, #10595, .F. ) ;
#30547 =( GEOMETRIC_REPRESENTATION_CONTEXT ( 3 ) GLOBAL_UNCERTAINTY_ASSIGNED_CONTEXT ( ( #17860 ) ) GLOBAL_UNIT_ASSIGNED_CONTEXT ( ( #34474, #26366, #34650 ) ) REPRESENTATION_CONTEXT ( 'NONE', 'WORKASPACE' ) );
#30548 = CARTESIAN_POINT ( 'NONE',  ( -39.02454729103295961, -113.2308352781851539, 7.840225545821551734 ) ) ;
#30549 = CIRCLE ( 'NONE', #16732, 4.000000000000000000 ) ;
#30550 = LINE ( 'NONE', #24444, #6050 ) ;
#30551 = CARTESIAN_POINT ( 'NONE',  ( 7.999999999999992895, 13.85708833600033074, -45.43276465116652219 ) ) ;
#30552 = FACE_OUTER_BOUND ( 'NONE', #29858, .T. ) ;
#30553 = ORIENTED_EDGE ( 'NONE', *, *, #16886, .F. ) ;
#30554 = VERTEX_POINT ( 'NONE', #8853 ) ;
#30555 = UNCERTAINTY_MEASURE_WITH_UNIT (LENGTH_MEASURE( 1.000000000000000082E-05 ), #8317, 'distance_accuracy_value', 'NONE');
#30556 = EDGE_CURVE ( 'NONE', #21743, #7443, #30221, .T. ) ;
#30557 = DIRECTION ( 'NONE',  ( 1.000000000000000000, -1.110223024625156540E-16, 0.000000000000000000 ) ) ;
#30558 = DIRECTION ( 'NONE',  ( -1.000000000000000000, 0.000000000000000000, 0.000000000000000000 ) ) ;
#30559 = ORIENTED_EDGE ( 'NONE', *, *, #18094, .T. ) ;
#30560 = EDGE_CURVE ( 'NONE', #12699, #708, #3777, .T. ) ;
#30561 = VERTEX_POINT ( 'NONE', #3124 ) ;
#30562 = CARTESIAN_POINT ( 'NONE',  ( 0.000000000000000000, 0.000000000000000000, 0.000000000000000000 ) ) ;
#30563 = CARTESIAN_POINT ( 'NONE',  ( 0.000000000000000000, 36.34385289850631295, -29.77717097092039111 ) ) ;
#30564 = EDGE_CURVE ( 'NONE', #25573, #25593, #11824, .T. ) ;
#30565 = CARTESIAN_POINT ( 'NONE',  ( 8.000000000000007105, -0.3151488735047419665, 11.27190672109269798 ) ) ;
#30566 = ORIENTED_EDGE ( 'NONE', *, *, #16747, .T. ) ;
#30567 = VERTEX_POINT ( 'NONE', #14076 ) ;
#30568 = DIRECTION ( 'NONE',  ( 1.000000000000000000, -4.607758420995284547E-15, -1.174092375852883357E-15 ) ) ;
#30569 = DIRECTION ( 'NONE',  ( 1.000000000000000000, 0.000000000000000000, 0.000000000000000000 ) ) ;
#30570 = CIRCLE ( 'NONE', #19076, 2.799122904894268071 ) ;
#30571 = STYLED_ITEM ( 'NONE', ( #4558 ), #13375 ) ;
#30572 = EDGE_LOOP ( 'NONE', ( #13601, #30646, #17254, #25252, #18402, #25610 ) ) ;
#30573 = AXIS2_PLACEMENT_3D ( 'NONE', #13658, #3036, #22275 ) ;
#30574 = CYLINDRICAL_SURFACE ( 'NONE', #24721, 10.00000000000000000 ) ;
#30575 = CYLINDRICAL_SURFACE ( 'NONE', #10399, 7.199999999999994849 ) ;
#30576 = CARTESIAN_POINT ( 'NONE',  ( -36.87500000000098055, -114.9929510916434339, 14.11852480586264846 ) ) ;
#30577 = PLANE ( 'NONE',  #4822 ) ;
#30578 = CARTESIAN_POINT ( 'NONE',  ( 4.000000000000000000, 4.898587196589412829E-16, -43.60000000000000142 ) ) ;
#30579 = CARTESIAN_POINT ( 'NONE',  ( -36.62499999999902656, -114.9929510916434339, 14.11852480586264846 ) ) ;
#30580 = DIRECTION ( 'NONE',  ( 0.000000000000000000, 0.000000000000000000, -1.000000000000000000 ) ) ;
#30581 = EDGE_CURVE ( 'NONE', #35401, #26642, #5647, .T. ) ;
#30582 = LINE ( 'NONE', #13499, #27633 ) ;
#30583 = DIRECTION ( 'NONE',  ( -1.000000000000000000, -0.000000000000000000, 0.000000000000000000 ) ) ;
#30584 = CIRCLE ( 'NONE', #683, 7.199999999999998401 ) ;
#30585 = DIRECTION ( 'NONE',  ( 1.000000000000000000, -4.336808689941997226E-15, -1.174092375852883357E-15 ) ) ;
#30586 = DIRECTION ( 'NONE',  ( -1.000000000000000000, -1.734723475976807094E-16, -0.000000000000000000 ) ) ;
#30587 = ORIENTED_EDGE ( 'NONE', *, *, #18138, .F. ) ;
#30588 = CARTESIAN_POINT ( 'NONE',  ( 7.999999999999992895, 15.49408907645171851, 44.90087086784599535 ) ) ;
#30589 = EDGE_LOOP ( 'NONE', ( #33090, #28128, #19891, #18342 ) ) ;
#30590 = CARTESIAN_POINT ( 'NONE',  ( -34.02454729103298092, -115.3019030900506294, 7.597274454178449155 ) ) ;
#30591 = CARTESIAN_POINT ( 'NONE',  ( 7.999999999999992895, 42.41764978026606059, -20.20639853260303198 ) ) ;
#30592 = CARTESIAN_POINT ( 'NONE',  ( -35.50000000000000711, -115.5178116849130276, -1.498529437126731034 ) ) ;
#30593 = ORIENTED_EDGE ( 'NONE', *, *, #1601, .F. ) ;
#30594 = VERTEX_POINT ( 'NONE', #8678 ) ;
#30595 = ADVANCED_FACE ( 'NONE', ( #3654 ), #19646, .T. ) ;
#30596 = CARTESIAN_POINT ( 'NONE',  ( 0.000000000000000000, -7.613867765417476008, -5.679790370316101011 ) ) ;
#30597 = DIRECTION ( 'NONE',  ( -1.000000000000000000, 0.000000000000000000, 0.000000000000000000 ) ) ;
#30598 = EDGE_CURVE ( 'NONE', #34183, #16691, #25615, .T. ) ;
#30599 = EDGE_CURVE ( 'NONE', #8057, #6961, #3476, .T. ) ;
#30600 = ORIENTED_EDGE ( 'NONE', *, *, #27810, .T. ) ;
#30601 = CIRCLE ( 'NONE', #35219, 0.5000000000000004441 ) ;
#30602 = CARTESIAN_POINT ( 'NONE',  ( 0.000000000000000000, 42.60732521687599217, -19.80331771201615609 ) ) ;
#30603 = CARTESIAN_POINT ( 'NONE',  ( 0.000000000000000000, 0.000000000000000000, 0.000000000000000000 ) ) ;
#30604 = ORIENTED_EDGE ( 'NONE', *, *, #29996, .F. ) ;
#30605 = ORIENTED_EDGE ( 'NONE', *, *, #2171, .F. ) ;
#30606 = CARTESIAN_POINT ( 'NONE',  ( 7.999999999999992895, 39.55064067543064965, 25.36340625197373910 ) ) ;
#30607 = EDGE_CURVE ( 'NONE', #19681, #529, #10952, .T. ) ;
#30608 =( NAMED_UNIT ( * ) PLANE_ANGLE_UNIT ( ) SI_UNIT ( $, .RADIAN. ) );
#30609 = EDGE_CURVE ( 'NONE', #25964, #26106, #18203, .T. ) ;
#30610 = FACE_OUTER_BOUND ( 'NONE', #15257, .T. ) ;
#30611 = ORIENTED_EDGE ( 'NONE', *, *, #4035, .T. ) ;
#30612 = ORIENTED_EDGE ( 'NONE', *, *, #9124, .F. ) ;
#30613 = AXIS2_PLACEMENT_3D ( 'NONE', #3499, #11754, #20020 ) ;
#30614 = CARTESIAN_POINT ( 'NONE',  ( -34.50000000000000000, -114.9307644833806137, -2.624782352598442614 ) ) ;
#30615 = ORIENTED_EDGE ( 'NONE', *, *, #21126, .F. ) ;
#30616 = CARTESIAN_POINT ( 'NONE',  ( -36.50000000000011369, -114.9929510916434339, 13.11852480586264669 ) ) ;
#30617 = CARTESIAN_POINT ( 'NONE',  ( -37.37500000000009237, -113.9929510916434339, 14.11852480586265024 ) ) ;
#30618 = AXIS2_PLACEMENT_3D ( 'NONE', #19780, #11364, #22671 ) ;
#30619 = FACE_OUTER_BOUND ( 'NONE', #29716, .T. ) ;
#30620 = CARTESIAN_POINT ( 'NONE',  ( -55.00000000000000000, 10.00000000000000888, -15.00000000000000178 ) ) ;
#30621 = AXIS2_PLACEMENT_3D ( 'NONE', #18788, #2073, #26920 ) ;
#30622 = CARTESIAN_POINT ( 'NONE',  ( -34.50015059926905536, -113.9929510916434339, 12.64306614848962518 ) ) ;
#30623 = DIRECTION ( 'NONE',  ( 1.000000000000000000, -0.000000000000000000, 0.000000000000000000 ) ) ;
#30624 = EDGE_CURVE ( 'NONE', #31461, #11231, #15133, .T. ) ;
#30625 = CARTESIAN_POINT ( 'NONE',  ( -38.00000000000000711, -115.9929510916434481, 12.17846912687782179 ) ) ;
#30626 = CARTESIAN_POINT ( 'NONE',  ( 0.000000000000000000, 10.15474465512060398, 9.637487275701170475 ) ) ;
#30627 = DIRECTION ( 'NONE',  ( 1.000000000000000000, -0.000000000000000000, -0.000000000000000000 ) ) ;
#30628 = ORIENTED_EDGE ( 'NONE', *, *, #29068, .T. ) ;
#30629 = PRODUCT_RELATED_PRODUCT_CATEGORY ( 'part', '', ( #15545 ) ) ;
#30630 = EDGE_LOOP ( 'NONE', ( #18332, #25974, #18627, #4441 ) ) ;
#30631 = EDGE_CURVE ( 'NONE', #6172, #26694, #34609, .T. ) ;
#30632 = DIRECTION ( 'NONE',  ( 1.000000000000000000, -5.339440136655842133E-16, -1.047965281155519420E-16 ) ) ;
#30633 = CARTESIAN_POINT ( 'NONE',  ( 0.000000000000000000, -4.460989585141084568, 16.92083251265323440 ) ) ;
#30634 = VERTEX_POINT ( 'NONE', #23621 ) ;
#30635 = VECTOR ( 'NONE', #12775, 1000.000000000000000 ) ;
#30636 = CYLINDRICAL_SURFACE ( 'NONE', #6709, 8.000000000000051514 ) ;
#30637 = EDGE_LOOP ( 'NONE', ( #18247, #35483, #34105, #27890 ) ) ;
#30638 = AXIS2_PLACEMENT_3D ( 'NONE', #25138, #465, #8728 ) ;
#30639 = CARTESIAN_POINT ( 'NONE',  ( -35.50000000000000000, -115.0140978167138712, -0.6247823525984408377 ) ) ;
#30640 = DIRECTION ( 'NONE',  ( -1.000000000000000000, 0.000000000000000000, -0.000000000000000000 ) ) ;
#30641 = CARTESIAN_POINT ( 'NONE',  ( -37.88768952767750164, -115.9754527089670262, 6.472274454178450043 ) ) ;
#30642 = EDGE_CURVE ( 'NONE', #1965, #21046, #12674, .T. ) ;
#30643 = ADVANCED_FACE ( 'NONE', ( #4559 ), #29212, .F. ) ;
#30644 = ORIENTED_EDGE ( 'NONE', *, *, #10208, .T. ) ;
#30645 = DIRECTION ( 'NONE',  ( -0.000000000000000000, 0.8191520442889889120, 0.5735764363510502672 ) ) ;
#30646 = ORIENTED_EDGE ( 'NONE', *, *, #27324, .F. ) ;
#30647 = CARTESIAN_POINT ( 'NONE',  ( -42.49999999999999289, -14.60640646055094649, 76.70096189432339884 ) ) ;
#30648 = CARTESIAN_POINT ( 'NONE',  ( -35.50000000000000000, -117.0141134414687514, -0.5779076015960331603 ) ) ;
#30649 = AXIS2_PLACEMENT_3D ( 'NONE', #1261, #4159, #1441 ) ;
#30650 = ORIENTED_EDGE ( 'NONE', *, *, #14607, .F. ) ;
#30651 = ORIENTED_EDGE ( 'NONE', *, *, #6378, .T. ) ;
#30652 = CARTESIAN_POINT ( 'NONE',  ( 8.000000000000007105, -3.753907720749058541, 8.725776631572749409 ) ) ;
#30653 = AXIS2_PLACEMENT_3D ( 'NONE', #19680, #6544, #9076 ) ;
#30654 =( NAMED_UNIT ( * ) SI_UNIT ( $, .STERADIAN. ) SOLID_ANGLE_UNIT ( ) );
#30655 = EDGE_CURVE ( 'NONE', #31131, #27160, #23009, .T. ) ;
#30656 = CARTESIAN_POINT ( 'NONE',  ( 4.000000000000003553, 47.32430374665931794, 21.55018039121545215 ) ) ;
#30657 = VERTEX_POINT ( 'NONE', #26140 ) ;
#30658 = ORIENTED_EDGE ( 'NONE', *, *, #26880, .T. ) ;
#30659 = CARTESIAN_POINT ( 'NONE',  ( -34.50000000000000000, -112.0140978167138712, -0.4997823525984337878 ) ) ;
#30660 = DIRECTION ( 'NONE',  ( -1.000000000000000000, 0.000000000000000000, 0.000000000000000000 ) ) ;
#30661 = ORIENTED_EDGE ( 'NONE', *, *, #12960, .T. ) ;
#30662 = DIRECTION ( 'NONE',  ( 0.000000000000000000, 0.000000000000000000, -1.000000000000000000 ) ) ;
#30663 = AXIS2_PLACEMENT_3D ( 'NONE', #34174, #17054, #30753 ) ;
#30664 = AXIS2_PLACEMENT_3D ( 'NONE', #7102, #6927, #7282 ) ;
#30665 = CARTESIAN_POINT ( 'NONE',  ( -35.50400759022158326, -113.9929510916434339, 12.68378527132497524 ) ) ;
#30666 = AXIS2_PLACEMENT_3D ( 'NONE', #30892, #28197, #3368 ) ;
#30667 = CARTESIAN_POINT ( 'NONE',  ( 6.896599878636562764, -12.98179148322720167, -1.200000000000006617 ) ) ;
#30668 = DIRECTION ( 'NONE',  ( 0.000000000000000000, 0.000000000000000000, -1.000000000000000000 ) ) ;
#30669 = CARTESIAN_POINT ( 'NONE',  ( -34.50000000000000000, -112.4803765279500993, 2.803636946313094569 ) ) ;
#30670 = ADVANCED_FACE ( 'NONE', ( #1845 ), #20888, .T. ) ;
#30671 = CARTESIAN_POINT ( 'NONE',  ( -35.50000000000000000, -114.2450133963102843, 8.522190569412378736 ) ) ;
#30672 = DIRECTION ( 'NONE',  ( 1.000000000000000000, 0.000000000000000000, 0.000000000000000000 ) ) ;
#30673 = EDGE_CURVE ( 'NONE', #3956, #32057, #6509, .T. ) ;
#30675 = AXIS2_PLACEMENT_3D ( 'NONE', #16043, #32279, #13021 ) ;
#30674 = DIRECTION ( 'NONE',  ( 1.000000000000000000, -4.625929269271460867E-15, -1.156482317317865217E-15 ) ) ;
#30676 = VECTOR ( 'NONE', #20636, 1000.000000000000000 ) ;
#30677 = ADVANCED_FACE ( 'NONE', ( #23441 ), #28482, .T. ) ;
#30678 = ORIENTED_EDGE ( 'NONE', *, *, #4724, .F. ) ;
#30679 = CIRCLE ( 'NONE', #15131, 0.04099999999999937028 ) ;
#30680 = DIRECTION ( 'NONE',  ( -1.000000000000000000, -0.000000000000000000, -0.000000000000000000 ) ) ;
#30681 = DIRECTION ( 'NONE',  ( 0.000000000000000000, 0.000000000000000000, 1.000000000000000000 ) ) ;
#30682 = LINE ( 'NONE', #17149, #24894 ) ;
#30683 = EDGE_LOOP ( 'NONE', ( #31165, #34687 ) ) ;
#30684 = DIRECTION ( 'NONE',  ( -1.783119874454246424E-31, -1.187911941725854497E-31, 1.000000000000000000 ) ) ;
#30685 = DIRECTION ( 'NONE',  ( 1.000000000000000000, 0.000000000000000000, 0.000000000000000000 ) ) ;
#30686 = DIRECTION ( 'NONE',  ( 0.000000000000000000, -9.406921877466749789E-15, 1.000000000000000000 ) ) ;
#30687 = PLANE ( 'NONE',  #13824 ) ;
#30688 = EDGE_CURVE ( 'NONE', #21944, #24250, #4103, .T. ) ;
#30689 = CONTEXT_DEPENDENT_SHAPE_REPRESENTATION ( #4415, #10107 ) ;
#30690 = EDGE_CURVE ( 'NONE', #6413, #9689, #2384, .T. ) ;
#30691 = CARTESIAN_POINT ( 'NONE',  ( -42.49999999999999289, -33.18172400785640264, 69.52756813566438154 ) ) ;
#30692 = LINE ( 'NONE', #16637, #2124 ) ;
#30693 = VECTOR ( 'NONE', #34897, 1000.000000000000114 ) ;
#30694 = VERTEX_POINT ( 'NONE', #31180 ) ;
#30695 = DIRECTION ( 'NONE',  ( -1.000000000000000000, 0.000000000000000000, 0.000000000000000000 ) ) ;
#30696 = FACE_OUTER_BOUND ( 'NONE', #12858, .T. ) ;
#30697 = DIRECTION ( 'NONE',  ( -1.000000000000000000, 0.000000000000000000, 0.000000000000000000 ) ) ;
#30698 = ORIENTED_EDGE ( 'NONE', *, *, #7135, .T. ) ;
#30699 = CARTESIAN_POINT ( 'NONE',  ( -35.97545270896705460, -114.3549511594417680, 2.590225545821551734 ) ) ;
#30700 = VERTEX_POINT ( 'NONE', #28840 ) ;
#30701 = ORIENTED_EDGE ( 'NONE', *, *, #32128, .T. ) ;
#30702 = ORIENTED_EDGE ( 'NONE', *, *, #29132, .F. ) ;
#30703 = DIRECTION ( 'NONE',  ( -1.000000000000000000, 0.000000000000000000, 0.000000000000000000 ) ) ;
#30704 = CIRCLE ( 'NONE', #3672, 47.49900000000001654 ) ;
#30705 = AXIS2_PLACEMENT_3D ( 'NONE', #31594, #25492, #17903 ) ;
#30706 = CYLINDRICAL_SURFACE ( 'NONE', #35021, 47.49900000000001654 ) ;
#30707 = CARTESIAN_POINT ( 'NONE',  ( 0.000000000000000000, 0.000000000000000000, 0.000000000000000000 ) ) ;
#30708 = CARTESIAN_POINT ( 'NONE',  ( -35.50000000000000711, -114.9819937217110635, 10.35556074009299188 ) ) ;
#30709 = LINE ( 'NONE', #22761, #19500 ) ;
#30710 = DIRECTION ( 'NONE',  ( -1.174092375852890260E-15, 4.222049128630259891E-16, 1.000000000000000000 ) ) ;
#30711 = CARTESIAN_POINT ( 'NONE',  ( -34.50000000000000000, -114.9929510916434339, 10.52826033068511435 ) ) ;
#30712 = DIRECTION ( 'NONE',  ( -1.000000000000000000, 0.000000000000000000, 0.000000000000000000 ) ) ;
#30713 = EDGE_CURVE ( 'NONE', #7261, #14579, #7221, .T. ) ;
#30714 = DIRECTION ( 'NONE',  ( -1.000000000000000000, 0.000000000000000000, 0.000000000000000000 ) ) ;
#30715 = CARTESIAN_POINT ( 'NONE',  ( -35.50000000000000000, -114.1556834383649459, 8.511484393387789282 ) ) ;
#30716 = CARTESIAN_POINT ( 'NONE',  ( -35.50000000000000711, -112.0269151300720409, -0.7876962586524208776 ) ) ;
#30717 = FACE_OUTER_BOUND ( 'NONE', #23511, .T. ) ;
#30718 = DIRECTION ( 'NONE',  ( 0.000000000000000000, 0.000000000000000000, 1.000000000000000000 ) ) ;
#30719 = CARTESIAN_POINT ( 'NONE',  ( 7.999999999999992895, -8.053585752062238257, 46.81126742072021329 ) ) ;
#30720 = AXIS2_PLACEMENT_3D ( 'NONE', #20298, #23738, #31655 ) ;
#30721 = AXIS2_PLACEMENT_3D ( 'NONE', #21238, #21762, #24484 ) ;
#30722 = CARTESIAN_POINT ( 'NONE',  ( 7.999999999999992895, -26.17370628620627215, -39.63700417846191471 ) ) ;
#30723 = DIRECTION ( 'NONE',  ( -1.000000000000000000, -0.000000000000000000, -0.000000000000000000 ) ) ;
#30724 = EDGE_LOOP ( 'NONE', ( #30124, #28673, #35185, #13660 ) ) ;
#30725 = CARTESIAN_POINT ( 'NONE',  ( -37.99999999999998579, -114.0592624029313242, 3.246475545821551734 ) ) ;
#30726 = CARTESIAN_POINT ( 'NONE',  ( -4.000000000000000000, -2.710505431213761085E-17, 55.00000000000000000 ) ) ;
#30727 = CARTESIAN_POINT ( 'NONE',  ( 0.000000000000000000, -2.710505431213761085E-17, 38.00000000000000711 ) ) ;
#30728 = DIRECTION ( 'NONE',  ( -1.000000000000000000, 0.000000000000000000, 0.000000000000000000 ) ) ;
#30729 = ORIENTED_EDGE ( 'NONE', *, *, #15092, .T. ) ;
#30730 = VERTEX_POINT ( 'NONE', #12640 ) ;
#30731 = FACE_OUTER_BOUND ( 'NONE', #4957, .T. ) ;
#30732 = DIRECTION ( 'NONE',  ( -1.000000000000000000, 0.000000000000000000, 0.000000000000000000 ) ) ;
#30733 = ORIENTED_EDGE ( 'NONE', *, *, #4051, .T. ) ;
#30734 = EDGE_LOOP ( 'NONE', ( #32367, #31323, #8826, #29765 ) ) ;
#30735 = DIRECTION ( 'NONE',  ( 0.000000000000000000, 0.000000000000000000, 1.000000000000000000 ) ) ;
#30736 = DIRECTION ( 'NONE',  ( -1.000000000000000000, 0.000000000000000000, 0.000000000000000000 ) ) ;
#30737 = PRODUCT_CONTEXT ( 'NONE', #35176, 'mechanical' ) ;
#30738 = PLANE ( 'NONE',  #27144 ) ;
#30739 = VERTEX_POINT ( 'NONE', #4191 ) ;
#30740 = ORIENTED_EDGE ( 'NONE', *, *, #12300, .T. ) ;
#30741 = VECTOR ( 'NONE', #30732, 1000.000000000000000 ) ;
#30742 = AXIS2_PLACEMENT_3D ( 'NONE', #24439, #35425, #26978 ) ;
#30743 = FACE_OUTER_BOUND ( 'NONE', #31339, .T. ) ;
#30744 = CARTESIAN_POINT ( 'NONE',  ( 0.000000000000000000, 0.000000000000000000, 0.000000000000000000 ) ) ;
#30745 = ORIENTED_EDGE ( 'NONE', *, *, #26861, .F. ) ;
#30746 = CARTESIAN_POINT ( 'NONE',  ( 8.000000000000000000, 0.000000000000000000, 0.000000000000000000 ) ) ;
#30747 = VECTOR ( 'NONE', #33463, 1000.000000000000000 ) ;
#30748 = CARTESIAN_POINT ( 'NONE',  ( -34.50000000000000000, -113.4307644833805142, -0.6247823525984269599 ) ) ;
#30749 = DIRECTION ( 'NONE',  ( 0.000000000000000000, -3.469446951953611033E-15, -1.000000000000000000 ) ) ;
#30750 = CARTESIAN_POINT ( 'NONE',  ( -9.999999999999994671, 0.000000000000000000, 0.000000000000000000 ) ) ;
#30751 = EDGE_CURVE ( 'NONE', #14247, #29371, #29970, .T. ) ;
#30752 = CARTESIAN_POINT ( 'NONE',  ( -34.50000000000000000, -115.9929510916434481, 10.51725893871049067 ) ) ;
#30753 = DIRECTION ( 'NONE',  ( 1.047965281155515106E-16, -6.938893903907203726E-17, -1.000000000000000000 ) ) ;
#30754 = DIRECTION ( 'NONE',  ( 0.000000000000000000, 0.3681245526846786964, -0.9297764858882511252 ) ) ;
#30755 = CARTESIAN_POINT ( 'NONE',  ( -37.43749999999998579, -114.9929510916434339, 14.11852480586264846 ) ) ;
#30756 = CARTESIAN_POINT ( 'NONE',  ( 0.000000000000000000, 0.000000000000000000, 0.000000000000000000 ) ) ;
#30757 = DIRECTION ( 'NONE',  ( -1.000000000000000000, 0.000000000000000000, 0.000000000000000000 ) ) ;
#30758 = VECTOR ( 'NONE', #7240, 1000.000000000000000 ) ;
#30759 = CARTESIAN_POINT ( 'NONE',  ( 0.000000000000000000, 36.06787431788733045, -37.45808914225451502 ) ) ;
#30760 = DIRECTION ( 'NONE',  ( 9.615983791445651082E-17, -6.938893903907203726E-17, -1.000000000000000000 ) ) ;
#30761 = ORIENTED_EDGE ( 'NONE', *, *, #8476, .F. ) ;
#30762 = CARTESIAN_POINT ( 'NONE',  ( 7.999999999999992895, 2.123073309835184830, 47.45152853935336168 ) ) ;
#30763 = VERTEX_POINT ( 'NONE', #9752 ) ;
#30764 = EDGE_CURVE ( 'NONE', #9927, #3820, #30530, .T. ) ;
#30765 = CARTESIAN_POINT ( 'NONE',  ( -39.97545270896702618, -112.6980969099493990, 6.847274454178448266 ) ) ;
#30766 = CYLINDRICAL_SURFACE ( 'NONE', #12349, 20.00000000000000355 ) ;
#30767 = CARTESIAN_POINT ( 'NONE',  ( -35.50000000000000711, -112.0140900043366088, -0.5935324770972457697 ) ) ;
#30768 = VERTEX_POINT ( 'NONE', #18019 ) ;
#30769 = ORIENTED_EDGE ( 'NONE', *, *, #20217, .T. ) ;
#30771 = DIRECTION ( 'NONE',  ( 0.000000000000000000, -0.8660254037844410391, 0.4999999999999958367 ) ) ;
#30770 = PRODUCT_DEFINITION_SHAPE ( 'NONE', 'NONE',  #21149 ) ;
#30772 = DIRECTION ( 'NONE',  ( 0.000000000000000000, -6.987080667128811173E-15, 1.000000000000000000 ) ) ;
#30773 = ORIENTED_EDGE ( 'NONE', *, *, #16280, .T. ) ;
#30774 = AXIS2_PLACEMENT_3D ( 'NONE', #32828, #2421, #10507 ) ;
#30775 = CYLINDRICAL_SURFACE ( 'NONE', #19010, 7.199999999999994849 ) ;
#30776 = DIRECTION ( 'NONE',  ( 1.000000000000000000, 0.000000000000000000, 0.000000000000000000 ) ) ;
#30777 = ORIENTED_EDGE ( 'NONE', *, *, #7516, .F. ) ;
#30778 = ORIENTED_EDGE ( 'NONE', *, *, #16872, .T. ) ;
#30779 = CARTESIAN_POINT ( 'NONE',  ( -46.00000000000000000, 0.000000000000000000, 70.00000000000000000 ) ) ;
#30780 = EDGE_CURVE ( 'NONE', #35108, #6583, #16136, .T. ) ;
#30781 = PRESENTATION_STYLE_ASSIGNMENT (( #22141 ) ) ;
#30782 = DIRECTION ( 'NONE',  ( 1.000000000000000000, 0.000000000000000000, 0.000000000000000000 ) ) ;
#30783 = ORIENTED_EDGE ( 'NONE', *, *, #27166, .F. ) ;
#30784 = ORIENTED_EDGE ( 'NONE', *, *, #33672, .F. ) ;
#30785 = CARTESIAN_POINT ( 'NONE',  ( -35.50000000000000000, -111.0168437565048691, 0.9961850632443862708 ) ) ;
#30786 = EDGE_LOOP ( 'NONE', ( #308, #3809, #11354, #18015 ) ) ;
#30787 = CARTESIAN_POINT ( 'NONE',  ( -35.50005019975638021, -114.9929510916434339, 12.62670525340498529 ) ) ;
#30788 = EDGE_CURVE ( 'NONE', #17135, #19278, #15312, .T. ) ;
#30789 = CARTESIAN_POINT ( 'NONE',  ( -38.95206139890799335, -113.9929510916434339, 13.00730889637963550 ) ) ;
#30790 = AXIS2_PLACEMENT_3D ( 'NONE', #1911, #24223, #13074 ) ;
#30791 = EDGE_CURVE ( 'NONE', #2951, #17076, #32254, .T. ) ;
#30792 = CYLINDRICAL_SURFACE ( 'NONE', #3986, 20.00000000000000711 ) ;
#30793 = DIRECTION ( 'NONE',  ( 0.000000000000000000, -0.1253332335642905471, -0.9921147013144795412 ) ) ;
#30794 = CARTESIAN_POINT ( 'NONE',  ( -34.50075263804418313, -113.9929510916434339, 12.66759465831979981 ) ) ;
#30795 = DIRECTION ( 'NONE',  ( 1.000000000000000000, -5.339440136655842133E-16, -1.047965281155519420E-16 ) ) ;
#30796 = CIRCLE ( 'NONE', #15262, 8.000000000000007105 ) ;
#30797 = AXIS2_PLACEMENT_3D ( 'NONE', #15385, #18278, #1729 ) ;
#30798 = CARTESIAN_POINT ( 'NONE',  ( -35.50000000000000711, -114.0998638248492085, 9.511920366020609308 ) ) ;
#30799 = DIRECTION ( 'NONE',  ( 0.000000000000000000, 0.000000000000000000, -1.000000000000000000 ) ) ;
#30800 = DIRECTION ( 'NONE',  ( 1.000000000000000000, -0.000000000000000000, 0.000000000000000000 ) ) ;
#30801 = ORIENTED_EDGE ( 'NONE', *, *, #3829, .T. ) ;
#30802 = ORIENTED_EDGE ( 'NONE', *, *, #11474, .T. ) ;
#30803 = ADVANCED_FACE ( 'NONE', ( #21431, #24507 ), #10297, .F. ) ;
#30804 = DIRECTION ( 'NONE',  ( 0.000000000000000000, 0.000000000000000000, -1.000000000000000000 ) ) ;
#30805 = DIRECTION ( 'NONE',  ( 0.000000000000000000, 0.9822872507286879440, 0.1873813145857285700 ) ) ;
#30806 = EDGE_CURVE ( 'NONE', #33648, #28225, #12694, .T. ) ;
#30807 = VECTOR ( 'NONE', #19424, 1000.000000000000000 ) ;
#30808 = ORIENTED_EDGE ( 'NONE', *, *, #6679, .F. ) ;
#30809 = DIRECTION ( 'NONE',  ( -1.000000000000000000, 0.000000000000000000, -0.000000000000000000 ) ) ;
#30810 = ORIENTED_EDGE ( 'NONE', *, *, #3341, .F. ) ;
#30811 = CARTESIAN_POINT ( 'NONE',  ( -35.50000000000000000, -115.0140978167137860, -0.6411448143358557950 ) ) ;
#30812 = CARTESIAN_POINT ( 'NONE',  ( 8.000000000000000000, 14.80634052301623171, -8.177498406287266874 ) ) ;
#30813 = CARTESIAN_POINT ( 'NONE',  ( -35.99999999999999289, -114.0592624029313242, 9.003524454178446490 ) ) ;
#30814 = VERTEX_POINT ( 'NONE', #18562 ) ;
#30815 = CARTESIAN_POINT ( 'NONE',  ( 4.000000000000000000, 4.627536653468036720E-16, 29.09999999999999787 ) ) ;
#30816 = ORIENTED_EDGE ( 'NONE', *, *, #7360, .F. ) ;
#30817 = LINE ( 'NONE', #11037, #2722 ) ;
#30818 = AXIS2_PLACEMENT_3D ( 'NONE', #15338, #18762, #20742 ) ;
#30819 = CARTESIAN_POINT ( 'NONE',  ( -35.50000000000000711, -112.0141053790792114, 0.9054673897245171243 ) ) ;
#30820 = ORIENTED_EDGE ( 'NONE', *, *, #24261, .T. ) ;
#30821 = ORIENTED_EDGE ( 'NONE', *, *, #4478, .T. ) ;
#30822 = CARTESIAN_POINT ( 'NONE',  ( -36.11231047232249125, -112.0245472910329880, 4.222274454178449155 ) ) ;
#30823 = AXIS2_PLACEMENT_3D ( 'NONE', #16038, #13540, #29402 ) ;
#30824 = EDGE_CURVE ( 'NONE', #34828, #34524, #1206, .T. ) ;
#30825 = AXIS2_PLACEMENT_3D ( 'NONE', #18235, #29413, #18050 ) ;
#30826 = DIRECTION ( 'NONE',  ( 0.000000000000000000, 0.6427876096865403621, -0.7660444431189772363 ) ) ;
#30827 = VERTEX_POINT ( 'NONE', #18734 ) ;
#30828 = ORIENTED_EDGE ( 'NONE', *, *, #13890, .T. ) ;
#30829 = CARTESIAN_POINT ( 'NONE',  ( -34.50000000000000000, -112.0140978167138712, 0.6252176474015680441 ) ) ;
#30830 = VECTOR ( 'NONE', #15741, 1000.000000000000000 ) ;
#30831 = LINE ( 'NONE', #8682, #26369 ) ;
#30832 = ORIENTED_EDGE ( 'NONE', *, *, #7041, .T. ) ;
#30833 = ORIENTED_EDGE ( 'NONE', *, *, #15417, .T. ) ;
#30834 = VECTOR ( 'NONE', #9424, 1000.000000000000000 ) ;
#30835 = DIRECTION ( 'NONE',  ( -1.000000000000000000, 0.000000000000000000, 0.000000000000000000 ) ) ;
#30836 = EDGE_CURVE ( 'NONE', #16982, #22664, #4731, .T. ) ;
#30837 = CARTESIAN_POINT ( 'NONE',  ( -36.50000000000010658, -113.9929510916434339, 13.11852480586264846 ) ) ;
#30838 = DIRECTION ( 'NONE',  ( 0.000000000000000000, 0.000000000000000000, 1.000000000000000000 ) ) ;
#30839 = EDGE_CURVE ( 'NONE', #4881, #24556, #27040, .T. ) ;
#30840 = LINE ( 'NONE', #22723, #26886 ) ;
#30841 = ADVANCED_FACE ( 'NONE', ( #15668 ), #2385, .F. ) ;
#30842 = CARTESIAN_POINT ( 'NONE',  ( -34.50000000000000000, -113.2372261171341563, 2.916049522752222511 ) ) ;
#30843 = CARTESIAN_POINT ( 'NONE',  ( -39.00000000000000000, -115.9929510916434481, 12.26648026267477221 ) ) ;
#30844 = VECTOR ( 'NONE', #1263, 1000.000000000000000 ) ;
#30845 = CARTESIAN_POINT ( 'NONE',  ( 7.999999999999992895, 46.21320724403665281, -10.97699764141904488 ) ) ;
#30846 = LINE ( 'NONE', #421, #31837 ) ;
#30847 = AXIS2_PLACEMENT_3D ( 'NONE', #19545, #25333, #33593 ) ;
#30848 = DIRECTION ( 'NONE',  ( 9.266685234918781277E-17, -6.938893903907202493E-17, -1.000000000000000000 ) ) ;
#30849 = DIRECTION ( 'NONE',  ( -1.000000000000000000, 0.000000000000000000, 0.000000000000000000 ) ) ;
#30850 = DIRECTION ( 'NONE',  ( -1.000000000000000000, -0.000000000000000000, -0.000000000000000000 ) ) ;
#30851 = AXIS2_PLACEMENT_3D ( 'NONE', #19931, #28246, #20643 ) ;
#30852 = EDGE_CURVE ( 'NONE', #26218, #9081, #6358, .T. ) ;
#30853 = ORIENTED_EDGE ( 'NONE', *, *, #22729, .T. ) ;
#30854 = AXIS2_PLACEMENT_3D ( 'NONE', #21329, #15925, #2103 ) ;
#30855 = LINE ( 'NONE', #3502, #33508 ) ;
#30856 = CARTESIAN_POINT ( 'NONE',  ( 0.000000000000000000, 0.000000000000000000, -44.50000000000000000 ) ) ;
#30857 = CARTESIAN_POINT ( 'NONE',  ( -0.3000000000000016542, -14.69693845669907439, -1.200000000000006617 ) ) ;
#30858 = LINE ( 'NONE', #783, #27637 ) ;
#30859 = AXIS2_PLACEMENT_3D ( 'NONE', #34494, #7108, #15374 ) ;
#30860 = CONTEXT_DEPENDENT_SHAPE_REPRESENTATION ( #1397, #23920 ) ;
#30861 = AXIS2_PLACEMENT_3D ( 'NONE', #27072, #4762, #2415 ) ;
#30862 = DIRECTION ( 'NONE',  ( 0.000000000000000000, 0.000000000000000000, -1.000000000000000000 ) ) ;
#30863 = CARTESIAN_POINT ( 'NONE',  ( 8.000000000000000000, -14.18878633068154826, -6.236773481718229206 ) ) ;
#30864 = ORIENTED_EDGE ( 'NONE', *, *, #20768, .F. ) ;
#30865 = CARTESIAN_POINT ( 'NONE',  ( 0.000000000000000000, -11.06713717293229138, -13.55483219355740765 ) ) ;
#30866 = DIRECTION ( 'NONE',  ( -1.000000000000000000, 0.000000000000000000, 0.000000000000000000 ) ) ;
#30867 = DIRECTION ( 'NONE',  ( -1.000000000000000000, -0.000000000000000000, 0.000000000000000000 ) ) ;
#30868 = ORIENTED_EDGE ( 'NONE', *, *, #30607, .F. ) ;
#30869 = CARTESIAN_POINT ( 'NONE',  ( -38.02454729103295961, -113.6450488405582462, 6.340225545821551734 ) ) ;
#30870 = ORIENTED_EDGE ( 'NONE', *, *, #7516, .T. ) ;
#30871 = EDGE_CURVE ( 'NONE', #5721, #9761, #14985, .T. ) ;
#30872 = CIRCLE ( 'NONE', #21659, 7.499999999999992895 ) ;
#30873 = VERTEX_POINT ( 'NONE', #16374 ) ;
#30874 = ORIENTED_EDGE ( 'NONE', *, *, #524, .T. ) ;
#30875 = CARTESIAN_POINT ( 'NONE',  ( 4.000000000000003553, 46.77034588191337150, -22.72740077717178053 ) ) ;
#30876 = CIRCLE ( 'NONE', #35491, 20.00000000000000711 ) ;
#30877 = EDGE_CURVE ( 'NONE', #22597, #20473, #35149, .T. ) ;
#30878 = CARTESIAN_POINT ( 'NONE',  ( -35.50000000000000711, -115.5178116849130276, -1.498529437126731034 ) ) ;
#30879 = CIRCLE ( 'NONE', #8436, 20.00000000000000355 ) ;
#30880 = DIRECTION ( 'NONE',  ( 1.000000000000000000, 0.000000000000000000, 0.000000000000000000 ) ) ;
#30881 = LINE ( 'NONE', #12325, #32190 ) ;
#30882 = CIRCLE ( 'NONE', #3299, 7.199999999999994849 ) ;
#30883 = EDGE_CURVE ( 'NONE', #8708, #4534, #14393, .T. ) ;
#30884 = VECTOR ( 'NONE', #33971, 1000.000000000000000 ) ;
#30885 = FACE_OUTER_BOUND ( 'NONE', #13473, .T. ) ;
#30886 = ADVANCED_FACE ( 'NONE', ( #13707 ), #32079, .T. ) ;
#30887 = CARTESIAN_POINT ( 'NONE',  ( -34.50000000000000000, -114.9902084924877954, 10.43071793783961176 ) ) ;
#30888 = CARTESIAN_POINT ( 'NONE',  ( 44.00000000000000000, 1.616533774874506480E-14, 0.000000000000000000 ) ) ;
#30889 = DIRECTION ( 'NONE',  ( 1.000000000000000000, 0.000000000000000000, 0.000000000000000000 ) ) ;
#30890 = CARTESIAN_POINT ( 'NONE',  ( -35.50000000000000000, -115.9927366631908825, 10.47601115720670073 ) ) ;
#30891 = CARTESIAN_POINT ( 'NONE',  ( -35.50000000000000711, -112.0250551866464548, 1.025914454044489332 ) ) ;
#30892 = CARTESIAN_POINT ( 'NONE',  ( 70.00000000000001421, -30.47068043442695284, 88.33026027086506815 ) ) ;
#30893 = CARTESIAN_POINT ( 'NONE',  ( 0.000000000000000000, 0.000000000000000000, 0.000000000000000000 ) ) ;
#30894 = VECTOR ( 'NONE', #21717, 1000.000000000000000 ) ;
#30895 = CARTESIAN_POINT ( 'NONE',  ( 30.00000000000000000, 1.359357947053562196E-14, 0.000000000000000000 ) ) ;
#30896 = DIRECTION ( 'NONE',  ( 1.226634733346697831E-16, -0.9659258262890646485, -0.2588190451025342842 ) ) ;
#30897 = VECTOR ( 'NONE', #22766, 1000.000000000000000 ) ;
#30898 = DIRECTION ( 'NONE',  ( 1.000000000000000000, -0.000000000000000000, -0.000000000000000000 ) ) ;
#30899 = DIRECTION ( 'NONE',  ( 0.000000000000000000, 0.000000000000000000, 1.000000000000000000 ) ) ;
#30900 = ORIENTED_EDGE ( 'NONE', *, *, #19126, .F. ) ;
#30901 = CARTESIAN_POINT ( 'NONE',  ( -36.02454729103297382, -113.5265240346956261, 9.902725545821553510 ) ) ;
#30902 = DIRECTION ( 'NONE',  ( -1.000000000000000000, -0.000000000000000000, 0.000000000000000000 ) ) ;
#30903 = CIRCLE ( 'NONE', #9056, 4.000000000000000000 ) ;
#30904 = DIRECTION ( 'NONE',  ( 0.000000000000000000, 0.000000000000000000, 1.000000000000000000 ) ) ;
#30905 = VERTEX_POINT ( 'NONE', #29912 ) ;
#30906 = EDGE_LOOP ( 'NONE', ( #23748, #8877, #33393, #23167 ) ) ;
#30907 = VECTOR ( 'NONE', #11, 1000.000000000000000 ) ;
#30908 = DIRECTION ( 'NONE',  ( 0.000000000000000000, 0.000000000000000000, 1.000000000000000000 ) ) ;
#30909 = FACE_OUTER_BOUND ( 'NONE', #32581, .T. ) ;
#30910 = EDGE_LOOP ( 'NONE', ( #6595, #27368, #26800, #23373 ) ) ;
#30911 = CARTESIAN_POINT ( 'NONE',  ( -39.16322519054178741, -111.9205845034225177, 4.933975545821551734 ) ) ;
#30912 = ORIENTED_EDGE ( 'NONE', *, *, #4481, .F. ) ;
#30913 = AXIS2_PLACEMENT_3D ( 'NONE', #16276, #13599, #24594 ) ;
#30914 = ADVANCED_FACE ( 'NONE', ( #21787 ), #5258, .T. ) ;
#30915 = EDGE_CURVE ( 'NONE', #19601, #25221, #7409, .T. ) ;
#30916 = CARTESIAN_POINT ( 'NONE',  ( 50.00000000000000000, -25.98076211353320275, 92.99999999999991473 ) ) ;
#30917 = DIRECTION ( 'NONE',  ( 0.000000000000000000, 1.000000000000000000, 0.000000000000000000 ) ) ;
#30918 = ITEM_DEFINED_TRANSFORMATION ( 'NONE', 'NONE', #25287,  #21307 ) ;
#30919 = CARTESIAN_POINT ( 'NONE',  ( 0.000000000000000000, 0.000000000000000000, 36.00000000000000000 ) ) ;
#30920 = ORIENTED_EDGE ( 'NONE', *, *, #6902, .F. ) ;
#30921 = ORIENTED_EDGE ( 'NONE', *, *, #15535, .T. ) ;
#30922 = AXIS2_PLACEMENT_3D ( 'NONE', #14931, #20323, #17636 ) ;
#30923 = CARTESIAN_POINT ( 'NONE',  ( -34.49999999999998579, -14.67619866229203929, 93.25874355921412473 ) ) ;
#30924 = CIRCLE ( 'NONE', #19438, 4.800000000000003375 ) ;
#30925 = ORIENTED_EDGE ( 'NONE', *, *, #14553, .T. ) ;
#30926 = DIRECTION ( 'NONE',  ( 0.000000000000000000, 0.5877852522924743583, -0.8090169943749466741 ) ) ;
#30927 = AXIS2_PLACEMENT_3D ( 'NONE', #8558, #19530, #6041 ) ;
#30928 = AXIS2_PLACEMENT_3D ( 'NONE', #10053, #24114, #12764 ) ;
#30929 = CARTESIAN_POINT ( 'NONE',  ( -34.50000000000000000, -114.9307644833806137, -0.6247823525984269599 ) ) ;
#30930 = LINE ( 'NONE', #26517, #8716 ) ;
#30931 = DIRECTION ( 'NONE',  ( -1.000000000000000000, 0.000000000000000000, 0.000000000000000000 ) ) ;
#30932 = CARTESIAN_POINT ( 'NONE',  ( -34.50000000000000000, -114.2253558743059330, 8.519800927820798009 ) ) ;
#30933 = PLANE ( 'NONE',  #7672 ) ;
#30934 = CARTESIAN_POINT ( 'NONE',  ( -34.97545270896703329, -113.2308352781851397, 2.909774454178448710 ) ) ;
#30935 = CARTESIAN_POINT ( 'NONE',  ( -37.48437500000004263, -114.9929510916434339, 14.11852480586264846 ) ) ;
#30936 = DIRECTION ( 'NONE',  ( 0.000000000000000000, 0.000000000000000000, -1.000000000000000000 ) ) ;
#30937 = DIRECTION ( 'NONE',  ( 0.000000000000000000, 0.000000000000000000, 1.000000000000000000 ) ) ;
#30938 = FACE_OUTER_BOUND ( 'NONE', #23646, .T. ) ;
#30939 = CARTESIAN_POINT ( 'NONE',  ( -1.599999999999990319, 0.000000000000000000, 0.000000000000000000 ) ) ;
#30940 = EDGE_LOOP ( 'NONE', ( #4366, #29871, #5371, #21253 ) ) ;
#30941 = CARTESIAN_POINT ( 'NONE',  ( 8.000000000000000000, -16.53603053422215297, 8.931325931664547468 ) ) ;
#30942 = ORIENTED_EDGE ( 'NONE', *, *, #20458, .T. ) ;
#30943 = CARTESIAN_POINT ( 'NONE',  ( -33.97545270896702618, -112.8166217158120475, 4.409774454178449155 ) ) ;
#30944 = LINE ( 'NONE', #25378, #24998 ) ;
#30945 = CARTESIAN_POINT ( 'NONE',  ( -35.50000000000000711, -112.0651520602111191, -0.9469505670458575608 ) ) ;
#30946 = ORIENTED_EDGE ( 'NONE', *, *, #18754, .F. ) ;
#30947 = ORIENTED_EDGE ( 'NONE', *, *, #35085, .T. ) ;
#30948 = LINE ( 'NONE', #6106, #25193 ) ;
#30949 = DIRECTION ( 'NONE',  ( 1.000000000000000000, 0.000000000000000000, 0.000000000000000000 ) ) ;
#30950 = VERTEX_POINT ( 'NONE', #16195 ) ;
#30951 = VECTOR ( 'NONE', #9663, 1000.000000000000000 ) ;
#30952 = ORIENTED_EDGE ( 'NONE', *, *, #14115, .T. ) ;
#30953 = AXIS2_PLACEMENT_3D ( 'NONE', #3362, #8208, #11101 ) ;
#30954 = AXIS2_PLACEMENT_3D ( 'NONE', #30314, #25077, #5651 ) ;
#30955 = ADVANCED_FACE ( 'NONE', ( #34975 ), #18382, .T. ) ;
#30956 = DIRECTION ( 'NONE',  ( -1.000000000000000000, 0.000000000000000000, 0.000000000000000000 ) ) ;
#30957 = ORIENTED_EDGE ( 'NONE', *, *, #14731, .F. ) ;
#30958 = ORIENTED_EDGE ( 'NONE', *, *, #14757, .T. ) ;
#30959 = CARTESIAN_POINT ( 'NONE',  ( -36.11231047232249836, -115.9754527089670262, 5.777725545821550845 ) ) ;
#30960 = PRESENTATION_STYLE_ASSIGNMENT (( #25570 ) ) ;
#30961 = FACE_OUTER_BOUND ( 'NONE', #7216, .T. ) ;
#30962 = VERTEX_POINT ( 'NONE', #5427 ) ;
#30963 = VERTEX_POINT ( 'NONE', #21072 ) ;
#30964 = CARTESIAN_POINT ( 'NONE',  ( -35.50000000000000000, -111.0140978167138570, 0.5627176474015715968 ) ) ;
#30965 = EDGE_CURVE ( 'NONE', #15523, #27258, #15542, .T. ) ;
#30966 = CARTESIAN_POINT ( 'NONE',  ( -42.49999999999999289, -38.85511776651532756, 79.29903810567645905 ) ) ;
#30967 = EDGE_LOOP ( 'NONE', ( #13141, #9647, #6577, #6473, #7359 ) ) ;
#30968 = CARTESIAN_POINT ( 'NONE',  ( -35.95915003344517658, -114.9929510916434339, 13.11692036158763308 ) ) ;
#30969 = CARTESIAN_POINT ( 'NONE',  ( -39.00000000000000000, -113.9929510916434339, 11.73841344789285657 ) ) ;
#30970 = CARTESIAN_POINT ( 'NONE',  ( 112.0000000000000000, 81.48267994499606459, 30.15054357219658954 ) ) ;
#30971 = CIRCLE ( 'NONE', #28103, 14.00000000000000000 ) ;
#30972 = CARTESIAN_POINT ( 'NONE',  ( 65.00000000000001421, -26.38406014851796400, 79.52301627764160230 ) ) ;
#30973 = CARTESIAN_POINT ( 'NONE',  ( -36.99999999999988631, -113.9929510916434339, 14.11852480586265024 ) ) ;
#30974 = CARTESIAN_POINT ( 'NONE',  ( 0.000000000000000000, -2.710505431213761085E-17, -21.89999999999999858 ) ) ;
#30975 = VECTOR ( 'NONE', #27052, 1000.000000000000000 ) ;
#30976 = CARTESIAN_POINT ( 'NONE',  ( -35.50000000000000711, -114.9929510916434339, 12.39849696637031506 ) ) ;
#30977 = LINE ( 'NONE', #28109, #27977 ) ;
#30978 = AXIS2_PLACEMENT_3D ( 'NONE', #15179, #7451, #18428 ) ;
#30979 = DIRECTION ( 'NONE',  ( 0.000000000000000000, 0.8660254037844398178, -0.4999999999999980571 ) ) ;
#30980 = CARTESIAN_POINT ( 'NONE',  ( 44.00000000000000000, -10.99999999999997868, 0.000000000000000000 ) ) ;
#30981 = ORIENTED_EDGE ( 'NONE', *, *, #8566, .F. ) ;
#30982 = CARTESIAN_POINT ( 'NONE',  ( -38.00000000000000711, -115.9929510916434481, 11.91443571948719615 ) ) ;
#30983 = ORIENTED_EDGE ( 'NONE', *, *, #5211, .F. ) ;
#30984 = LINE ( 'NONE', #19793, #32171 ) ;
#30985 = DIRECTION ( 'NONE',  ( 0.000000000000000000, 0.000000000000000000, 1.000000000000000000 ) ) ;
#30986 = VERTEX_POINT ( 'NONE', #3607 ) ;
#30987 = CARTESIAN_POINT ( 'NONE',  ( -39.49999999999999289, -3.784235812937200460, 96.08311962715481513 ) ) ;
#30988 = VERTEX_POINT ( 'NONE', #33312 ) ;
#30989 = CARTESIAN_POINT ( 'NONE',  ( -35.50000000000000000, -114.3474311500471572, -0.6247823525984269599 ) ) ;
#30990 = CARTESIAN_POINT ( 'NONE',  ( 0.000000000000000000, 8.605879768205232594, 12.89022243466711437 ) ) ;
#30991 = CARTESIAN_POINT ( 'NONE',  ( -38.99999999999999289, -113.9407375970686900, 2.253524454178449155 ) ) ;
#30992 = ORIENTED_EDGE ( 'NONE', *, *, #23726, .F. ) ;
#30993 = CARTESIAN_POINT ( 'NONE',  ( -36.94073759706868287, -112.0000000000000142, 4.128524454178449155 ) ) ;
#30994 = DIRECTION ( 'NONE',  ( 0.000000000000000000, -1.000000000000000000, 0.000000000000000000 ) ) ;
#30995 = ADVANCED_FACE ( 'NONE', ( #30445 ), #30263, .T. ) ;
#30996 = CARTESIAN_POINT ( 'NONE',  ( -35.50000000000000711, -112.0154707866092707, 0.9357013553229778235 ) ) ;
#30997 = EDGE_LOOP ( 'NONE', ( #33424, #34250, #20500, #31260 ) ) ;
#30998 = ORIENTED_EDGE ( 'NONE', *, *, #15910, .F. ) ;
#30999 = ADVANCED_FACE ( 'NONE', ( #30610, #2911 ), #3254, .T. ) ;
#31000 = CYLINDRICAL_SURFACE ( 'NONE', #19354, 4.000000000000000000 ) ;
#31001 = AXIS2_PLACEMENT_3D ( 'NONE', #31459, #12911, #31807 ) ;
#31002 = CARTESIAN_POINT ( 'NONE',  ( 7.999999999999992895, 17.50309955389611716, 43.60271849949368317 ) ) ;
#31003 = ORIENTED_EDGE ( 'NONE', *, *, #20003, .T. ) ;
#31004 = ORIENTED_EDGE ( 'NONE', *, *, #13467, .F. ) ;
#31005 = AXIS2_PLACEMENT_3D ( 'NONE', #28316, #6517, #19491 ) ;
#31006 = CARTESIAN_POINT ( 'NONE',  ( -34.50000000000000000, -112.0140978167138712, 0.5627176474015717078 ) ) ;
#31007 = DIRECTION ( 'NONE',  ( -0.000000000000000000, 0.000000000000000000, -1.000000000000000000 ) ) ;
#31008 = EDGE_CURVE ( 'NONE', #32720, #11477, #3082, .T. ) ;
#31009 = AXIS2_PLACEMENT_3D ( 'NONE', #29318, #1770, #18319 ) ;
#31010 = ORIENTED_EDGE ( 'NONE', *, *, #5774, .F. ) ;
#31011 = PRODUCT_DEFINITION_CONTEXT ( 'detailed design', #25537, 'design' ) ;
#31012 = ORIENTED_EDGE ( 'NONE', *, *, #30199, .F. ) ;
#31013 = VECTOR ( 'NONE', #25756, 1000.000000000000000 ) ;
#31014 = DIRECTION ( 'NONE',  ( 0.000000000000000000, 0.000000000000000000, 1.000000000000000000 ) ) ;
#31015 = CARTESIAN_POINT ( 'NONE',  ( -35.96730626674924025, -113.9929510916434339, 13.11752178341330222 ) ) ;
#31016 = CARTESIAN_POINT ( 'NONE',  ( 0.000000000000000000, 0.000000000000000000, -3.000000000000002665 ) ) ;
#31017 = CARTESIAN_POINT ( 'NONE',  ( 7.999999999999992895, 42.03146605346819342, -22.12489237027273603 ) ) ;
#31018 = CARTESIAN_POINT ( 'NONE',  ( -35.50000000000000000, -113.9929510916434339, 12.57451923796416260 ) ) ;
#31019 = CARTESIAN_POINT ( 'NONE',  ( -35.50000000000000000, -115.9929510916434481, 11.21034663311132107 ) ) ;
#31020 = CARTESIAN_POINT ( 'NONE',  ( 8.000000000000000000, -2.494040418455211849, -18.62763138773853200 ) ) ;
#31021 = DIRECTION ( 'NONE',  ( 0.000000000000000000, 0.000000000000000000, 1.000000000000000000 ) ) ;
#31022 = DIRECTION ( 'NONE',  ( 0.000000000000000000, 0.000000000000000000, -1.000000000000000000 ) ) ;
#31023 = CARTESIAN_POINT ( 'NONE',  ( 0.000000000000000000, 0.000000000000000000, 0.000000000000000000 ) ) ;
#31024 = CYLINDRICAL_SURFACE ( 'NONE', #15096, 52.00000000000000711 ) ;
#31025 = ADVANCED_FACE ( 'NONE', ( #14035 ), #13872, .T. ) ;
#31026 = ORIENTED_EDGE ( 'NONE', *, *, #25553, .T. ) ;
#31027 = VECTOR ( 'NONE', #1980, 1000.000000000000114 ) ;
#31028 = LINE ( 'NONE', #8878, #13399 ) ;
#31029 = CARTESIAN_POINT ( 'NONE',  ( 3.799999999999999822, 0.000000000000000000, -53.39999999999999858 ) ) ;
#31030 = FACE_OUTER_BOUND ( 'NONE', #34744, .T. ) ;
#31031 = DIRECTION ( 'NONE',  ( 0.000000000000000000, 0.4999999999999989453, 0.8660254037844392627 ) ) ;
#31032 = ITEM_DEFINED_TRANSFORMATION ( 'NONE', 'NONE', #7523,  #21307 ) ;
#31033 = MECHANICAL_DESIGN_GEOMETRIC_PRESENTATION_REPRESENTATION (  '', ( #26451 ), #20087 ) ;
#31034 = PRODUCT_DEFINITION_FORMATION_WITH_SPECIFIED_SOURCE ( 'ANY', '', #12395, .NOT_KNOWN. ) ;
#31035 = CIRCLE ( 'NONE', #15501, 52.00000000000000711 ) ;
#31036 = CARTESIAN_POINT ( 'NONE',  ( 4.000000000000003553, 50.95304419620825342, 10.38206564895680017 ) ) ;
#31037 = CARTESIAN_POINT ( 'NONE',  ( 4.121423858225409909, -12.61643262889541894, -1.200000000000006617 ) ) ;
#31038 = ORIENTED_EDGE ( 'NONE', *, *, #1997, .T. ) ;
#31039 = DIRECTION ( 'NONE',  ( -1.000000000000000000, 0.000000000000000000, -0.000000000000000000 ) ) ;
#31040 = EDGE_CURVE ( 'NONE', #16592, #12885, #32962, .T. ) ;
#31041 = CYLINDRICAL_SURFACE ( 'NONE', #19960, 52.00000000000000711 ) ;
#31042 = LINE ( 'NONE', #23103, #23163 ) ;
#31043 = ORIENTED_EDGE ( 'NONE', *, *, #26925, .T. ) ;
#31044 = ORIENTED_EDGE ( 'NONE', *, *, #33602, .F. ) ;
#31045 = ADVANCED_FACE ( 'NONE', ( #17084 ), #17261, .T. ) ;
#31046 = CARTESIAN_POINT ( 'NONE',  ( -37.99999999999998579, -114.0592624029313242, 3.246475545821551734 ) ) ;
#31047 = EDGE_CURVE ( 'NONE', #11860, #23663, #24857, .T. ) ;
#31048 = ORIENTED_EDGE ( 'NONE', *, *, #33286, .F. ) ;
#31049 = EDGE_LOOP ( 'NONE', ( #32101, #17869, #7579, #26346, #13958 ) ) ;
#31050 = ORIENTED_EDGE ( 'NONE', *, *, #16639, .T. ) ;
#31051 = CARTESIAN_POINT ( 'NONE',  ( 0.000000000000000000, 39.55064067543064965, 25.36340625197373910 ) ) ;
#31052 = AXIS2_PLACEMENT_3D ( 'NONE', #30496, #27963, #33363 ) ;
#31053 = EDGE_CURVE ( 'NONE', #10066, #35092, #23619, .T. ) ;
#31054 = FACE_OUTER_BOUND ( 'NONE', #28295, .T. ) ;
#31055 = EDGE_CURVE ( 'NONE', #29036, #6031, #31094, .T. ) ;
#31056 = DIRECTION ( 'NONE',  ( -1.000000000000000000, 0.000000000000000000, 0.000000000000000000 ) ) ;
#31057 = AXIS2_PLACEMENT_3D ( 'NONE', #13157, #10077, #21044 ) ;
#31058 = CARTESIAN_POINT ( 'NONE',  ( -36.50000000000011369, -114.9929510916434339, 13.11852480586264669 ) ) ;
#31059 = CARTESIAN_POINT ( 'NONE',  ( 46.00000000000000000, 9.797174393178841435E-16, 78.00000000000001421 ) ) ;
#31060 = AXIS2_PLACEMENT_3D ( 'NONE', #255, #11242, #22211 ) ;
#31061 = VECTOR ( 'NONE', #34333, 1000.000000000000000 ) ;
#31062 = CARTESIAN_POINT ( 'NONE',  ( 0.000000000000000000, -36.05989434073634925, 30.12041790338604130 ) ) ;
#31063 = CARTESIAN_POINT ( 'NONE',  ( -34.50000000000000000, -114.9929510916434339, 10.61627146648203812 ) ) ;
#31064 = FACE_OUTER_BOUND ( 'NONE', #10629, .T. ) ;
#31065 = PRODUCT_DEFINITION_SHAPE ( 'NONE', 'NONE',  #3129 ) ;
#31066 = CARTESIAN_POINT ( 'NONE',  ( 7.999999999999992895, -19.44205635905512608, -43.33776004284631256 ) ) ;
#31067 = VERTEX_POINT ( 'NONE', #6294 ) ;
#31068 = CARTESIAN_POINT ( 'NONE',  ( -35.50000000000000000, -114.3049001878960240, 8.530677542735578101 ) ) ;
#31069 = CARTESIAN_POINT ( 'NONE',  ( -35.50000000000000711, -112.3465879560236687, 1.629585756119413364 ) ) ;
#31070 =( NAMED_UNIT ( * ) PLANE_ANGLE_UNIT ( ) SI_UNIT ( $, .RADIAN. ) );
#31071 = ADVANCED_FACE ( 'NONE', ( #33481 ), #25219, .F. ) ;
#31072 = DIRECTION ( 'NONE',  ( -1.000000000000000000, 0.000000000000000000, -0.000000000000000000 ) ) ;
#31073 = CARTESIAN_POINT ( 'NONE',  ( -10.00000000000000178, 0.000000000000000000, 0.000000000000000000 ) ) ;
#31074 = DIRECTION ( 'NONE',  ( -1.000000000000000000, 0.000000000000000000, 0.000000000000000000 ) ) ;
#31075 = ADVANCED_FACE ( 'NONE', ( #11353 ), #11521, .T. ) ;
#31076 = DIRECTION ( 'NONE',  ( -1.000000000000000000, 0.000000000000000000, 0.000000000000000000 ) ) ;
#31077 = DIRECTION ( 'NONE',  ( 0.000000000000000000, 0.000000000000000000, -1.000000000000000000 ) ) ;
#31078 = ORIENTED_EDGE ( 'NONE', *, *, #14688, .T. ) ;
#31079 = AXIS2_PLACEMENT_3D ( 'NONE', #22991, #17403, #1224 ) ;
#31080 = EDGE_CURVE ( 'NONE', #29170, #18178, #22142, .T. ) ;
#31081 = CARTESIAN_POINT ( 'NONE',  ( -36.52652403469559061, -114.9754527089670262, 7.277725545821552622 ) ) ;
#31082 = CARTESIAN_POINT ( 'NONE',  ( 3.160591952521676795, -3.281206521718066149, -0.7999999999999951594 ) ) ;
#31083 = FACE_BOUND ( 'NONE', #31712, .T. ) ;
#31084 = ORIENTED_EDGE ( 'NONE', *, *, #26381, .F. ) ;
#31085 = VERTEX_POINT ( 'NONE', #33137 ) ;
#31086 = CARTESIAN_POINT ( 'NONE',  ( -50.00000000000000000, 0.000000000000000000, 70.00000000000000000 ) ) ;
#31087 = DIRECTION ( 'NONE',  ( 0.000000000000000000, 0.000000000000000000, 1.000000000000000000 ) ) ;
#31088 = VERTEX_POINT ( 'NONE', #16734 ) ;
#31089 = EDGE_CURVE ( 'NONE', #12715, #1256, #8635, .T. ) ;
#31090 = CARTESIAN_POINT ( 'NONE',  ( -38.18337828418796676, -117.0245472910329738, 2.965225545821551734 ) ) ;
#31091 = ORIENTED_EDGE ( 'NONE', *, *, #21166, .F. ) ;
#31092 = CIRCLE ( 'NONE', #9830, 7.200000000000006395 ) ;
#31093 = ADVANCED_FACE ( 'NONE', ( #22662 ), #19770, .T. ) ;
#31094 = CIRCLE ( 'NONE', #46, 8.000000000000001776 ) ;
#31095 = DIRECTION ( 'NONE',  ( 0.000000000000000000, -0.5877852522924803536, 0.8090169943749422332 ) ) ;
#31096 = DIRECTION ( 'NONE',  ( 0.000000000000000000, 0.000000000000000000, 1.000000000000000000 ) ) ;
#31097 = APPLICATION_PROTOCOL_DEFINITION ( 'draft international standard', 'automotive_design', 1998, #16995 ) ;
#31098 = ADVANCED_FACE ( 'NONE', ( #30961 ), #17616, .T. ) ;
#31099 = DIRECTION ( 'NONE',  ( -1.000000000000000000, 5.339440136655842133E-16, 1.047965281155519420E-16 ) ) ;
#31100 = VERTEX_POINT ( 'NONE', #11869 ) ;
#31101 = ORIENTED_EDGE ( 'NONE', *, *, #24883, .F. ) ;
#31102 = DIRECTION ( 'NONE',  ( -1.000000000000000000, 0.000000000000000000, 0.000000000000000000 ) ) ;
#31103 = FACE_OUTER_BOUND ( 'NONE', #2907, .T. ) ;
#31104 = ORIENTED_EDGE ( 'NONE', *, *, #4310, .F. ) ;
#31105 = CARTESIAN_POINT ( 'NONE',  ( -4.000000000000000000, 0.000000000000000000, -44.50000000000000000 ) ) ;
#31106 = CARTESIAN_POINT ( 'NONE',  ( -34.50000000000000000, -113.1256619669233885, 1.895633585076891947 ) ) ;
#31107 = DIRECTION ( 'NONE',  ( 0.000000000000000000, 0.9848077530122084644, -0.1736481776669276389 ) ) ;
#31108 = DIRECTION ( 'NONE',  ( 0.000000000000000000, 0.000000000000000000, 1.000000000000000000 ) ) ;
#31109 = CARTESIAN_POINT ( 'NONE',  ( -34.50000000000000000, -115.9929510916434481, 10.55026311463432087 ) ) ;
#31110 = DIRECTION ( 'NONE',  ( -1.000000000000000000, 0.000000000000000000, 0.000000000000000000 ) ) ;
#31111 = DIRECTION ( 'NONE',  ( -1.000000000000000000, 0.000000000000000000, 0.000000000000000000 ) ) ;
#31112 = AXIS2_PLACEMENT_3D ( 'NONE', #12021, #28064, #34169 ) ;
#31113 = CARTESIAN_POINT ( 'NONE',  ( -38.98077402996267438, -114.9929510916434339, 12.86289566494346204 ) ) ;
#31115 = CARTESIAN_POINT ( 'NONE',  ( -39.49999999999999289, -9.059673409587547965, 113.4689433211305811 ) ) ;
#31114 = VECTOR ( 'NONE', #17794, 1000.000000000000000 ) ;
#31116 = ADVANCED_FACE ( 'NONE', ( #9527 ), #25751, .T. ) ;
#31117 = CARTESIAN_POINT ( 'NONE',  ( 8.000000000000000000, 0.000000000000000000, 0.000000000000000000 ) ) ;
#31118 = CARTESIAN_POINT ( 'NONE',  ( 7.999999999999992895, -36.05989434073634925, 30.12041790338604130 ) ) ;
#31119 = CYLINDRICAL_SURFACE ( 'NONE', #35366, 52.00000000000000711 ) ;
#31120 = ADVANCED_FACE ( 'NONE', ( #12049 ), #1429, .T. ) ;
#31121 = ORIENTED_EDGE ( 'NONE', *, *, #31673, .F. ) ;
#31122 = CARTESIAN_POINT ( 'NONE',  ( 0.000000000000000000, -10.15474465512038194, -9.637487275701211331 ) ) ;
#31123 = ORIENTED_EDGE ( 'NONE', *, *, #26243, .F. ) ;
#31124 = CARTESIAN_POINT ( 'NONE',  ( -36.94073759706866156, -111.0000000000000284, 8.628524454178448266 ) ) ;
#31125 = CARTESIAN_POINT ( 'NONE',  ( -34.49999999999998579, -17.72201855431907447, 96.30456345124113682 ) ) ;
#31126 = CARTESIAN_POINT ( 'NONE',  ( -35.50000000000000711, -116.0141056290913610, -0.5935324770972248976 ) ) ;
#31127 = VERTEX_POINT ( 'NONE', #15445 ) ;
#31128 = VERTEX_POINT ( 'NONE', #20667 ) ;
#31129 = DIRECTION ( 'NONE',  ( -1.000000000000000000, -0.000000000000000000, -0.000000000000000000 ) ) ;
#31130 = CARTESIAN_POINT ( 'NONE',  ( 8.000000000000007105, 0.000000000000000000, 0.000000000000000000 ) ) ;
#31131 = VERTEX_POINT ( 'NONE', #14915 ) ;
#31132 = EDGE_CURVE ( 'NONE', #28967, #13424, #5277, .T. ) ;
#31133 = ORIENTED_EDGE ( 'NONE', *, *, #35179, .T. ) ;
#31134 = EDGE_CURVE ( 'NONE', #6583, #26304, #35172, .T. ) ;
#31135 = LINE ( 'NONE', #25920, #3912 ) ;
#31136 = ORIENTED_EDGE ( 'NONE', *, *, #11021, .F. ) ;
#31137 = VERTEX_POINT ( 'NONE', #20306 ) ;
#31138 = CARTESIAN_POINT ( 'NONE',  ( -35.54388159064475872, -115.3723087153909432, 2.683975545821551290 ) ) ;
#31139 = AXIS2_PLACEMENT_3D ( 'NONE', #32083, #10475, #32434 ) ;
#31140 = CIRCLE ( 'NONE', #4721, 8.000000000000000000 ) ;
#31141 = DIRECTION ( 'NONE',  ( 0.000000000000000000, 0.000000000000000000, 1.000000000000000000 ) ) ;
#31142 = ORIENTED_EDGE ( 'NONE', *, *, #31543, .F. ) ;
#31143 = EDGE_LOOP ( 'NONE', ( #13565, #11291, #22362, #25769 ) ) ;
#31144 = CARTESIAN_POINT ( 'NONE',  ( -35.50000000000000000, -111.0780159515033034, -1.143161139953928762 ) ) ;
#31145 = CARTESIAN_POINT ( 'NONE',  ( -44.00199999999999534, 14.29999999999999893, 3.000000000000002665 ) ) ;
#31146 = ORIENTED_EDGE ( 'NONE', *, *, #21020, .F. ) ;
#31147 = DIRECTION ( 'NONE',  ( -1.000000000000000000, -0.000000000000000000, 0.000000000000000000 ) ) ;
#31148 = CARTESIAN_POINT ( 'NONE',  ( -38.99879592093640213, -113.9929510916434339, 12.67985367974111277 ) ) ;
#31149 = DIRECTION ( 'NONE',  ( -1.000000000000000000, 0.000000000000000000, 0.000000000000000000 ) ) ;
#31150 = CARTESIAN_POINT ( 'NONE',  ( 8.000000000000007105, 0.000000000000000000, 0.000000000000000000 ) ) ;
#31151 = CARTESIAN_POINT ( 'NONE',  ( -37.37500000000009237, -113.9929510916434339, 14.11852480586265024 ) ) ;
#31152 = CARTESIAN_POINT ( 'NONE',  ( 8.000000000000000000, -16.71027810728550733, 4.579731798933878828 ) ) ;
#31153 = CARTESIAN_POINT ( 'NONE',  ( -36.15625000000007816, -114.9929510916434339, 13.11852480586264669 ) ) ;
#31154 = DIRECTION ( 'NONE',  ( -1.000000000000000000, -0.000000000000000000, -0.000000000000000000 ) ) ;
#31155 = EDGE_LOOP ( 'NONE', ( #686, #30175, #12091, #32772 ) ) ;
#31156 = DIRECTION ( 'NONE',  ( 0.000000000000000000, 0.8443279255020161855, -0.5358267949789946583 ) ) ;
#31157 = DIRECTION ( 'NONE',  ( 1.000000000000000000, 0.000000000000000000, 0.000000000000000000 ) ) ;
#31158 = EDGE_CURVE ( 'NONE', #12983, #3192, #26533, .T. ) ;
#31159 = ORIENTED_EDGE ( 'NONE', *, *, #31158, .F. ) ;
#31160 = CARTESIAN_POINT ( 'NONE',  ( -35.50000000000000711, -114.9922651054798308, 10.46846006712531008 ) ) ;
#31161 = ORIENTED_EDGE ( 'NONE', *, *, #2042, .T. ) ;
#31162 = MECHANICAL_DESIGN_GEOMETRIC_PRESENTATION_REPRESENTATION (  '', ( #18512 ), #16782 ) ;
#31163 = AXIS2_PLACEMENT_3D ( 'NONE', #6387, #22940, #19864 ) ;
#31164 = DIRECTION ( 'NONE',  ( -1.000000000000000000, 0.000000000000000000, 0.000000000000000000 ) ) ;
#31165 = ORIENTED_EDGE ( 'NONE', *, *, #26861, .T. ) ;
#31166 = LINE ( 'NONE', #30987, #21632 ) ;
#31167 = ORIENTED_EDGE ( 'NONE', *, *, #21599, .F. ) ;
#31168 = CARTESIAN_POINT ( 'NONE',  ( -35.50000000000000000, -115.0140978167138712, 0.8752176474015623819 ) ) ;
#31169 = LINE ( 'NONE', #25060, #12146 ) ;
#31170 = CARTESIAN_POINT ( 'NONE',  ( -37.05926240293131713, -115.9999999999999858, 3.378524454178448710 ) ) ;
#31171 = ORIENTED_EDGE ( 'NONE', *, *, #7245, .T. ) ;
#31172 = CARTESIAN_POINT ( 'NONE',  ( -35.62769128460905677, -115.4561184093552413, 1.691024454178448710 ) ) ;
#31173 = VECTOR ( 'NONE', #30849, 1000.000000000000000 ) ;
#31174 = CARTESIAN_POINT ( 'NONE',  ( 8.000000000000000000, 6.071532165918824830E-15, 1.000000000000000000 ) ) ;
#31175 = CARTESIAN_POINT ( 'NONE',  ( -35.50000000000000711, -116.0140978167138712, -0.4997823525984418369 ) ) ;
#31176 = ORIENTED_EDGE ( 'NONE', *, *, #31215, .T. ) ;
#31177 = ORIENTED_EDGE ( 'NONE', *, *, #31405, .T. ) ;
#31178 = CIRCLE ( 'NONE', #29473, 4.800000000000002487 ) ;
#31179 = DIRECTION ( 'NONE',  ( -0.000000000000000000, 0.000000000000000000, -1.000000000000000000 ) ) ;
#31180 = CARTESIAN_POINT ( 'NONE',  ( 0.000000000000000000, -51.93417535146743802, 2.615612846549014492 ) ) ;
#31181 = ORIENTED_EDGE ( 'NONE', *, *, #35259, .T. ) ;
#31182 = ORIENTED_EDGE ( 'NONE', *, *, #4723, .F. ) ;
#31183 = CARTESIAN_POINT ( 'NONE',  ( -34.50000000000000000, -116.0124910254613297, -0.6902086197697608894 ) ) ;
#31184 = CARTESIAN_POINT ( 'NONE',  ( -35.50000000000000711, -112.3465879560236687, 1.629585756119413364 ) ) ;
#31185 = VECTOR ( 'NONE', #10841, 1000.000000000000000 ) ;
#31186 = EDGE_LOOP ( 'NONE', ( #24601, #7111, #16987, #22255 ) ) ;
#31187 = AXIS2_PLACEMENT_3D ( 'NONE', #21475, #23669, #10158 ) ;
#31188 = ORIENTED_EDGE ( 'NONE', *, *, #34379, .F. ) ;
#31189 = CYLINDRICAL_SURFACE ( 'NONE', #17757, 20.00000000000000711 ) ;
#31190 = CARTESIAN_POINT ( 'NONE',  ( -37.37500000000009237, -113.9929510916434339, 13.11852480586264846 ) ) ;
#31191 = CARTESIAN_POINT ( 'NONE',  ( -34.50000000000000000, -113.2637153405686519, 1.912112492696748989 ) ) ;
#31192 = DIRECTION ( 'NONE',  ( 0.000000000000000000, -6.994405055138476738E-15, 1.000000000000000000 ) ) ;
#31193 = CARTESIAN_POINT ( 'NONE',  ( -35.50000000000000000, -113.9929510916434339, 12.26648026267477398 ) ) ;
#31194 = CARTESIAN_POINT ( 'NONE',  ( -35.50040135968784938, -115.9929510916434481, 12.63896776382214071 ) ) ;
#31195 = UNCERTAINTY_MEASURE_WITH_UNIT (LENGTH_MEASURE( 1.000000000000000082E-05 ), #14468, 'distance_accuracy_value', 'NONE');
#31196 = DIRECTION ( 'NONE',  ( -1.000000000000000000, 0.000000000000000000, 0.000000000000000000 ) ) ;
#31197 = CIRCLE ( 'NONE', #26042, 52.00000000000000711 ) ;
#31198 = CARTESIAN_POINT ( 'NONE',  ( -34.49999999999998579, -25.98076211353322051, 84.99999999999992895 ) ) ;
#31199 = EDGE_CURVE ( 'NONE', #23286, #7406, #9168, .T. ) ;
#31200 = DIRECTION ( 'NONE',  ( -1.000000000000000000, 0.000000000000000000, 0.000000000000000000 ) ) ;
#31201 = CARTESIAN_POINT ( 'NONE',  ( 7.999999999999992895, 0.000000000000000000, 0.000000000000000000 ) ) ;
#31202 = DIRECTION ( 'NONE',  ( 0.000000000000000000, 0.000000000000000000, -1.000000000000000000 ) ) ;
#31203 = EDGE_LOOP ( 'NONE', ( #2368, #22870, #33528, #22518 ) ) ;
#31204 = DIRECTION ( 'NONE',  ( 0.000000000000000000, 0.000000000000000000, 1.000000000000000000 ) ) ;
#31205 = DIRECTION ( 'NONE',  ( -1.000000000000000000, 0.000000000000000000, 0.000000000000000000 ) ) ;
#31206 = VECTOR ( 'NONE', #2979, 1000.000000000000000 ) ;
#31207 = AXIS2_PLACEMENT_3D ( 'NONE', #24129, #32568, #7551 ) ;
#31208 = DIRECTION ( 'NONE',  ( -1.000000000000000000, 0.000000000000000000, 0.000000000000000000 ) ) ;
#31209 = CARTESIAN_POINT ( 'NONE',  ( 0.000000000000000000, 0.000000000000000000, 0.000000000000000000 ) ) ;
#31210 = EDGE_CURVE ( 'NONE', #24482, #2498, #34026, .T. ) ;
#31211 = VECTOR ( 'NONE', #29997, 1000.000000000000000 ) ;
#31212 = CYLINDRICAL_SURFACE ( 'NONE', #31928, 4.000000000000003553 ) ;
#31213 = DIRECTION ( 'NONE',  ( 0.000000000000000000, 0.000000000000000000, 1.000000000000000000 ) ) ;
#31214 = VERTEX_POINT ( 'NONE', #9877 ) ;
#31215 = EDGE_CURVE ( 'NONE', #16103, #15577, #6826, .T. ) ;
#31216 = SHAPE_REPRESENTATION ( 'spring', ( #21307 ), #12169 ) ;
#31217 = CARTESIAN_POINT ( 'NONE',  ( 7.999999999999992895, -27.79676263918213763, 37.88001506494759241 ) ) ;
#31218 = CARTESIAN_POINT ( 'NONE',  ( -34.50000000000000000, -116.9884631899972476, -0.9506101647064282290 ) ) ;
#31219 = CARTESIAN_POINT ( 'NONE',  ( -21.15833593587365513, -29.27980021920993536, 87.71410161513767889 ) ) ;
#31220 = ORIENTED_EDGE ( 'NONE', *, *, #33677, .F. ) ;
#31221 = ORIENTED_EDGE ( 'NONE', *, *, #24454, .F. ) ;
#31222 = CARTESIAN_POINT ( 'NONE',  ( -37.05926240293131713, -113.0000000000000000, 9.621475545821549957 ) ) ;
#31223 = ORIENTED_EDGE ( 'NONE', *, *, #32117, .F. ) ;
#31225 = ORIENTED_EDGE ( 'NONE', *, *, #5279, .F. ) ;
#31224 = CIRCLE ( 'NONE', #15685, 8.000000000000007105 ) ;
#31226 = ORIENTED_EDGE ( 'NONE', *, *, #3921, .F. ) ;
#31227 = DIRECTION ( 'NONE',  ( -1.000000000000000000, 0.000000000000000000, -0.000000000000000000 ) ) ;
#31228 = AXIS2_PLACEMENT_3D ( 'NONE', #31416, #15020, #21137 ) ;
#31229 = CARTESIAN_POINT ( 'NONE',  ( -35.50000000000000711, -116.0140978167138712, 0.3752176474015736507 ) ) ;
#31230 = ADVANCED_FACE ( 'NONE', ( #34388 ), #34200, .T. ) ;
#31231 = CARTESIAN_POINT ( 'NONE',  ( -42.49999999999999289, -25.98076211353322051, 84.99999999999992895 ) ) ;
#31232 = CIRCLE ( 'NONE', #11693, 3.799999999999999822 ) ;
#31233 = CARTESIAN_POINT ( 'NONE',  ( -35.98364338251434447, -114.9929510916434339, 13.11827392651456314 ) ) ;
#31234 = CIRCLE ( 'NONE', #15697, 20.00000000000000711 ) ;
#31235 = DIRECTION ( 'NONE',  ( 0.000000000000000000, -0.9048270524660235736, 0.4257792915650641663 ) ) ;
#31236 = AXIS2_PLACEMENT_3D ( 'NONE', #6026, #19169, #5334 ) ;
#31237 = CARTESIAN_POINT ( 'NONE',  ( 46.00000000000000000, 0.000000000000000000, 61.99999999999999289 ) ) ;
#31238 = CARTESIAN_POINT ( 'NONE',  ( -34.50000000000000000, -114.9929510916434339, 11.21034663311131929 ) ) ;
#31239 = CARTESIAN_POINT ( 'NONE',  ( 0.000000000000000000, -13.56094713063606072, 50.20060470671736397 ) ) ;
#31240 = ADVANCED_FACE ( 'NONE', ( #14741 ), #28796, .T. ) ;
#31241 = EDGE_CURVE ( 'NONE', #6425, #16937, #6468, .T. ) ;
#31242 = LINE ( 'NONE', #8912, #23794 ) ;
#31243 = EDGE_LOOP ( 'NONE', ( #22828, #20922 ) ) ;
#31244 = EDGE_CURVE ( 'NONE', #1732, #19003, #30549, .T. ) ;
#31245 = CARTESIAN_POINT ( 'NONE',  ( -35.50000000000000000, -115.9929510916434481, 10.72628538622835670 ) ) ;
#31246 = CARTESIAN_POINT ( 'NONE',  ( -35.50000000000000711, -114.0000000000000853, 2.000000000000001776 ) ) ;
#31247 = DIRECTION ( 'NONE',  ( -1.174092375852890260E-15, 4.222049128630259891E-16, 1.000000000000000000 ) ) ;
#31248 = CARTESIAN_POINT ( 'NONE',  ( -46.00000000000000000, -25.98076211353320275, 76.99999999999992895 ) ) ;
#31249 = VECTOR ( 'NONE', #14097, 1000.000000000000000 ) ;
#31250 = LINE ( 'NONE', #28554, #27411 ) ;
#31251 = FACE_OUTER_BOUND ( 'NONE', #14085, .T. ) ;
#31252 = DIRECTION ( 'NONE',  ( 0.000000000000000000, 1.000000000000000000, 0.000000000000000000 ) ) ;
#31253 = FACE_OUTER_BOUND ( 'NONE', #15207, .T. ) ;
#31254 = ORIENTED_EDGE ( 'NONE', *, *, #2012, .F. ) ;
#31255 = ADVANCED_FACE ( 'NONE', ( #20838, #28973 ), #28441, .F. ) ;
#31256 = CARTESIAN_POINT ( 'NONE',  ( -37.97545270896702618, -114.4734759653044023, 6.152725545821551734 ) ) ;
#31257 = CARTESIAN_POINT ( 'NONE',  ( 0.000000000000000000, 27.79676263918241119, -37.88001506494740056 ) ) ;
#31258 = DIRECTION ( 'NONE',  ( 0.000000000000000000, -0.000000000000000000, 1.000000000000000000 ) ) ;
#31259 = EDGE_CURVE ( 'NONE', #9289, #11649, #15266, .T. ) ;
#31260 = ORIENTED_EDGE ( 'NONE', *, *, #3063, .F. ) ;
#31261 = EDGE_LOOP ( 'NONE', ( #33006, #27289, #14301, #25160 ) ) ;
#31262 = CIRCLE ( 'NONE', #8835, 7.199999999999993960 ) ;
#31263 = VECTOR ( 'NONE', #29439, 1000.000000000000000 ) ;
#31264 = CARTESIAN_POINT ( 'NONE',  ( 7.999999999999992895, 49.25004636492389665, 16.68630974939777545 ) ) ;
#31265 = VERTEX_POINT ( 'NONE', #18154 ) ;
#31266 = CARTESIAN_POINT ( 'NONE',  ( -34.92058450342249643, -111.8367748094582197, 6.808975545821551734 ) ) ;
#31267 = ORIENTED_EDGE ( 'NONE', *, *, #16026, .T. ) ;
#31268 = DIRECTION ( 'NONE',  ( 0.000000000000000000, 0.9510565162951521989, 0.3090169943749514481 ) ) ;
#31269 = FACE_OUTER_BOUND ( 'NONE', #18241, .T. ) ;
#31270 = APPLICATION_PROTOCOL_DEFINITION ( 'draft international standard', 'automotive_design', 1998, #18159 ) ;
#31271 = EDGE_CURVE ( 'NONE', #4101, #17645, #69, .T. ) ;
#31272 = CARTESIAN_POINT ( 'NONE',  ( 0.000000000000000000, 0.000000000000000000, 0.000000000000000000 ) ) ;
#31273 = ORIENTED_EDGE ( 'NONE', *, *, #24871, .T. ) ;
#31274 = ORIENTED_EDGE ( 'NONE', *, *, #24082, .F. ) ;
#31275 = AXIS2_PLACEMENT_3D ( 'NONE', #22551, #16795, #33024 ) ;
#31276 = LINE ( 'NONE', #4468, #17938 ) ;
#31277 = LINE ( 'NONE', #25528, #30103 ) ;
#31278 = ORIENTED_EDGE ( 'NONE', *, *, #8852, .T. ) ;
#31279 = DIRECTION ( 'NONE',  ( 1.000000000000000000, 0.000000000000000000, 0.000000000000000000 ) ) ;
#31280 = CARTESIAN_POINT ( 'NONE',  ( -34.50000000000000000, -112.6605569508015350, 1.812590711673265575 ) ) ;
#31281 = CARTESIAN_POINT ( 'NONE',  ( 8.000000000000000000, -9.471478019455243924, 14.71414642875952161 ) ) ;
#31282 = DIRECTION ( 'NONE',  ( 0.000000000000000000, 0.000000000000000000, 1.000000000000000000 ) ) ;
#31283 = CIRCLE ( 'NONE', #11164, 47.49900000000003075 ) ;
#31284 = CARTESIAN_POINT ( 'NONE',  ( -34.50000000000000000, -114.1928420708668028, 8.515919878418792166 ) ) ;
#31285 = EDGE_CURVE ( 'NONE', #11684, #8621, #32381, .T. ) ;
#31286 = AXIS2_PLACEMENT_3D ( 'NONE', #9897, #23414, #15109 ) ;
#31287 = EDGE_CURVE ( 'NONE', #25221, #580, #7544, .T. ) ;
#31288 = CARTESIAN_POINT ( 'NONE',  ( 0.000000000000000000, -35.11945359308084846, -38.34871548466050939 ) ) ;
#31289 = CARTESIAN_POINT ( 'NONE',  ( 0.000000000000000000, -11.46872990052349550, -45.56340405422456996 ) ) ;
#31290 = ADVANCED_FACE ( 'NONE', ( #35106 ), #15795, .T. ) ;
#31291 = CARTESIAN_POINT ( 'NONE',  ( -38.69949915733018742, -114.9929510916434339, 13.54034599209165712 ) ) ;
#31292 = LINE ( 'NONE', #33454, #988 ) ;
#31293 = DIRECTION ( 'NONE',  ( 0.000000000000000000, 0.000000000000000000, -1.000000000000000000 ) ) ;
#31294 = DIRECTION ( 'NONE',  ( -1.000000000000000000, 0.000000000000000000, -0.000000000000000000 ) ) ;
#31295 = FACE_OUTER_BOUND ( 'NONE', #34417, .T. ) ;
#31296 = DIRECTION ( 'NONE',  ( 0.000000000000000000, 0.1253332335643046747, -0.9921147013144777649 ) ) ;
#31297 = ORIENTED_EDGE ( 'NONE', *, *, #7988, .T. ) ;
#31298 = CARTESIAN_POINT ( 'NONE',  ( -33.97545270896702618, -112.8166217158120475, 8.909774454178450043 ) ) ;
#31299 = CARTESIAN_POINT ( 'NONE',  ( 50.00000000000000711, 0.000000000000000000, 0.000000000000000000 ) ) ;
#31300 = CARTESIAN_POINT ( 'NONE',  ( -35.50000000000000000, -113.0140978167138712, -0.1247823525984260717 ) ) ;
#31301 = EDGE_CURVE ( 'NONE', #17702, #33466, #1803, .T. ) ;
#31302 = ORIENTED_EDGE ( 'NONE', *, *, #9748, .F. ) ;
#31303 = ORIENTED_EDGE ( 'NONE', *, *, #22089, .F. ) ;
#31304 = DIRECTION ( 'NONE',  ( -1.783119874454246424E-31, -1.187911941725854497E-31, 1.000000000000000000 ) ) ;
#31305 = CARTESIAN_POINT ( 'NONE',  ( 5.400000000000071410, 0.9999999999999662492, -44.50000000000000000 ) ) ;
#31306 = VERTEX_POINT ( 'NONE', #23933 ) ;
#31307 = ORIENTED_EDGE ( 'NONE', *, *, #31604, .F. ) ;
#31308 = VECTOR ( 'NONE', #29824, 1000.000000000000000 ) ;
#31309 = DIRECTION ( 'NONE',  ( -1.000000000000000000, 0.000000000000000000, 0.000000000000000000 ) ) ;
#31310 = AXIS2_PLACEMENT_3D ( 'NONE', #160, #25547, #24836 ) ;
#31311 = ORIENTED_EDGE ( 'NONE', *, *, #12761, .F. ) ;
#31312 = CARTESIAN_POINT ( 'NONE',  ( -38.45611840935523418, -112.6276912846090568, 3.433975545821551290 ) ) ;
#31313 = FILL_AREA_STYLE ('',( #6467 ) ) ;
#31314 = EDGE_CURVE ( 'NONE', #25823, #24996, #1794, .T. ) ;
#31315 = CIRCLE ( 'NONE', #16338, 15.49899999999999878 ) ;
#31316 = CARTESIAN_POINT ( 'NONE',  ( -10.00000000000000000, 0.000000000000000000, 0.000000000000000000 ) ) ;
#31317 = ORIENTED_EDGE ( 'NONE', *, *, #12113, .T. ) ;
#31318 = EDGE_LOOP ( 'NONE', ( #7017, #23307, #11691, #16676 ) ) ;
#31319 = CARTESIAN_POINT ( 'NONE',  ( -35.50000000000000000, -117.0140978167138854, -0.3122823525984416149 ) ) ;
#31320 = EDGE_CURVE ( 'NONE', #12885, #180, #27684, .T. ) ;
#31321 = EDGE_CURVE ( 'NONE', #14882, #2210, #4853, .T. ) ;
#31322 = FACE_OUTER_BOUND ( 'NONE', #24368, .T. ) ;
#31323 = ORIENTED_EDGE ( 'NONE', *, *, #7085, .T. ) ;
#31324 = CARTESIAN_POINT ( 'NONE',  ( -38.00000000000000711, -114.9929510916434339, 10.85830208992306822 ) ) ;
#31325 = CARTESIAN_POINT ( 'NONE',  ( -34.50000000000000000, -114.0882517521923489, 9.510534276948430232 ) ) ;
#31326 = DIRECTION ( 'NONE',  ( -1.000000000000000000, -1.734723475976807094E-16, 0.000000000000000000 ) ) ;
#31327 = EDGE_CURVE ( 'NONE', #18878, #22481, #14441, .T. ) ;
#31328 = LINE ( 'NONE', #14754, #26630 ) ;
#31329 = EDGE_CURVE ( 'NONE', #20180, #20307, #23746, .T. ) ;
#31330 = CARTESIAN_POINT ( 'NONE',  ( -38.95206139890799335, -113.9929510916434339, 13.00730889637963550 ) ) ;
#31331 = DIRECTION ( 'NONE',  ( -1.000000000000000000, -0.000000000000000000, 0.000000000000000000 ) ) ;
#31332 = CARTESIAN_POINT ( 'NONE',  ( -36.62499999999902656, -114.9929510916434339, 13.11852480586264669 ) ) ;
#31333 = PLANE ( 'NONE',  #32545 ) ;
#31334 = ORIENTED_EDGE ( 'NONE', *, *, #8194, .T. ) ;
#31336 = AXIS2_PLACEMENT_3D ( 'NONE', #34850, #17730, #15373 ) ;
#31335 = DIRECTION ( 'NONE',  ( 0.000000000000000000, 0.000000000000000000, -1.000000000000000000 ) ) ;
#31337 = CARTESIAN_POINT ( 'NONE',  ( 7.999999999999992895, 19.74581912682909390, -48.10512059033372623 ) ) ;
#31338 = CIRCLE ( 'NONE', #15791, 19.99999999999998579 ) ;
#31339 = EDGE_LOOP ( 'NONE', ( #31683, #1131, #8418, #30587 ) ) ;
#31340 = CARTESIAN_POINT ( 'NONE',  ( -35.50000000000000711, -114.9929296450195721, 10.49869535309826674 ) ) ;
#31341 = ORIENTED_EDGE ( 'NONE', *, *, #34208, .T. ) ;
#31342 = CARTESIAN_POINT ( 'NONE',  ( 8.000000000000000000, -8.605879768205326741, 12.89022243466705930 ) ) ;
#31343 = AXIS2_PLACEMENT_3D ( 'NONE', #16137, #21728, #27155 ) ;
#31344 = EDGE_LOOP ( 'NONE', ( #22100, #34962, #4235, #5424, #35280, #4503, #3388, #30925, #10856, #26712, #3276, #35287 ) ) ;
#31345 = DIRECTION ( 'NONE',  ( 0.000000000000000000, 0.000000000000000000, -1.000000000000000000 ) ) ;
#31346 = EDGE_LOOP ( 'NONE', ( #35540, #20915, #16148, #13225 ) ) ;
#31347 = CARTESIAN_POINT ( 'NONE',  ( -35.50000000000000000, -113.4307644833805142, -0.6247823525984269599 ) ) ;
#31348 = DIRECTION ( 'NONE',  ( 1.000000000000000000, -5.339440136655843119E-16, 0.000000000000000000 ) ) ;
#31349 = DIRECTION ( 'NONE',  ( -1.000000000000000000, 0.000000000000000000, 0.000000000000000000 ) ) ;
#31350 = ORIENTED_EDGE ( 'NONE', *, *, #1753, .T. ) ;
#31351 = CARTESIAN_POINT ( 'NONE',  ( -38.99999999999999289, -113.9407375970686900, 2.253524454178449155 ) ) ;
#31352 = AXIS2_PLACEMENT_3D ( 'NONE', #25588, #11707, #30979 ) ;
#31353 = CARTESIAN_POINT ( 'NONE',  ( 5.400000000000015454, -1.000000000000002220, -22.00000000000000000 ) ) ;
#31354 = CARTESIAN_POINT ( 'NONE',  ( -35.50000000000000711, -115.8137639216009234, -1.239329810084483841 ) ) ;
#31355 = ORIENTED_EDGE ( 'NONE', *, *, #23562, .T. ) ;
#31356 = ORIENTED_EDGE ( 'NONE', *, *, #2075, .T. ) ;
#31357 = FACE_OUTER_BOUND ( 'NONE', #23824, .T. ) ;
#31358 = EDGE_CURVE ( 'NONE', #4138, #21338, #1971, .T. ) ;
#31359 = DIRECTION ( 'NONE',  ( 0.000000000000000000, 0.000000000000000000, 1.000000000000000000 ) ) ;
#31360 = VERTEX_POINT ( 'NONE', #34737 ) ;
#31361 = ORIENTED_EDGE ( 'NONE', *, *, #8351, .F. ) ;
#31362 = CARTESIAN_POINT ( 'NONE',  ( -34.50000000000000000, -115.0468226098135744, -1.624774171496087716 ) ) ;
#31363 = LINE ( 'NONE', #3837, #21212 ) ;
#31364 = ADVANCED_FACE ( 'NONE', ( #21025 ), #8063, .T. ) ;
#31365 = PRODUCT_DEFINITION_SHAPE ( 'NONE', 'NONE',  #35620 ) ;
#31366 = CIRCLE ( 'NONE', #7226, 15.49899999999999167 ) ;
#31367 = ORIENTED_EDGE ( 'NONE', *, *, #21969, .T. ) ;
#31368 = VERTEX_POINT ( 'NONE', #10429 ) ;
#31369 = LINE ( 'NONE', #35508, #2863 ) ;
#31370 = VECTOR ( 'NONE', #13422, 1000.000000000000000 ) ;
#31371 = AXIS2_PLACEMENT_3D ( 'NONE', #33884, #17304, #2955 ) ;
#31372 = CARTESIAN_POINT ( 'NONE',  ( -35.98364338251434447, -113.9929510916434339, 13.11827392651456314 ) ) ;
#31373 = FACE_OUTER_BOUND ( 'NONE', #18740, .T. ) ;
#31374 = CARTESIAN_POINT ( 'NONE',  ( -35.50000000000000000, -113.9929510916434339, 12.60752341388803721 ) ) ;
#31375 = CARTESIAN_POINT ( 'NONE',  ( -35.50000000000000000, -115.9874658933321001, 10.35517832894335832 ) ) ;
#31376 = AXIS2_PLACEMENT_3D ( 'NONE', #34041, #6311, #23226 ) ;
#31377 = DIRECTION ( 'NONE',  ( -0.000000000000000000, 0.000000000000000000, -1.000000000000000000 ) ) ;
#31378 = FACE_OUTER_BOUND ( 'NONE', #6677, .T. ) ;
#31379 = CARTESIAN_POINT ( 'NONE',  ( 0.000000000000000000, 47.22458491092820765, 5.098390039074404356 ) ) ;
#31380 = CARTESIAN_POINT ( 'NONE',  ( 70.00000000000001421, 54.25778039068027425, 73.39034659349927381 ) ) ;
#31381 = DIRECTION ( 'NONE',  ( 0.000000000000000000, 0.000000000000000000, -1.000000000000000000 ) ) ;
#31382 = EDGE_LOOP ( 'NONE', ( #21471, #16811, #7574, #30392 ) ) ;
#31383 = DIRECTION ( 'NONE',  ( -1.000000000000000000, -0.000000000000000000, 0.000000000000000000 ) ) ;
#31384 = AXIS2_PLACEMENT_3D ( 'NONE', #27769, #19630, #5281 ) ;
#31385 = DIRECTION ( 'NONE',  ( 1.000000000000000000, -0.000000000000000000, 0.000000000000000000 ) ) ;
#31386 = DIRECTION ( 'NONE',  ( -1.000000000000000000, 0.000000000000000000, 0.000000000000000000 ) ) ;
#31387 = ITEM_DEFINED_TRANSFORMATION ( 'NONE', 'NONE', #29386,  #21307 ) ;
#31388 = CARTESIAN_POINT ( 'NONE',  ( 30.00000000000000711, -44.99999999999997868, 0.000000000000000000 ) ) ;
#31389 = FACE_OUTER_BOUND ( 'NONE', #10625, .T. ) ;
#31390 = VECTOR ( 'NONE', #10325, 1000.000000000000000 ) ;
#31391 = ORIENTED_EDGE ( 'NONE', *, *, #24415, .F. ) ;
#31392 = AXIS2_PLACEMENT_3D ( 'NONE', #3549, #25158, #6061 ) ;
#31393 = CARTESIAN_POINT ( 'NONE',  ( 8.000000000000000000, 18.62763138773855687, 2.494040418455418351 ) ) ;
#31394 = CARTESIAN_POINT ( 'NONE',  ( -34.50000000000000000, -114.9307644833806137, -2.624782352598442614 ) ) ;
#31395 = DIRECTION ( 'NONE',  ( 0.000000000000000000, -0.8660254037844368202, -0.5000000000000031086 ) ) ;
#31396 = VERTEX_POINT ( 'NONE', #21388 ) ;
#31397 = ORIENTED_EDGE ( 'NONE', *, *, #7741, .F. ) ;
#31398 = CARTESIAN_POINT ( 'NONE',  ( -35.99999999999999289, -114.0592624029313242, 1.503524454178448710 ) ) ;
#31399 = ORIENTED_EDGE ( 'NONE', *, *, #4035, .F. ) ;
#31400 = CIRCLE ( 'NONE', #17012, 12.55910585664918422 ) ;
#31401 = AXIS2_PLACEMENT_3D ( 'NONE', #5234, #14016, #25009 ) ;
#31402 = ORIENTED_EDGE ( 'NONE', *, *, #23135, .T. ) ;
#31403 = EDGE_LOOP ( 'NONE', ( #30011, #25957, #5167, #26542 ) ) ;
#31404 = CARTESIAN_POINT ( 'NONE',  ( -34.50000000000000000, -114.1185248058627053, 1.007048908356900085 ) ) ;
#31405 = EDGE_CURVE ( 'NONE', #1847, #1074, #5215, .T. ) ;
#31406 = FACE_OUTER_BOUND ( 'NONE', #32906, .T. ) ;
#31407 = CARTESIAN_POINT ( 'NONE',  ( 8.000000000000000000, -17.56975900509168298, -9.555290079479430432 ) ) ;
#31408 = VECTOR ( 'NONE', #33337, 1000.000000000000000 ) ;
#31409 = CARTESIAN_POINT ( 'NONE',  ( -35.50000000000000711, -114.9929510916434339, 12.17846912687782712 ) ) ;
#31410 = FACE_OUTER_BOUND ( 'NONE', #34043, .T. ) ;
#31411 = ADVANCED_FACE ( 'NONE', ( #13311 ), #29685, .T. ) ;
#31412 = DIRECTION ( 'NONE',  ( -1.000000000000000000, -0.000000000000000000, -0.000000000000000000 ) ) ;
#31413 = VECTOR ( 'NONE', #18931, 1000.000000000000000 ) ;
#31414 = VECTOR ( 'NONE', #33414, 1000.000000000000000 ) ;
#31415 = CARTESIAN_POINT ( 'NONE',  ( -37.43749999999998579, -114.9929510916434339, 14.11852480586264846 ) ) ;
#31416 = CARTESIAN_POINT ( 'NONE',  ( 0.000000000000000000, -27.79676263918213763, 37.88001506494759241 ) ) ;
#31417 = AXIS2_PLACEMENT_3D ( 'NONE', #25467, #786, #22744 ) ;
#31418 = AXIS2_PLACEMENT_3D ( 'NONE', #30893, #31426, #25680 ) ;
#31419 = DIRECTION ( 'NONE',  ( 0.000000000000000000, 0.8660254037844350439, 0.5000000000000061062 ) ) ;
#31420 = ORIENTED_EDGE ( 'NONE', *, *, #34295, .F. ) ;
#31421 = CARTESIAN_POINT ( 'NONE',  ( -35.50000000000000000, -115.9920935318519923, 10.44577481630138749 ) ) ;
#31422 = CARTESIAN_POINT ( 'NONE',  ( -35.50000000000000711, -112.0140978167138712, -0.1247823525984259746 ) ) ;
#31423 = SURFACE_STYLE_FILL_AREA ( #26199 ) ;
#31424 = CIRCLE ( 'NONE', #15889, 22.00000000000000000 ) ;
#31425 = DIRECTION ( 'NONE',  ( -1.000000000000000000, 5.339440136655861854E-16, 0.000000000000000000 ) ) ;
#31426 = DIRECTION ( 'NONE',  ( -1.000000000000000000, -0.000000000000000000, 0.000000000000000000 ) ) ;
#31427 = AXIS2_PLACEMENT_3D ( 'NONE', #22593, #28024, #3372 ) ;
#31428 = DIRECTION ( 'NONE',  ( 1.000000000000000000, 0.000000000000000000, 0.000000000000000000 ) ) ;
#31429 = CARTESIAN_POINT ( 'NONE',  ( -50.00000000000000000, -2.775557561562891351E-14, 106.0000000000000000 ) ) ;
#31430 = SHAPE_REPRESENTATION ( 'instrument roller bearing_iso_ISO 1224 - 180816 - R,14,SI,NC,14', ( #21307 ), #32842 ) ;
#31431 = CARTESIAN_POINT ( 'NONE',  ( 2.000000000000001332, 3.278627369596165408E-16, 4.725000000000016520 ) ) ;
#31432 = CARTESIAN_POINT ( 'NONE',  ( 8.000000000000007105, -13.42368113696669418, 3.975523202427999614 ) ) ;
#31433 = VERTEX_POINT ( 'NONE', #26641 ) ;
#31434 = CARTESIAN_POINT ( 'NONE',  ( -38.02454729103295961, -113.6450488405582462, 6.340225545821551734 ) ) ;
#31435 = LINE ( 'NONE', #9464, #10661 ) ;
#31436 = DIRECTION ( 'NONE',  ( 0.000000000000000000, -0.8660254037844410391, 0.4999999999999958367 ) ) ;
#31437 = ORIENTED_EDGE ( 'NONE', *, *, #15901, .F. ) ;
#31438 = AXIS2_PLACEMENT_3D ( 'NONE', #19744, #17233, #33819 ) ;
#31439 = EDGE_LOOP ( 'NONE', ( #31341, #26449, #34615, #8504 ) ) ;
#31440 = CARTESIAN_POINT ( 'NONE',  ( -42.49999999999999289, -25.27980021920979326, 80.78589838486217900 ) ) ;
#31441 = CYLINDRICAL_SURFACE ( 'NONE', #19217, 20.00000000000000355 ) ;
#31442 = ORIENTED_EDGE ( 'NONE', *, *, #16521, .T. ) ;
#31443 = CARTESIAN_POINT ( 'NONE',  ( -39.99999999999999289, -114.0592624029313242, 7.746475545821553510 ) ) ;
#31444 = ORIENTED_EDGE ( 'NONE', *, *, #6242, .T. ) ;
#31445 = AXIS2_PLACEMENT_3D ( 'NONE', #33860, #31154, #20148 ) ;
#31446 = CIRCLE ( 'NONE', #26862, 20.00000000000000355 ) ;
#31447 = DIRECTION ( 'NONE',  ( 1.000000000000000000, 0.000000000000000000, 0.000000000000000000 ) ) ;
#31448 = CIRCLE ( 'NONE', #23400, 4.000000000000000000 ) ;
#31449 = DIRECTION ( 'NONE',  ( 0.000000000000000000, 0.000000000000000000, -1.000000000000000000 ) ) ;
#31450 = EDGE_CURVE ( 'NONE', #933, #11196, #19053, .T. ) ;
#31451 = EDGE_CURVE ( 'NONE', #35346, #8923, #7885, .T. ) ;
#31452 = FACE_OUTER_BOUND ( 'NONE', #23694, .T. ) ;
#31453 = CIRCLE ( 'NONE', #23007, 47.49900000000001654 ) ;
#31454 = ITEM_DEFINED_TRANSFORMATION ( 'NONE', 'NONE', #21310,  #21307 ) ;
#31455 = FACE_OUTER_BOUND ( 'NONE', #28546, .T. ) ;
#31456 = VERTEX_POINT ( 'NONE', #2511 ) ;
#31457 = ORIENTED_EDGE ( 'NONE', *, *, #4084, .T. ) ;
#31458 = CARTESIAN_POINT ( 'NONE',  ( 70.00001200000001234, -29.47590766695025266, 87.01447592148352328 ) ) ;
#31459 = CARTESIAN_POINT ( 'NONE',  ( 0.000000000000000000, 0.000000000000000000, 0.000000000000000000 ) ) ;
#31460 = ADVANCED_FACE ( 'NONE', ( #13478 ), #24460, .F. ) ;
#31461 = VERTEX_POINT ( 'NONE', #5730 ) ;
#31462 = CYLINDRICAL_SURFACE ( 'NONE', #416, 52.00000000000000711 ) ;
#31463 = ADVANCED_FACE ( 'NONE', ( #21922 ), #8940, .T. ) ;
#31464 = CARTESIAN_POINT ( 'NONE',  ( -34.50000000000000000, -115.0304602784513293, -0.6247823525985405357 ) ) ;
#31465 = DIRECTION ( 'NONE',  ( 1.000000000000000000, -5.339440136655842133E-16, -1.047965281155519420E-16 ) ) ;
#31466 = DIRECTION ( 'NONE',  ( -1.000000000000000000, 0.000000000000000000, 0.000000000000000000 ) ) ;
#31467 = CARTESIAN_POINT ( 'NONE',  ( -34.57658136524561598, -115.9929510916434481, 13.10177712753338675 ) ) ;
#31468 = CIRCLE ( 'NONE', #34326, 20.00000000000000711 ) ;
#31469 = DIRECTION ( 'NONE',  ( 0.000000000000000000, -0.2538061376417690140, -0.9672551082808337197 ) ) ;
#31470 = CARTESIAN_POINT ( 'NONE',  ( 7.999999999999992895, 18.53613841426789932, 48.58406706613910586 ) ) ;
#31471 = CARTESIAN_POINT ( 'NONE',  ( -34.50000000000000000, -114.1835524127412924, 8.514811007161055656 ) ) ;
#31472 = DIRECTION ( 'NONE',  ( -1.000000000000000000, 0.000000000000000000, 0.000000000000000000 ) ) ;
#31473 = VECTOR ( 'NONE', #29123, 1000.000000000000000 ) ;
#31474 = AXIS2_PLACEMENT_3D ( 'NONE', #22920, #28334, #11589 ) ;
#31475 = PLANE ( 'NONE',  #33369 ) ;
#31476 = CIRCLE ( 'NONE', #21160, 15.49899999999998279 ) ;
#31477 = CARTESIAN_POINT ( 'NONE',  ( 8.000000000000000000, -17.47118961583598917, -0.9861715913089493801 ) ) ;
#31478 = CARTESIAN_POINT ( 'NONE',  ( -3.799999999999999822, 4.382607293638566128E-16, -30.90000000000000568 ) ) ;
#31479 = VECTOR ( 'NONE', #31966, 1000.000000000000000 ) ;
#31480 = CARTESIAN_POINT ( 'NONE',  ( 0.000000000000000000, 0.000000000000000000, 0.000000000000000000 ) ) ;
#31481 = ORIENTED_EDGE ( 'NONE', *, *, #3606, .F. ) ;
#31482 = CARTESIAN_POINT ( 'NONE',  ( -39.99999999999999289, -114.0592624029313242, 6.246475545821551734 ) ) ;
#31483 = AXIS2_PLACEMENT_3D ( 'NONE', #13341, #2727, #22128 ) ;
#31484 = FACE_OUTER_BOUND ( 'NONE', #5834, .T. ) ;
#31485 = EDGE_CURVE ( 'NONE', #10090, #24596, #19561, .T. ) ;
#31486 = CARTESIAN_POINT ( 'NONE',  ( -35.50000000000000000, -113.0140978167134449, 0.8752176474011410523 ) ) ;
#31487 = ORIENTED_EDGE ( 'NONE', *, *, #29564, .F. ) ;
#31488 = ORIENTED_EDGE ( 'NONE', *, *, #9541, .F. ) ;
#31489 = CARTESIAN_POINT ( 'NONE',  ( 8.000000000000000000, 0.000000000000000000, 0.000000000000000000 ) ) ;
#31490 = DIRECTION ( 'NONE',  ( -1.000000000000000000, 0.000000000000000000, -0.000000000000000000 ) ) ;
#31491 = ORIENTED_EDGE ( 'NONE', *, *, #33524, .F. ) ;
#31492 = ORIENTED_EDGE ( 'NONE', *, *, #9630, .F. ) ;
#31493 = ORIENTED_EDGE ( 'NONE', *, *, #66, .T. ) ;
#31494 = CIRCLE ( 'NONE', #17100, 9.499000000000004107 ) ;
#31495 = VECTOR ( 'NONE', #23533, 1000.000000000000000 ) ;
#31496 = EDGE_CURVE ( 'NONE', #2828, #30730, #16689, .T. ) ;
#31497 = DIRECTION ( 'NONE',  ( 1.000000000000000000, -1.110223024625156540E-16, 0.000000000000000000 ) ) ;
#31498 = ADVANCED_FACE ( 'NONE', ( #17041 ), #499, .T. ) ;
#31499 = CARTESIAN_POINT ( 'NONE',  ( -38.97545270896704039, -114.8876895276775087, 7.652725545821550845 ) ) ;
#31500 = EDGE_CURVE ( 'NONE', #30478, #25573, #5857, .T. ) ;
#31501 = DIRECTION ( 'NONE',  ( 0.000000000000000000, 0.9980267284282717810, -0.06279051952930997382 ) ) ;
#31502 = VERTEX_POINT ( 'NONE', #22979 ) ;
#31503 = ORIENTED_EDGE ( 'NONE', *, *, #11946, .F. ) ;
#31504 = CARTESIAN_POINT ( 'NONE',  ( -35.50000000000000000, -114.5974311500472567, -2.624782352598442614 ) ) ;
#31505 = CIRCLE ( 'NONE', #15960, 52.00000000000000711 ) ;
#31506 = CARTESIAN_POINT ( 'NONE',  ( 8.000000000000000000, -10.46102064772325413, -19.35373470438994303 ) ) ;
#31507 = ADVANCED_FACE ( 'NONE', ( #19727 ), #27700, .T. ) ;
#31508 = DIRECTION ( 'NONE',  ( -1.000000000000000000, 0.000000000000000000, 0.000000000000000000 ) ) ;
#31509 = ORIENTED_EDGE ( 'NONE', *, *, #25810, .F. ) ;
#31510 = PRESENTATION_LAYER_ASSIGNMENT (  '', '', ( #22884 ) ) ;
#31511 = CARTESIAN_POINT ( 'NONE',  ( -38.00000000000000711, -114.9929510916434339, 12.53051367006571937 ) ) ;
#31512 = ADVANCED_FACE ( 'NONE', ( #14174 ), #19398, .T. ) ;
#31513 = CARTESIAN_POINT ( 'NONE',  ( -34.50000000000000000, -114.1152303497977414, 9.513755561829650986 ) ) ;
#31514 = DIRECTION ( 'NONE',  ( 0.000000000000000000, 0.000000000000000000, 1.000000000000000000 ) ) ;
#31515 = CARTESIAN_POINT ( 'NONE',  ( 0.000000000000000000, 0.000000000000000000, 45.00000000000000711 ) ) ;
#31516 = CARTESIAN_POINT ( 'NONE',  ( -38.92341863475394348, -113.9929510916434339, 13.10177712753322155 ) ) ;
#31517 = LINE ( 'NONE', #31152, #30844 ) ;
#31518 = CARTESIAN_POINT ( 'NONE',  ( -35.50000102263782509, -114.9929510916434339, 12.62466071271731316 ) ) ;
#31519 =( NAMED_UNIT ( * ) PLANE_ANGLE_UNIT ( ) SI_UNIT ( $, .RADIAN. ) );
#31520 = ORIENTED_EDGE ( 'NONE', *, *, #34780, .F. ) ;
#31521 = DIRECTION ( 'NONE',  ( -1.000000000000000000, 0.000000000000000000, 0.000000000000000000 ) ) ;
#31522 = CARTESIAN_POINT ( 'NONE',  ( 8.000000000000007105, 9.604183132802424083, -5.908880290975567995 ) ) ;
#31523 = ORIENTED_EDGE ( 'NONE', *, *, #2822, .T. ) ;
#31524 = CARTESIAN_POINT ( 'NONE',  ( -35.50000000000000711, -114.9929510916434339, 10.59426868253284226 ) ) ;
#31525 = ORIENTED_EDGE ( 'NONE', *, *, #24958, .F. ) ;
#31526 = EDGE_CURVE ( 'NONE', #34823, #24024, #21930, .T. ) ;
#31527 = EDGE_LOOP ( 'NONE', ( #30219, #9160, #23864, #19562 ) ) ;
#31528 = VECTOR ( 'NONE', #6958, 1000.000000000000000 ) ;
#31529 = CARTESIAN_POINT ( 'NONE',  ( 0.1085714285714300953, -3.798448662927791819, -0.7999999999999951594 ) ) ;
#31530 = VERTEX_POINT ( 'NONE', #33607 ) ;
#31531 = CARTESIAN_POINT ( 'NONE',  ( -34.50000000000000000, -113.4742757288593964, 0.9301473394660054739 ) ) ;
#31532 = CARTESIAN_POINT ( 'NONE',  ( 0.000000000000000000, 0.000000000000000000, 60.90000000000001279 ) ) ;
#31533 = EDGE_CURVE ( 'NONE', #17480, #33223, #29428, .T. ) ;
#31534 = CARTESIAN_POINT ( 'NONE',  ( -4.000000000000000000, -2.710505431213761085E-17, 55.00000000000000000 ) ) ;
#31535 = ADVANCED_FACE ( 'NONE', ( #24989 ), #30738, .T. ) ;
#31536 = ORIENTED_EDGE ( 'NONE', *, *, #8305, .T. ) ;
#31537 = AXIS2_PLACEMENT_3D ( 'NONE', #2156, #13130, #26987 ) ;
#31538 = CARTESIAN_POINT ( 'NONE',  ( -36.23083527818512550, -116.0245472910329880, 6.284774454178450043 ) ) ;
#31539 = LINE ( 'NONE', #4358, #20512 ) ;
#31540 = CARTESIAN_POINT ( 'NONE',  ( -35.50000000000000711, -112.0140978167138712, -0.3747823525984256832 ) ) ;
#31541 = ORIENTED_EDGE ( 'NONE', *, *, #28698, .F. ) ;
#31542 = ORIENTED_EDGE ( 'NONE', *, *, #25698, .F. ) ;
#31543 = EDGE_CURVE ( 'NONE', #3309, #7646, #31140, .T. ) ;
#31544 = DIRECTION ( 'NONE',  ( -1.000000000000000000, 0.000000000000000000, 0.000000000000000000 ) ) ;
#31545 = EDGE_CURVE ( 'NONE', #22786, #11158, #661, .T. ) ;
#31546 = CARTESIAN_POINT ( 'NONE',  ( 0.000000000000000000, 0.000000000000000000, 0.000000000000000000 ) ) ;
#31547 = ORIENTED_EDGE ( 'NONE', *, *, #7663, .T. ) ;
#31548 = VERTEX_POINT ( 'NONE', #27864 ) ;
#31549 = CARTESIAN_POINT ( 'NONE',  ( -34.50000000000000000, -115.1446187476384040, -1.616767172155725740 ) ) ;
#31550 = CARTESIAN_POINT ( 'NONE',  ( -35.50000000000000711, -112.8356783780338759, 1.859636627348750348 ) ) ;
#31551 = VECTOR ( 'NONE', #7660, 1000.000000000000000 ) ;
#31552 = ORIENTED_EDGE ( 'NONE', *, *, #8364, .F. ) ;
#31553 = EDGE_LOOP ( 'NONE', ( #4732, #28447, #1032, #6164 ) ) ;
#31554 = DIRECTION ( 'NONE',  ( 0.000000000000000000, 0.000000000000000000, -1.000000000000000000 ) ) ;
#31555 = EDGE_CURVE ( 'NONE', #5428, #21923, #2690, .T. ) ;
#31556 = VECTOR ( 'NONE', #26371, 1000.000000000000000 ) ;
#31557 = CARTESIAN_POINT ( 'NONE',  ( -37.99974912065192001, -113.9929510916434339, 12.63488142334838749 ) ) ;
#31558 = CARTESIAN_POINT ( 'NONE',  ( 0.000000000000000000, 45.78515115856061612, -12.64416602183615623 ) ) ;
#31559 = CARTESIAN_POINT ( 'NONE',  ( -35.50000000000000000, -113.9929510916434339, 11.73841344789270202 ) ) ;
#31560 = CARTESIAN_POINT ( 'NONE',  ( -35.50000102263781798, -115.9929510916434481, 12.62466071271731494 ) ) ;
#31561 = DIRECTION ( 'NONE',  ( -1.000000000000000000, -0.000000000000000000, 0.000000000000000000 ) ) ;
#31562 = LINE ( 'NONE', #14622, #17507 ) ;
#31563 = DIRECTION ( 'NONE',  ( 0.000000000000000000, -0.8660254037844431485, 0.4999999999999922284 ) ) ;
#31564 = CARTESIAN_POINT ( 'NONE',  ( 8.000000000000000000, 16.71027810728552154, 4.579731798933993403 ) ) ;
#31565 = DIRECTION ( 'NONE',  ( 0.000000000000000000, 0.000000000000000000, -1.000000000000000000 ) ) ;
#31566 = ADVANCED_FACE ( 'NONE', ( #3212 ), #25174, .F. ) ;
#31567 = ORIENTED_EDGE ( 'NONE', *, *, #14111, .T. ) ;
#31568 = CARTESIAN_POINT ( 'NONE',  ( -34.49999999999998579, -23.26666049839540307, 81.70096189432331357 ) ) ;
#31569 = EDGE_CURVE ( 'NONE', #8675, #28820, #24264, .T. ) ;
#31570 = CARTESIAN_POINT ( 'NONE',  ( -35.50000000000000711, -112.1859307030124739, 1.448610958621386224 ) ) ;
#31571 = DIRECTION ( 'NONE',  ( 1.000000000000000000, -5.339440136655842133E-16, -1.047965281155519420E-16 ) ) ;
#31572 = CARTESIAN_POINT ( 'NONE',  ( -35.50000000000000711, -114.0882517521923489, 9.510534276948430232 ) ) ;
#31573 = DIRECTION ( 'NONE',  ( 0.000000000000000000, 0.000000000000000000, -1.000000000000000000 ) ) ;
#31574 = VERTEX_POINT ( 'NONE', #19214 ) ;
#31575 = AXIS2_PLACEMENT_3D ( 'NONE', #23256, #34252, #6701 ) ;
#31576 = CARTESIAN_POINT ( 'NONE',  ( 0.000000000000000000, 0.000000000000000000, 50.00000000000000000 ) ) ;
#31577 = CARTESIAN_POINT ( 'NONE',  ( -34.50000000000000000, -112.8832452823708792, -2.621568770093253953 ) ) ;
#31578 = FACE_OUTER_BOUND ( 'NONE', #19205, .T. ) ;
#31579 = ORIENTED_EDGE ( 'NONE', *, *, #31569, .F. ) ;
#31580 = ORIENTED_EDGE ( 'NONE', *, *, #12787, .T. ) ;
#31581 = CARTESIAN_POINT ( 'NONE',  ( -36.64504884055821776, -112.9754527089670688, 8.215225545821551734 ) ) ;
#31582 = VERTEX_POINT ( 'NONE', #30218 ) ;
#31583 = EDGE_LOOP ( 'NONE', ( #25223, #2438, #21210, #32197 ) ) ;
#31584 = VERTEX_POINT ( 'NONE', #1570 ) ;
#31585 = CARTESIAN_POINT ( 'NONE',  ( -35.50000000000000000, -113.1807644833805426, -0.6247823525984269599 ) ) ;
#31586 = CYLINDRICAL_SURFACE ( 'NONE', #6820, 15.49899999999998457 ) ;
#31587 = DIRECTION ( 'NONE',  ( 0.000000000000000000, 0.000000000000000000, -1.000000000000000000 ) ) ;
#31588 = CARTESIAN_POINT ( 'NONE',  ( -35.50000000000000711, -114.9929510916434339, 10.94631322572069365 ) ) ;
#31589 = CARTESIAN_POINT ( 'NONE',  ( 0.000000000000000000, -17.56975900509186062, 9.555290079479195953 ) ) ;
#31590 = CARTESIAN_POINT ( 'NONE',  ( -37.18750000000006395, -114.9929510916434339, 14.11852480586264846 ) ) ;
#31591 = DIRECTION ( 'NONE',  ( -1.000000000000000000, -0.000000000000000000, 0.000000000000000000 ) ) ;
#31592 = AXIS2_PLACEMENT_3D ( 'NONE', #8070, #5038, #24297 ) ;
#31593 = UNCERTAINTY_MEASURE_WITH_UNIT (LENGTH_MEASURE( 1.000000000000000082E-05 ), #27102, 'distance_accuracy_value', 'NONE');
#31594 = CARTESIAN_POINT ( 'NONE',  ( -46.00000000000000000, 0.000000000000000000, 70.00000000000000000 ) ) ;
#31595 = VERTEX_POINT ( 'NONE', #20799 ) ;
#31596 = AXIS2_PLACEMENT_3D ( 'NONE', #7176, #23745, #18339 ) ;
#31597 = CARTESIAN_POINT ( 'NONE',  ( -35.50400759022158326, -115.9929510916434481, 12.68378527132497524 ) ) ;
#31598 = CARTESIAN_POINT ( 'NONE',  ( -35.50000000000000711, -115.1770117227680998, -1.611965039240062181 ) ) ;
#31599 = DIRECTION ( 'NONE',  ( -1.000000000000000000, 0.000000000000000000, 0.000000000000000000 ) ) ;
#31600 = DIRECTION ( 'NONE',  ( -1.734723475976807094E-16, 0.4999999999999989453, 0.8660254037844392627 ) ) ;
#31601 = CARTESIAN_POINT ( 'NONE',  ( -10.00000000000000178, 0.000000000000000000, 0.000000000000000000 ) ) ;
#31602 = DIRECTION ( 'NONE',  ( 1.000000000000000000, -0.000000000000000000, -0.000000000000000000 ) ) ;
#31603 = CARTESIAN_POINT ( 'NONE',  ( 0.000000000000000000, 0.000000000000000000, 0.000000000000000000 ) ) ;
#31604 = EDGE_CURVE ( 'NONE', #23379, #31888, #11600, .T. ) ;
#31605 = CARTESIAN_POINT ( 'NONE',  ( 55.00000000000000711, -26.38406014851796400, 79.52301627764160230 ) ) ;
#31606 = DIRECTION ( 'NONE',  ( 0.000000000000000000, 0.000000000000000000, 1.000000000000000000 ) ) ;
#31607 = VERTEX_POINT ( 'NONE', #4282 ) ;
#31608 = CARTESIAN_POINT ( 'NONE',  ( -37.66520193420439711, -114.7490116281687023, 9.058975545821549957 ) ) ;
#31609 = DIRECTION ( 'NONE',  ( 0.000000000000000000, 0.000000000000000000, -1.000000000000000000 ) ) ;
#31610 = CARTESIAN_POINT ( 'NONE',  ( 0.000000000000000000, 8.053585752061906078, 46.81126742072027014 ) ) ;
#31611 = VERTEX_POINT ( 'NONE', #25887 ) ;
#31612 = ORIENTED_EDGE ( 'NONE', *, *, #25743, .T. ) ;
#31613 = DIRECTION ( 'NONE',  ( -1.000000000000000000, -1.836970198721029934E-16, -0.000000000000000000 ) ) ;
#31614 = DIRECTION ( 'NONE',  ( -1.000000000000000000, 1.502314598737164455E-16, -8.673617379883947958E-17 ) ) ;
#31615 = ORIENTED_EDGE ( 'NONE', *, *, #8238, .T. ) ;
#31616 = CARTESIAN_POINT ( 'NONE',  ( -37.05926240293131713, -111.0000000000000284, 9.621475545821549957 ) ) ;
#31617 = VERTEX_POINT ( 'NONE', #11821 ) ;
#31618 = AXIS2_PLACEMENT_3D ( 'NONE', #2883, #19578, #27362 ) ;
#31619 = CARTESIAN_POINT ( 'NONE',  ( 7.999999999999992895, -24.72041153920761758, 40.55929306992680949 ) ) ;
#31620 = DIRECTION ( 'NONE',  ( -1.000000000000000000, -0.000000000000000000, -0.000000000000000000 ) ) ;
#31621 = VECTOR ( 'NONE', #9288, 1000.000000000000000 ) ;
#31622 = CARTESIAN_POINT ( 'NONE',  ( 50.00000000000000000, 9.797174393178845379E-16, 78.00000000000001421 ) ) ;
#31623 = VECTOR ( 'NONE', #14179, 1000.000000000000000 ) ;
#31624 = DIRECTION ( 'NONE',  ( 0.000000000000000000, 0.3681245526846786964, -0.9297764858882511252 ) ) ;
#31625 = ORIENTED_EDGE ( 'NONE', *, *, #26243, .T. ) ;
#31626 = VERTEX_POINT ( 'NONE', #15220 ) ;
#31627 = CARTESIAN_POINT ( 'NONE',  ( 70.00001200000001234, -29.98076211353320986, 84.47640122440162713 ) ) ;
#31628 = LINE ( 'NONE', #4113, #27553 ) ;
#31629 = VERTEX_POINT ( 'NONE', #33985 ) ;
#31630 = LINE ( 'NONE', #4288, #33195 ) ;
#31631 = CARTESIAN_POINT ( 'NONE',  ( 0.000000000000000000, -16.59870953437682672, 3.253005020243791456 ) ) ;
#31632 = CARTESIAN_POINT ( 'NONE',  ( -2.000000000000001776, 0.000000000000000000, 0.000000000000000000 ) ) ;
#31633 = CARTESIAN_POINT ( 'NONE',  ( -34.50481333282507279, -115.9929510916434481, 12.74107470552716315 ) ) ;
#31634 = DIRECTION ( 'NONE',  ( 0.000000000000000000, -0.2486898871648622611, 0.9685831611286292997 ) ) ;
#31635 = CARTESIAN_POINT ( 'NONE',  ( -38.99999999999999289, -113.9407375970686900, 2.253524454178449155 ) ) ;
#31636 = CARTESIAN_POINT ( 'NONE',  ( -34.50000000000000000, -115.9929510916434481, 11.38636890470581164 ) ) ;
#31637 = LINE ( 'NONE', #15237, #23971 ) ;
#31638 = DIRECTION ( 'NONE',  ( -1.000000000000000000, 0.000000000000000000, 0.000000000000000000 ) ) ;
#31639 = CIRCLE ( 'NONE', #17264, 22.00000000000000000 ) ;
#31640 = FACE_OUTER_BOUND ( 'NONE', #15553, .T. ) ;
#31641 = DIRECTION ( 'NONE',  ( -1.000000000000000000, -1.836970198721029934E-16, -0.000000000000000000 ) ) ;
#31642 = EDGE_CURVE ( 'NONE', #35403, #2939, #9875, .T. ) ;
#31643 = EDGE_CURVE ( 'NONE', #18917, #11237, #30021, .T. ) ;
#31644 = FACE_OUTER_BOUND ( 'NONE', #27742, .T. ) ;
#31645 = DIRECTION ( 'NONE',  ( 1.000000000000000000, -0.000000000000000000, -0.000000000000000000 ) ) ;
#31646 = ORIENTED_EDGE ( 'NONE', *, *, #27301, .F. ) ;
#31647 = AXIS2_PLACEMENT_3D ( 'NONE', #34095, #3681, #22921 ) ;
#31648 = CARTESIAN_POINT ( 'NONE',  ( -34.83677480945821259, -116.0794154965774965, 2.683975545821551734 ) ) ;
#31649 = VECTOR ( 'NONE', #25436, 1000.000000000000000 ) ;
#31650 = DIRECTION ( 'NONE',  ( -1.000000000000000000, 0.000000000000000000, -0.000000000000000000 ) ) ;
#31651 = CARTESIAN_POINT ( 'NONE',  ( -35.50000000000000711, -116.0140978167138712, 0.6252176474015648244 ) ) ;
#31652 = VERTEX_POINT ( 'NONE', #9481 ) ;
#31653 = ORIENTED_EDGE ( 'NONE', *, *, #34331, .F. ) ;
#31654 = PRODUCT ( 'handle', 'handle', '', ( #9308 ) ) ;
#31655 = DIRECTION ( 'NONE',  ( -1.000000000000000000, 0.000000000000000000, 0.000000000000000000 ) ) ;
#31656 = EDGE_LOOP ( 'NONE', ( #35100, #663, #10318, #7543 ) ) ;
#31657 = ADVANCED_FACE ( 'NONE', ( #22801 ), #33802, .T. ) ;
#31658 = ORIENTED_EDGE ( 'NONE', *, *, #16337, .F. ) ;
#31659 = VERTEX_POINT ( 'NONE', #14876 ) ;
#31660 = DIRECTION ( 'NONE',  ( -1.000000000000000000, 0.000000000000000000, 0.000000000000000000 ) ) ;
#31661 = CARTESIAN_POINT ( 'NONE',  ( -35.00000000000000000, -113.9407375970686900, 5.496475545821551734 ) ) ;
#31662 = AXIS2_PLACEMENT_3D ( 'NONE', #16870, #12203, #28589 ) ;
#31663 = CARTESIAN_POINT ( 'NONE',  ( 0.000000000000000000, 0.000000000000000000, 45.00000000000000711 ) ) ;
#31664 = ORIENTED_EDGE ( 'NONE', *, *, #9301, .F. ) ;
#31665 = ORIENTED_EDGE ( 'NONE', *, *, #282, .T. ) ;
#31666 = CARTESIAN_POINT ( 'NONE',  ( -35.50000000000000000, -111.1162063037085801, -1.269118781493287607 ) ) ;
#31667 = DIRECTION ( 'NONE',  ( 1.000000000000000000, -0.000000000000000000, -0.000000000000000000 ) ) ;
#31668 = CARTESIAN_POINT ( 'NONE',  ( -42.49999999999999289, -34.23950567274729195, 73.69543654875863581 ) ) ;
#31669 = COLOUR_RGB ( '', 0.09019608, 0.27058824, 0.51372549) ;
#31670 = ORIENTED_EDGE ( 'NONE', *, *, #9948, .T. ) ;
#31671 = VECTOR ( 'NONE', #34243, 1000.000000000000000 ) ;
#31672 = CARTESIAN_POINT ( 'NONE',  ( -38.00000000000000711, -114.9929510916434339, 12.60752341388803721 ) ) ;
#31673 = EDGE_CURVE ( 'NONE', #21688, #20267, #13345, .T. ) ;
#31674 = AXIS2_PLACEMENT_3D ( 'NONE', #5028, #20837, #15617 ) ;
#31675 = CARTESIAN_POINT ( 'NONE',  ( -34.50000000000000000, -114.9929510916434339, 12.59652202191340642 ) ) ;
#31676 = FACE_OUTER_BOUND ( 'NONE', #15937, .T. ) ;
#31677 = CARTESIAN_POINT ( 'NONE',  ( -37.53269373325071712, -114.9929510916434339, 13.11752178341324360 ) ) ;
#31678 = LINE ( 'NONE', #23220, #9955 ) ;
#31679 = CARTESIAN_POINT ( 'NONE',  ( -35.87745010033553683, -113.9929510916434339, 14.11371147303761475 ) ) ;
#31680 = CARTESIAN_POINT ( 'NONE',  ( 0.000000000000000000, 20.99948489194422763, 42.60488980472790388 ) ) ;
#31681 = CARTESIAN_POINT ( 'NONE',  ( -37.50818044754229419, -114.9929510916434339, 13.11847460610629668 ) ) ;
#31682 = CARTESIAN_POINT ( 'NONE',  ( -34.49999999999998579, -34.23950567274729195, 73.69543654875863581 ) ) ;
#31683 = ORIENTED_EDGE ( 'NONE', *, *, #11069, .T. ) ;
#31684 = FACE_OUTER_BOUND ( 'NONE', #15227, .T. ) ;
#31685 = CARTESIAN_POINT ( 'NONE',  ( 55.00000000000000711, -28.31857036507964764, 80.03062855292515110 ) ) ;
#31686 = EDGE_CURVE ( 'NONE', #4628, #3462, #17392, .T. ) ;
#31687 = VERTEX_POINT ( 'NONE', #26230 ) ;
#31688 = EDGE_CURVE ( 'NONE', #17618, #26843, #670, .T. ) ;
#31689 = CARTESIAN_POINT ( 'NONE',  ( -35.50000000000000711, -114.9929510916434339, 10.53376102667243508 ) ) ;
#31690 = ORIENTED_EDGE ( 'NONE', *, *, #9939, .F. ) ;
#31691 = EDGE_CURVE ( 'NONE', #22225, #11561, #14467, .T. ) ;
#31692 = DIRECTION ( 'NONE',  ( 1.000000000000000000, -0.000000000000000000, -0.000000000000000000 ) ) ;
#31693 = VERTEX_POINT ( 'NONE', #3736 ) ;
#31694 = DIRECTION ( 'NONE',  ( -1.000000000000000000, 0.000000000000000000, 0.000000000000000000 ) ) ;
#31695 = ORIENTED_EDGE ( 'NONE', *, *, #19460, .F. ) ;
#31696 = CARTESIAN_POINT ( 'NONE',  ( -34.50000000000000000, -113.0140978167136581, 0.8752176474015604946 ) ) ;
#31697 = CYLINDRICAL_SURFACE ( 'NONE', #15008, 9.499000000000000554 ) ;
#31698 = CARTESIAN_POINT ( 'NONE',  ( -37.88768952767750164, -115.9754527089670262, 7.972274454178450043 ) ) ;
#31699 = ADVANCED_FACE ( 'NONE', ( #31455 ), #6594, .F. ) ;
#31700 = AXIS2_PLACEMENT_3D ( 'NONE', #30812, #17292, #11552 ) ;
#31701 = PRESENTATION_LAYER_ASSIGNMENT (  '', '', ( #11578 ) ) ;
#31702 = EDGE_LOOP ( 'NONE', ( #27026, #30072, #30701, #15427 ) ) ;
#31703 = AXIS2_PLACEMENT_3D ( 'NONE', #7368, #15980, #29339 ) ;
#31704 = CARTESIAN_POINT ( 'NONE',  ( -36.11231047232249125, -112.0245472910329880, 5.722274454178448266 ) ) ;
#31705 = EDGE_CURVE ( 'NONE', #10010, #33387, #4144, .T. ) ;
#31706 = CARTESIAN_POINT ( 'NONE',  ( -55.00000000000000000, 19.99999999999998934, 120.0000000000000000 ) ) ;
#31707 = CARTESIAN_POINT ( 'NONE',  ( -35.50000000000000711, -112.0140978167138712, -0.4685323525984295134 ) ) ;
#31708 = VERTEX_POINT ( 'NONE', #25523 ) ;
#31709 = VERTEX_POINT ( 'NONE', #23523 ) ;
#31710 = CARTESIAN_POINT ( 'NONE',  ( 8.000000000000000000, -5.482169781018935595, 16.00140663693123599 ) ) ;
#31711 = DIRECTION ( 'NONE',  ( 0.000000000000000000, 0.8443279255020124108, 0.5358267949790006535 ) ) ;
#31712 = EDGE_LOOP ( 'NONE', ( #20232, #27812 ) ) ;
#31713 = VERTEX_POINT ( 'NONE', #838 ) ;
#31714 = CARTESIAN_POINT ( 'NONE',  ( -34.50000000000000000, -116.0140978167138712, 0.3752176474015736507 ) ) ;
#31715 = CARTESIAN_POINT ( 'NONE',  ( -35.50000000000000711, -112.0140978167138712, 0.7189676474015718188 ) ) ;
#31716 = DIRECTION ( 'NONE',  ( 1.000000000000000000, -5.339440136655842133E-16, -1.047965281155519420E-16 ) ) ;
#31717 = VERTEX_POINT ( 'NONE', #23166 ) ;
#31718 = ORIENTED_EDGE ( 'NONE', *, *, #32711, .F. ) ;
#31719 = DIRECTION ( 'NONE',  ( 0.000000000000000000, 1.000000000000000000, 0.000000000000000000 ) ) ;
#31720 = EDGE_CURVE ( 'NONE', #15703, #17480, #19079, .T. ) ;
#31721 = CARTESIAN_POINT ( 'NONE',  ( -34.50000000000000000, -113.9929510916434339, 10.52826033068511435 ) ) ;
#31722 = DIRECTION ( 'NONE',  ( 0.000000000000000000, -0.9848077530122096857, 0.1736481776669208388 ) ) ;
#31724 = EDGE_CURVE ( 'NONE', #35356, #12864, #23082, .T. ) ;
#31723 = CIRCLE ( 'NONE', #32889, 52.00000000000000711 ) ;
#31725 =( GEOMETRIC_REPRESENTATION_CONTEXT ( 3 ) GLOBAL_UNCERTAINTY_ASSIGNED_CONTEXT ( ( #6065 ) ) GLOBAL_UNIT_ASSIGNED_CONTEXT ( ( #29911, #10296, #34781 ) ) REPRESENTATION_CONTEXT ( 'NONE', 'WORKASPACE' ) );
#31726 = CIRCLE ( 'NONE', #8130, 4.725000000000016520 ) ;
#31727 = CARTESIAN_POINT ( 'NONE',  ( -37.24999999999992184, -113.9929510916434339, 13.11852480586264846 ) ) ;
#31728 = CARTESIAN_POINT ( 'NONE',  ( -35.50000000000000000, -115.9929510916434481, 12.50851088611648265 ) ) ;
#31729 = DIRECTION ( 'NONE',  ( 0.000000000000000000, 0.000000000000000000, -1.000000000000000000 ) ) ;
#31730 = DIRECTION ( 'NONE',  ( -1.000000000000000000, 0.000000000000000000, 0.000000000000000000 ) ) ;
#31731 = EDGE_CURVE ( 'NONE', #2578, #31595, #17754, .T. ) ;
#31732 = VERTEX_POINT ( 'NONE', #34339 ) ;
#31733 = EDGE_CURVE ( 'NONE', #19728, #966, #26557, .T. ) ;
#31734 = FACE_OUTER_BOUND ( 'NONE', #31843, .T. ) ;
#31735 = CYLINDRICAL_SURFACE ( 'NONE', #7621, 52.00000000000000711 ) ;
#31736 = LINE ( 'NONE', #9951, #3646 ) ;
#31737 = EDGE_LOOP ( 'NONE', ( #30761, #12815, #17790, #27994 ) ) ;
#31738 = VECTOR ( 'NONE', #33581, 1000.000000000000000 ) ;
#31739 = DIRECTION ( 'NONE',  ( 0.000000000000000000, 0.000000000000000000, -1.000000000000000000 ) ) ;
#31740 = CARTESIAN_POINT ( 'NONE',  ( -35.50000000000000711, -112.0140978167138712, 0.5627176474015717078 ) ) ;
#31741 = DIRECTION ( 'NONE',  ( 0.000000000000000000, 0.000000000000000000, -1.000000000000000000 ) ) ;
#31742 = CONTEXT_DEPENDENT_SHAPE_REPRESENTATION ( #6917, #19610 ) ;
#31743 = CARTESIAN_POINT ( 'NONE',  ( -35.50000000000000711, -114.0000000000003411, 9.500000000000035527 ) ) ;
#31744 = CYLINDRICAL_SURFACE ( 'NONE', #11327, 4.000000000000000000 ) ;
#31745 = EDGE_CURVE ( 'NONE', #1101, #3615, #6959, .T. ) ;
#31746 = VERTEX_POINT ( 'NONE', #7137 ) ;
#31747 = DIRECTION ( 'NONE',  ( 0.000000000000000000, 0.000000000000000000, 1.000000000000000000 ) ) ;
#31748 = CARTESIAN_POINT ( 'NONE',  ( -35.50000000000000000, -113.8814751941374652, 2.992951091643117678 ) ) ;
#31749 = CARTESIAN_POINT ( 'NONE',  ( 3.239593890920905217, -13.56862304811760822, -1.200000000000006617 ) ) ;
#31750 = ORIENTED_EDGE ( 'NONE', *, *, #4723, .T. ) ;
#31751 = EDGE_LOOP ( 'NONE', ( #18372, #2537 ) ) ;
#31752 = CARTESIAN_POINT ( 'NONE',  ( -35.99999999999999289, -114.0592624029313242, 4.503524454178447378 ) ) ;
#31753 = CIRCLE ( 'NONE', #22540, 7.199999999999994849 ) ;
#31754 =( LENGTH_UNIT ( ) NAMED_UNIT ( * ) SI_UNIT ( .MILLI., .METRE. ) );
#31755 = ORIENTED_EDGE ( 'NONE', *, *, #13888, .T. ) ;
#31756 = ORIENTED_EDGE ( 'NONE', *, *, #22875, .T. ) ;
#31757 = CARTESIAN_POINT ( 'NONE',  ( -35.50000000000000000, -115.0140978167138712, -0.5622823525984408377 ) ) ;
#31758 = CARTESIAN_POINT ( 'NONE',  ( -42.49999999999999289, -25.98076211353322051, 84.99999999999992895 ) ) ;
#31759 = EDGE_CURVE ( 'NONE', #5115, #29876, #22514, .T. ) ;
#31760 = DIRECTION ( 'NONE',  ( 0.000000000000000000, 0.000000000000000000, 1.000000000000000000 ) ) ;
#31761 = AXIS2_PLACEMENT_3D ( 'NONE', #17323, #33546, #19664 ) ;
#31762 = EDGE_CURVE ( 'NONE', #27203, #29543, #23690, .T. ) ;
#31763 = CARTESIAN_POINT ( 'NONE',  ( -36.31249999999995026, -114.9929510916434339, 13.11852480586264669 ) ) ;
#31764 = EDGE_CURVE ( 'NONE', #19248, #5065, #31726, .T. ) ;
#31765 = CYLINDRICAL_SURFACE ( 'NONE', #18403, 4.000000000000000000 ) ;
#31766 = CARTESIAN_POINT ( 'NONE',  ( -34.50000000000000000, -114.9929510916434339, 12.53051367006571581 ) ) ;
#31767 = CARTESIAN_POINT ( 'NONE',  ( 8.000000000000000000, 15.17386234660384581, 15.92965478239621824 ) ) ;
#31768 = VECTOR ( 'NONE', #16970, 1000.000000000000000 ) ;
#31769 = ADVANCED_FACE ( 'NONE', ( #23705 ), #23891, .T. ) ;
#31770 = LINE ( 'NONE', #24214, #21478 ) ;
#31771 = VERTEX_POINT ( 'NONE', #31802 ) ;
#31772 = CARTESIAN_POINT ( 'NONE',  ( -35.50000000000000000, -115.9929510916434481, 12.50851088611648265 ) ) ;
#31774 = CARTESIAN_POINT ( 'NONE',  ( -35.50000000000000711, -115.6286452741999113, -1.424448457485488095 ) ) ;
#31773 = VECTOR ( 'NONE', #30316, 1000.000000000000000 ) ;
#31775 = EDGE_CURVE ( 'NONE', #33633, #14563, #12171, .T. ) ;
#31776 = DIRECTION ( 'NONE',  ( -1.000000000000000000, -0.000000000000000000, 0.000000000000000000 ) ) ;
#31777 = DIRECTION ( 'NONE',  ( 0.000000000000000000, -1.000000000000000000, 0.000000000000000000 ) ) ;
#31778 = ORIENTED_EDGE ( 'NONE', *, *, #7460, .F. ) ;
#31779 = FACE_OUTER_BOUND ( 'NONE', #23919, .T. ) ;
#31780 = DIRECTION ( 'NONE',  ( 0.000000000000000000, 0.000000000000000000, -1.000000000000000000 ) ) ;
#31781 = CARTESIAN_POINT ( 'NONE',  ( 0.000000000000000000, 0.000000000000000000, 0.000000000000000000 ) ) ;
#31782 = CARTESIAN_POINT ( 'NONE',  ( 8.000000000000000000, -16.71027810728550733, -2.620268201066114688 ) ) ;
#31783 = ORIENTED_EDGE ( 'NONE', *, *, #8625, .T. ) ;
#31784 = CARTESIAN_POINT ( 'NONE',  ( -37.47347596530441649, -114.9754527089670262, 6.472274454178449155 ) ) ;
#31785 = FACE_OUTER_BOUND ( 'NONE', #15134, .T. ) ;
#31786 = CARTESIAN_POINT ( 'NONE',  ( 2.000000000000001776, 0.000000000000000000, 0.000000000000000000 ) ) ;
#31787 = ORIENTED_EDGE ( 'NONE', *, *, #4028, .F. ) ;
#31788 = CIRCLE ( 'NONE', #28347, 5.000000000000004441 ) ;
#31789 = ORIENTED_EDGE ( 'NONE', *, *, #27121, .T. ) ;
#31790 = VECTOR ( 'NONE', #15185, 1000.000000000000000 ) ;
#31791 = AXIS2_PLACEMENT_3D ( 'NONE', #29899, #15825, #34959 ) ;
#31792 = FACE_OUTER_BOUND ( 'NONE', #29688, .T. ) ;
#31793 = ORIENTED_EDGE ( 'NONE', *, *, #31691, .F. ) ;
#31794 = CARTESIAN_POINT ( 'NONE',  ( -34.83677480945821259, -116.0794154965774965, 7.183975545821551734 ) ) ;
#31795 = ORIENTED_EDGE ( 'NONE', *, *, #13536, .F. ) ;
#31796 = CARTESIAN_POINT ( 'NONE',  ( 0.000000000000000000, 17.50309955389674954, -43.60271849949345579 ) ) ;
#31797 = VERTEX_POINT ( 'NONE', #7665 ) ;
#31798 = CARTESIAN_POINT ( 'NONE',  ( 0.000000000000000000, -2.710505431213761085E-17, 54.99999999999999289 ) ) ;
#31799 = AXIS2_PLACEMENT_3D ( 'NONE', #27103, #10359, #16627 ) ;
#31800 = CIRCLE ( 'NONE', #28333, 17.49900000000001654 ) ;
#31801 = DIRECTION ( 'NONE',  ( -1.000000000000000000, -0.000000000000000000, 0.000000000000000000 ) ) ;
#31802 = CARTESIAN_POINT ( 'NONE',  ( 0.000000000000000000, -14.87816164169118416, 4.342730381189816136 ) ) ;
#31803 = VERTEX_POINT ( 'NONE', #32165 ) ;
#31804 = VERTEX_POINT ( 'NONE', #12907 ) ;
#31805 = EDGE_CURVE ( 'NONE', #21774, #18596, #32298, .T. ) ;
#31806 = DIRECTION ( 'NONE',  ( -1.226634733346697831E-16, -0.9659258262890698665, 0.2588190451025151884 ) ) ;
#31807 = DIRECTION ( 'NONE',  ( 0.000000000000000000, -0.9510565162951565288, 0.3090169943749384029 ) ) ;
#31808 = ORIENTED_EDGE ( 'NONE', *, *, #31533, .T. ) ;
#31809 = DIRECTION ( 'NONE',  ( -1.000000000000000000, -0.000000000000000000, -0.000000000000000000 ) ) ;
#31810 = CIRCLE ( 'NONE', #17431, 19.99999999999998579 ) ;
#31811 = DIRECTION ( 'NONE',  ( 0.000000000000000000, 0.000000000000000000, -1.000000000000000000 ) ) ;
#31812 = DIRECTION ( 'NONE',  ( -0.000000000000000000, 0.000000000000000000, -1.000000000000000000 ) ) ;
#31813 = CARTESIAN_POINT ( 'NONE',  ( -34.50000000000000000, -115.9929510916434481, 11.91443571948720148 ) ) ;
#31814 = CARTESIAN_POINT ( 'NONE',  ( 4.000000000000000000, 17.06000345190455647, -10.43821259704003523 ) ) ;
#31815 = CARTESIAN_POINT ( 'NONE',  ( -38.99999999999999289, -113.9407375970686900, 3.753524454178449155 ) ) ;
#31816 = CARTESIAN_POINT ( 'NONE',  ( -34.50000000000000000, -115.9929510916434481, 10.51725893871049067 ) ) ;
#31817 = CARTESIAN_POINT ( 'NONE',  ( 0.000000000000000000, 0.000000000000000000, 60.00000000000000000 ) ) ;
#31818 = CARTESIAN_POINT ( 'NONE',  ( -5.639656061357301020, -10.48075544252181857, -1.200000000000006617 ) ) ;
#31819 = DIRECTION ( 'NONE',  ( 0.000000000000000000, 0.000000000000000000, 1.000000000000000000 ) ) ;
#31820 = LINE ( 'NONE', #9506, #842 ) ;
#31821 = AXIS2_PLACEMENT_3D ( 'NONE', #27766, #3106, #14410 ) ;
#31822 = CIRCLE ( 'NONE', #14559, 5.000000000000004441 ) ;
#31823 = CARTESIAN_POINT ( 'NONE',  ( 8.000000000000000000, -16.94522934049218676, 8.128228055638807348 ) ) ;
#31824 = FILL_AREA_STYLE_COLOUR ( '', #28140 ) ;
#31825 = ORIENTED_EDGE ( 'NONE', *, *, #20955, .F. ) ;
#31826 = CARTESIAN_POINT ( 'NONE',  ( -38.30190309005061522, -111.0245472910330022, 5.027725545821551734 ) ) ;
#31827 = DIRECTION ( 'NONE',  ( 0.000000000000000000, 0.8090169943749448977, 0.5877852522924766898 ) ) ;
#31828 = CARTESIAN_POINT ( 'NONE',  ( -35.50000000000000000, -113.0140978167142833, 0.8752176474019800478 ) ) ;
#31829 = ORIENTED_EDGE ( 'NONE', *, *, #17629, .F. ) ;
#31830 = ORIENTED_EDGE ( 'NONE', *, *, #6419, .F. ) ;
#31831 = CIRCLE ( 'NONE', #18619, 7.200000000000000178 ) ;
#31832 = DIRECTION ( 'NONE',  ( 0.000000000000000000, 0.3090169943749477288, -0.9510565162951535312 ) ) ;
#31833 = CARTESIAN_POINT ( 'NONE',  ( 0.000000000000000000, 0.000000000000000000, 0.000000000000000000 ) ) ;
#31834 = VERTEX_POINT ( 'NONE', #4986 ) ;
#31835 = VERTEX_POINT ( 'NONE', #26413 ) ;
#31836 = ORIENTED_EDGE ( 'NONE', *, *, #26638, .T. ) ;
#31837 = VECTOR ( 'NONE', #596, 1000.000000000000000 ) ;
#31838 = AXIS2_PLACEMENT_3D ( 'NONE', #13577, #7629, #27454 ) ;
#31839 = CARTESIAN_POINT ( 'NONE',  ( 8.000000000000007105, -3.268936481846063113, -13.61301047812921183 ) ) ;
#31840 = CARTESIAN_POINT ( 'NONE',  ( -6.938893903907228378E-15, 0.7408941433508786645, -1.200000000000006617 ) ) ;
#31841 = DIRECTION ( 'NONE',  ( 0.000000000000000000, 0.000000000000000000, -1.000000000000000000 ) ) ;
#31842 = CARTESIAN_POINT ( 'NONE',  ( -34.49999999999998579, -13.17619866229195047, 79.33933265213923391 ) ) ;
#31843 = EDGE_LOOP ( 'NONE', ( #33504, #19563, #11778, #14549 ) ) ;
#31844 = EDGE_LOOP ( 'NONE', ( #19911, #2463 ) ) ;
#31845 = CARTESIAN_POINT ( 'NONE',  ( -35.50000000000000000, -115.6584342456100671, -2.522673865603758614 ) ) ;
#31846 = CIRCLE ( 'NONE', #7124, 7.199999999999994849 ) ;
#31847 = ADVANCED_FACE ( 'NONE', ( #2121 ), #1748, .T. ) ;
#31848 = CIRCLE ( 'NONE', #15152, 8.000000000000008882 ) ;
#31849 = CARTESIAN_POINT ( 'NONE',  ( -39.49999999999999289, -14.17619866229204106, 94.12476896299857287 ) ) ;
#31850 = CARTESIAN_POINT ( 'NONE',  ( 0.000000000000000000, -22.43957647427188817, 41.27978878573619426 ) ) ;
#31851 = ORIENTED_EDGE ( 'NONE', *, *, #1316, .T. ) ;
#31852 = DIRECTION ( 'NONE',  ( 0.000000000000000000, 0.000000000000000000, 1.000000000000000000 ) ) ;
#31853 = CARTESIAN_POINT ( 'NONE',  ( -34.50000000000000000, -112.7472371723319355, 1.839427296857320648 ) ) ;
#31854 = CARTESIAN_POINT ( 'NONE',  ( -34.51202277066418844, -114.9929510916434339, 12.81430620224972294 ) ) ;
#31855 = CARTESIAN_POINT ( 'NONE',  ( 8.000000000000000000, 0.000000000000000000, 0.000000000000000000 ) ) ;
#31856 = CARTESIAN_POINT ( 'NONE',  ( -35.99181955245763476, -114.9929510916434339, 13.11847460610632687 ) ) ;
#31857 = CARTESIAN_POINT ( 'NONE',  ( 8.000000000000000000, 0.000000000000000000, 0.000000000000000000 ) ) ;
#31858 = ADVANCED_FACE ( 'NONE', ( #4644 ), #21345, .T. ) ;
#31859 = CARTESIAN_POINT ( 'NONE',  ( -34.50000000000000000, -114.9912366357066986, 10.44580456020104720 ) ) ;
#31860 = FACE_OUTER_BOUND ( 'NONE', #1560, .T. ) ;
#31861 = CARTESIAN_POINT ( 'NONE',  ( -37.98402046630260287, -114.9929510916434339, 12.74811950270164118 ) ) ;
#31862 = CARTESIAN_POINT ( 'NONE',  ( 7.999999999999992895, -34.03046037009232094, -33.13733193845841640 ) ) ;
#31863 = ORIENTED_EDGE ( 'NONE', *, *, #22056, .F. ) ;
#31864 = DIRECTION ( 'NONE',  ( -1.000000000000000000, 0.000000000000000000, 0.000000000000000000 ) ) ;
#31865 = DIRECTION ( 'NONE',  ( 1.000000000000000000, -0.000000000000000000, -0.000000000000000000 ) ) ;
#31866 = ORIENTED_EDGE ( 'NONE', *, *, #33847, .T. ) ;
#31867 = CARTESIAN_POINT ( 'NONE',  ( -35.50000000000000711, -114.9929501463477663, 10.50247632894551231 ) ) ;
#31868 = EDGE_LOOP ( 'NONE', ( #4808, #35589 ) ) ;
#31869 = CARTESIAN_POINT ( 'NONE',  ( -35.02454729103298803, -114.8876895276775087, 1.597274454178448710 ) ) ;
#31870 = CARTESIAN_POINT ( 'NONE',  ( 50.00000000000000711, -25.98076211353320275, 90.99999999999994316 ) ) ;
#31871 = EDGE_LOOP ( 'NONE', ( #28143, #3786, #30870, #12974 ) ) ;
#31872 = DIRECTION ( 'NONE',  ( 0.000000000000000000, 0.000000000000000000, 1.000000000000000000 ) ) ;
#31873 = VERTEX_POINT ( 'NONE', #27133 ) ;
#31874 = CIRCLE ( 'NONE', #28407, 4.980000000000017302 ) ;
#31875 = AXIS2_PLACEMENT_3D ( 'NONE', #30065, #5406, #4875 ) ;
#31876 = CARTESIAN_POINT ( 'NONE',  ( -34.50000000000000000, -113.0140978167138712, -0.6247823525979733228 ) ) ;
#31877 = CARTESIAN_POINT ( 'NONE',  ( 0.000000000000000000, -24.72041153920761758, 40.55929306992680949 ) ) ;
#31878 = CARTESIAN_POINT ( 'NONE',  ( -37.76916472181487450, -111.9754527089670404, 8.534774454178448266 ) ) ;
#31879 = ORIENTED_EDGE ( 'NONE', *, *, #24914, .T. ) ;
#31880 = CARTESIAN_POINT ( 'NONE',  ( -39.16322519054179452, -116.0794154965774823, 5.066024454178449155 ) ) ;
#31881 = DIRECTION ( 'NONE',  ( 0.000000000000000000, 0.000000000000000000, -1.000000000000000000 ) ) ;
#31882 = CARTESIAN_POINT ( 'NONE',  ( -35.50000000000000711, -112.0140978167138712, -0.5622823525984296245 ) ) ;
#31883 = ORIENTED_EDGE ( 'NONE', *, *, #19209, .T. ) ;
#31884 = ORIENTED_EDGE ( 'NONE', *, *, #24604, .T. ) ;
#31885 = DIRECTION ( 'NONE',  ( -1.000000000000000000, -0.000000000000000000, -0.000000000000000000 ) ) ;
#31886 =( NAMED_UNIT ( * ) SI_UNIT ( $, .STERADIAN. ) SOLID_ANGLE_UNIT ( ) );
#31887 = CARTESIAN_POINT ( 'NONE',  ( 0.000000000000000000, 0.000000000000000000, -49.10000000000000142 ) ) ;
#31888 = VERTEX_POINT ( 'NONE', #24249 ) ;
#31889 = VERTEX_POINT ( 'NONE', #21175 ) ;
#31890 = CARTESIAN_POINT ( 'NONE',  ( -34.50000000000000000, -114.9724313160460696, -1.624792769101446765 ) ) ;
#31891 = EDGE_CURVE ( 'NONE', #9483, #7515, #9316, .T. ) ;
#31892 = EDGE_CURVE ( 'NONE', #12629, #29368, #15055, .T. ) ;
#31893 = DIRECTION ( 'NONE',  ( -1.000000000000000000, -0.000000000000000000, -0.000000000000000000 ) ) ;
#31894 = ORIENTED_EDGE ( 'NONE', *, *, #35235, .F. ) ;
#31895 = EDGE_LOOP ( 'NONE', ( #13344, #1163, #4939, #9218 ) ) ;
#31896 = DIRECTION ( 'NONE',  ( 0.000000000000000000, 0.000000000000000000, -1.000000000000000000 ) ) ;
#31897 = VECTOR ( 'NONE', #11811, 1000.000000000000000 ) ;
#31898 = CARTESIAN_POINT ( 'NONE',  ( -34.50000000000000000, -113.9929510916435618, 10.50625754673588474 ) ) ;
#31899 = DIRECTION ( 'NONE',  ( -1.000000000000000000, -0.000000000000000000, -0.000000000000000000 ) ) ;
#31900 = EDGE_CURVE ( 'NONE', #5418, #34867, #15576, .T. ) ;
#31901 = CARTESIAN_POINT ( 'NONE',  ( -38.00000000000000711, -113.9929510916434339, 12.39849696637031151 ) ) ;
#31902 = ADVANCED_FACE ( 'NONE', ( #2303 ), #31986, .F. ) ;
#31903 = AXIS2_PLACEMENT_3D ( 'NONE', #11850, #3958, #22832 ) ;
#31904 = CARTESIAN_POINT ( 'NONE',  ( -38.00000000000000711, -115.9929510916434481, 12.50851088611646311 ) ) ;
#31905 = CARTESIAN_POINT ( 'NONE',  ( 65.00000000000001421, -25.98076211353320986, 91.99999999999994316 ) ) ;
#31906 = LINE ( 'NONE', #20906, #32475 ) ;
#31907 = EDGE_LOOP ( 'NONE', ( #28466, #32512, #10498, #29190 ) ) ;
#31908 = DIRECTION ( 'NONE',  ( 0.000000000000000000, 0.000000000000000000, -1.000000000000000000 ) ) ;
#31909 = PLANE ( 'NONE',  #13956 ) ;
#31910 = DIRECTION ( 'NONE',  ( 0.000000000000000000, 0.000000000000000000, 1.000000000000000000 ) ) ;
#31911 = CIRCLE ( 'NONE', #15215, 14.00000000000000000 ) ;
#31912 = VERTEX_POINT ( 'NONE', #1933 ) ;
#31913 = CARTESIAN_POINT ( 'NONE',  ( 4.000000000000000000, 4.627536653468036720E-16, 54.99999999999999289 ) ) ;
#31914 = CARTESIAN_POINT ( 'NONE',  ( -35.50000000000000711, -112.8511839106603247, -1.611965039240275122 ) ) ;
#31915 = DIRECTION ( 'NONE',  ( 0.000000000000000000, 0.4817536741017164337, -0.8763066800438629178 ) ) ;
#31916 = DIRECTION ( 'NONE',  ( 0.000000000000000000, 1.000000000000000000, 0.000000000000000000 ) ) ;
#31917 = CARTESIAN_POINT ( 'NONE',  ( -35.50000000000000711, -114.0185793162512908, 9.502217742515812304 ) ) ;
#31918 = CARTESIAN_POINT ( 'NONE',  ( 0.000000000000000000, 0.9861715913090087771, -17.47118961583601049 ) ) ;
#31919 = EDGE_CURVE ( 'NONE', #4062, #10084, #21385, .T. ) ;
#31920 = ORIENTED_EDGE ( 'NONE', *, *, #16562, .F. ) ;
#31921 = CYLINDRICAL_SURFACE ( 'NONE', #18748, 47.49900000000001654 ) ;
#31922 = AXIS2_PLACEMENT_3D ( 'NONE', #7513, #19026, #30025 ) ;
#31923 = CARTESIAN_POINT ( 'NONE',  ( -34.50000000000000000, -115.3399256288223569, -2.599147725881697291 ) ) ;
#31924 = CYLINDRICAL_SURFACE ( 'NONE', #23798, 4.800000000000000711 ) ;
#31925 = VERTEX_POINT ( 'NONE', #18473 ) ;
#31926 = ORIENTED_EDGE ( 'NONE', *, *, #31745, .T. ) ;
#31927 = CARTESIAN_POINT ( 'NONE',  ( -36.33479806579560289, -113.2509883718313262, 8.308975545821549957 ) ) ;
#31928 = AXIS2_PLACEMENT_3D ( 'NONE', #8885, #33556, #27817 ) ;
#31929 = FILL_AREA_STYLE ('',( #25476 ) ) ;
#31930 = CARTESIAN_POINT ( 'NONE',  ( 0.000000000000000000, -3.678165988948486564, -15.05623113391070866 ) ) ;
#31931 = EDGE_LOOP ( 'NONE', ( #31050, #19088, #8660, #21735 ) ) ;
#31932 = EDGE_LOOP ( 'NONE', ( #22839, #11206, #23926, #11631 ) ) ;
#31933 = CARTESIAN_POINT ( 'NONE',  ( -34.50000000000000000, -113.1061333991432321, 0.8862035858144284850 ) ) ;
#31934 = VECTOR ( 'NONE', #7268, 1000.000000000000000 ) ;
#31935 = ADVANCED_FACE ( 'NONE', ( #32510, #29833 ), #5172, .F. ) ;
#31936 = ADVANCED_FACE ( 'NONE', ( #13791 ), #8552, .T. ) ;
#31937 = ADVANCED_FACE ( 'NONE', ( #25131 ), #28882, .T. ) ;
#31938 = DIRECTION ( 'NONE',  ( 0.000000000000000000, 0.000000000000000000, 1.000000000000000000 ) ) ;
#31939 = DIRECTION ( 'NONE',  ( -1.000000000000000000, 0.000000000000000000, 0.000000000000000000 ) ) ;
#31940 = CIRCLE ( 'NONE', #34236, 20.00000000000000711 ) ;
#31941 = APPLICATION_CONTEXT ( 'automotive_design' ) ;
#31942 = CARTESIAN_POINT ( 'NONE',  ( -37.99359134332094357, -114.9929510916434339, 12.69998175888958158 ) ) ;
#31943 = DIRECTION ( 'NONE',  ( 9.314451653655516225E-17, -6.938893903907203726E-17, -1.000000000000000000 ) ) ;
#31944 = ADVANCED_FACE ( 'NONE', ( #16825 ), #10918, .T. ) ;
#31945 = CARTESIAN_POINT ( 'NONE',  ( -36.99999999999989342, -114.9929510916434339, 14.11852480586264846 ) ) ;
#31946 = DIRECTION ( 'NONE',  ( 1.000000000000000000, -4.528031003192420052E-15, -1.174092375852883160E-15 ) ) ;
#31947 = PRODUCT ( 'spring', 'spring', '', ( #9127 ) ) ;
#31948 = AXIS2_PLACEMENT_3D ( 'NONE', #11239, #2624, #13941 ) ;
#31949 = DIRECTION ( 'NONE',  ( 0.000000000000000000, 0.3090169943749415116, 0.9510565162951555296 ) ) ;
#31950 = EDGE_LOOP ( 'NONE', ( #16290, #343, #4492, #6381 ) ) ;
#31951 = CARTESIAN_POINT ( 'NONE',  ( -35.50160444427493189, -115.9929510916434481, 12.65937477241749853 ) ) ;
#31952 = CARTESIAN_POINT ( 'NONE',  ( 0.000000000000000000, 0.000000000000000000, 0.000000000000000000 ) ) ;
#31953 = FACE_OUTER_BOUND ( 'NONE', #18090, .T. ) ;
#31954 = EDGE_CURVE ( 'NONE', #6627, #29835, #27734, .T. ) ;
#31955 = DIRECTION ( 'NONE',  ( 0.000000000000000000, -0.9822872507286865007, -0.1873813145857356477 ) ) ;
#31956 = DIRECTION ( 'NONE',  ( 0.000000000000000000, 0.000000000000000000, 1.000000000000000000 ) ) ;
#31957 = ORIENTED_EDGE ( 'NONE', *, *, #24224, .T. ) ;
#31958 = DIRECTION ( 'NONE',  ( -1.000000000000000000, 0.000000000000000000, -0.000000000000000000 ) ) ;
#31959 = DIRECTION ( 'NONE',  ( 1.000000000000000000, 0.000000000000000000, -0.000000000000000000 ) ) ;
#31960 = CARTESIAN_POINT ( 'NONE',  ( 0.000000000000000000, -13.85708833599938217, -45.43276465116679930 ) ) ;
#31961 = DIRECTION ( 'NONE',  ( 0.000000000000000000, 0.000000000000000000, -1.000000000000000000 ) ) ;
#31962 = VERTEX_POINT ( 'NONE', #5345 ) ;
#31963 = CARTESIAN_POINT ( 'NONE',  ( -37.99999999999998579, -113.9407375970686758, 2.253524454178448710 ) ) ;
#31964 = MECHANICAL_DESIGN_GEOMETRIC_PRESENTATION_REPRESENTATION (  '', ( #6670 ), #10120 ) ;
#31965 = CARTESIAN_POINT ( 'NONE',  ( -42.49999999999999289, -21.98076211353320630, 84.99999999999994316 ) ) ;
#31966 = DIRECTION ( 'NONE',  ( -1.000000000000000000, 0.000000000000000000, 0.000000000000000000 ) ) ;
#31967 = EDGE_CURVE ( 'NONE', #21828, #24050, #27664, .T. ) ;
#31968 = ORIENTED_EDGE ( 'NONE', *, *, #13487, .T. ) ;
#31969 = AXIS2_PLACEMENT_3D ( 'NONE', #27365, #5749, #30064 ) ;
#31970 = ORIENTED_EDGE ( 'NONE', *, *, #9541, .T. ) ;
#31971 = CARTESIAN_POINT ( 'NONE',  ( -44.00000000000000000, 3.711905462088098291E-31, 0.000000000000000000 ) ) ;
#31972 = EDGE_CURVE ( 'NONE', #32783, #26597, #24955, .T. ) ;
#31973 = LINE ( 'NONE', #21164, #4768 ) ;
#31974 = EDGE_LOOP ( 'NONE', ( #7846, #31307, #2057, #9729 ) ) ;
#31975 = CARTESIAN_POINT ( 'NONE',  ( -39.16322519054178741, -111.9205845034225177, 7.933975545821553510 ) ) ;
#31976 = ORIENTED_EDGE ( 'NONE', *, *, #21115, .T. ) ;
#31977 = FACE_OUTER_BOUND ( 'NONE', #2287, .T. ) ;
#31978 = VERTEX_POINT ( 'NONE', #22236 ) ;
#31979 = EDGE_LOOP ( 'NONE', ( #13353, #4052 ) ) ;
#31980 = DIRECTION ( 'NONE',  ( -1.000000000000000000, 0.000000000000000000, 0.000000000000000000 ) ) ;
#31981 = CIRCLE ( 'NONE', #2679, 20.00000000000000711 ) ;
#31982 = DIRECTION ( 'NONE',  ( -1.000000000000000000, 0.000000000000000000, 0.000000000000000000 ) ) ;
#31983 = EDGE_CURVE ( 'NONE', #33223, #1657, #32321, .T. ) ;
#31984 = EDGE_CURVE ( 'NONE', #9824, #11644, #8180, .T. ) ;
#31985 = CIRCLE ( 'NONE', #7254, 8.000000000000007105 ) ;
#31986 = PLANE ( 'NONE',  #3600 ) ;
#31987 = ORIENTED_EDGE ( 'NONE', *, *, #33311, .F. ) ;
#31988 = ORIENTED_EDGE ( 'NONE', *, *, #29968, .T. ) ;
#31989 = CIRCLE ( 'NONE', #6129, 14.00000000000000000 ) ;
#31990 = DIRECTION ( 'NONE',  ( -1.000000000000000000, -0.000000000000000000, -0.000000000000000000 ) ) ;
#31991 = DIRECTION ( 'NONE',  ( 0.02857142857142376188, 0.9995917534020517525, 3.884870526907702978E-16 ) ) ;
#31992 = EDGE_LOOP ( 'NONE', ( #23480, #15828, #24536, #20966 ) ) ;
#31993 = CARTESIAN_POINT ( 'NONE',  ( 7.999999999999992895, -42.03146605346803000, 22.12489237027305577 ) ) ;
#31994 = CIRCLE ( 'NONE', #22775, 8.000000000000005329 ) ;
#31995 = CIRCLE ( 'NONE', #2132, 47.49900000000001654 ) ;
#31996 = CARTESIAN_POINT ( 'NONE',  ( 0.000000000000000000, -49.25004636492376875, -16.68630974939810940 ) ) ;
#31997 = CARTESIAN_POINT ( 'NONE',  ( -90.00000000000002842, 0.000000000000000000, 6.938893903907228378E-15 ) ) ;
#31998 = CARTESIAN_POINT ( 'NONE',  ( -35.97545865737298953, -115.9929510916434481, 14.11837420659365527 ) ) ;
#31999 = FACE_OUTER_BOUND ( 'NONE', #18823, .T. ) ;
#32000 = CARTESIAN_POINT ( 'NONE',  ( -36.11231047232249836, -112.0245472910329880, 4.222274454178449155 ) ) ;
#32001 = CARTESIAN_POINT ( 'NONE',  ( -34.50000000000000000, -115.9929510916434481, 11.21034663311132107 ) ) ;
#32002 = CARTESIAN_POINT ( 'NONE',  ( 0.000000000000000000, -14.18878633068162998, 6.236773481718038248 ) ) ;
#32003 = DIRECTION ( 'NONE',  ( -1.000000000000000000, 0.000000000000000000, 0.000000000000000000 ) ) ;
#32004 = AXIS2_PLACEMENT_3D ( 'NONE', #21041, #29537, #35299 ) ;
#32005 = DIRECTION ( 'NONE',  ( 0.000000000000000000, 0.000000000000000000, 1.000000000000000000 ) ) ;
#32006 = CARTESIAN_POINT ( 'NONE',  ( 9.714451465470119729E-14, 0.9999999999999870104, -44.50000000000000000 ) ) ;
#32007 = AXIS2_PLACEMENT_3D ( 'NONE', #26124, #27327, #16138 ) ;
#32008 = DIRECTION ( 'NONE',  ( 0.000000000000000000, -0.9510565162951500895, -0.3090169943749579429 ) ) ;
#32009 = CARTESIAN_POINT ( 'NONE',  ( 7.999999999999992895, -43.83938735307282997, 18.28286404005782728 ) ) ;
#32010 = ORIENTED_EDGE ( 'NONE', *, *, #26220, .T. ) ;
#32011 = CARTESIAN_POINT ( 'NONE',  ( -35.02454729103298803, -113.1123104723225197, 5.402725545821551734 ) ) ;
#32012 = CYLINDRICAL_SURFACE ( 'NONE', #22687, 8.000000000000001776 ) ;
#32013 = VECTOR ( 'NONE', #35576, 1000.000000000000000 ) ;
#32014 = CARTESIAN_POINT ( 'NONE',  ( -35.50000000000000000, -113.0140978167137860, 0.8752176474016654106 ) ) ;
#32015 = ADVANCED_FACE ( 'NONE', ( #626 ), #30178, .F. ) ;
#32016 = VERTEX_POINT ( 'NONE', #8723 ) ;
#32017 = ORIENTED_EDGE ( 'NONE', *, *, #26389, .F. ) ;
#32018 = AXIS2_PLACEMENT_3D ( 'NONE', #2589, #13381, #35351 ) ;
#32019 = EDGE_CURVE ( 'NONE', #5508, #26760, #1273, .T. ) ;
#32020 = DIRECTION ( 'NONE',  ( 0.000000000000000000, 0.000000000000000000, 1.000000000000000000 ) ) ;
#32021 = CARTESIAN_POINT ( 'NONE',  ( -50.00000000000000000, 9.797174393178825657E-16, -8.000000000000000000 ) ) ;
#32022 = VERTEX_POINT ( 'NONE', #32702 ) ;
#32023 = AXIS2_PLACEMENT_3D ( 'NONE', #30023, #33071, #19536 ) ;
#32024 = ORIENTED_EDGE ( 'NONE', *, *, #21599, .T. ) ;
#32025 = VERTEX_POINT ( 'NONE', #33234 ) ;
#32026 = VECTOR ( 'NONE', #5151, 1000.000000000000000 ) ;
#32027 = DIRECTION ( 'NONE',  ( -1.000000000000000000, 0.000000000000000000, 0.000000000000000000 ) ) ;
#32028 = CARTESIAN_POINT ( 'NONE',  ( 4.000000000000003553, 51.19683565102457834, -9.104066087302935983 ) ) ;
#32029 = DIRECTION ( 'NONE',  ( 1.000000000000000000, 0.000000000000000000, 0.000000000000000000 ) ) ;
#32030 = DIRECTION ( 'NONE',  ( -1.000000000000000000, -1.836970198721029934E-16, -0.000000000000000000 ) ) ;
#32031 = VECTOR ( 'NONE', #34900, 1000.000000000000000 ) ;
#32032 = ORIENTED_EDGE ( 'NONE', *, *, #29960, .F. ) ;
#32033 = ORIENTED_EDGE ( 'NONE', *, *, #27567, .F. ) ;
#32034 = CARTESIAN_POINT ( 'NONE',  ( -35.50000000000000711, -112.0140978167138712, -0.1247823525984259746 ) ) ;
#32035 = VECTOR ( 'NONE', #15723, 1000.000000000000000 ) ;
#32036 = LINE ( 'NONE', #9533, #12834 ) ;
#32037 = DIRECTION ( 'NONE',  ( -1.000000000000000000, 0.000000000000000000, -0.000000000000000000 ) ) ;
#32038 = ORIENTED_EDGE ( 'NONE', *, *, #9326, .T. ) ;
#32039 = LINE ( 'NONE', #12955, #31027 ) ;
#32040 = CIRCLE ( 'NONE', #15359, 4.800000000000003375 ) ;
#32041 = CARTESIAN_POINT ( 'NONE',  ( -34.50000000000000000, -112.6605569508015350, 1.812590711673265575 ) ) ;
#32042 = CIRCLE ( 'NONE', #11357, 4.000000000000003553 ) ;
#32043 = CARTESIAN_POINT ( 'NONE',  ( -34.50000000000000000, -114.9492820284331742, 10.20776876943783940 ) ) ;
#32044 = VECTOR ( 'NONE', #29270, 1000.000000000000000 ) ;
#32045 = CARTESIAN_POINT ( 'NONE',  ( 0.000000000000000000, 0.3151488735048668666, 11.27190672109269798 ) ) ;
#32046 = CARTESIAN_POINT ( 'NONE',  ( -35.97955704204053262, -114.9929510916434339, 13.11812344617474579 ) ) ;
#32047 = FACE_OUTER_BOUND ( 'NONE', #12076, .T. ) ;
#32048 = CARTESIAN_POINT ( 'NONE',  ( -34.50000000000000000, -114.1152303497977414, 9.513755561829650986 ) ) ;
#32049 = CARTESIAN_POINT ( 'NONE',  ( 8.000000000000000000, -12.96676809804139197, -13.60411018104332292 ) ) ;
#32050 = CARTESIAN_POINT ( 'NONE',  ( -38.00000000000000711, -114.9929510916434339, 12.26648026267477043 ) ) ;
#32051 = DIRECTION ( 'NONE',  ( -1.000000000000000000, 0.000000000000000000, 0.000000000000000000 ) ) ;
#32052 = ORIENTED_EDGE ( 'NONE', *, *, #19318, .F. ) ;
#32053 = CYLINDRICAL_SURFACE ( 'NONE', #21001, 47.49900000000001654 ) ;
#32054 = CARTESIAN_POINT ( 'NONE',  ( -55.00000000000000000, -25.98076211353320275, 90.99999999999994316 ) ) ;
#32055 = EDGE_LOOP ( 'NONE', ( #30678, #16863, #9159, #34865 ) ) ;
#32056 = CARTESIAN_POINT ( 'NONE',  ( -37.99839555572501837, -114.9929510916434339, 12.65937477241748965 ) ) ;
#32057 = VERTEX_POINT ( 'NONE', #3172 ) ;
#32058 = CARTESIAN_POINT ( 'NONE',  ( -39.02454729103295961, -114.7691647218148745, 5.159774454178448266 ) ) ;
#32059 = CARTESIAN_POINT ( 'NONE',  ( 0.000000000000000000, 9.508666619816651178, 19.83898331853691488 ) ) ;
#32060 = AXIS2_PLACEMENT_3D ( 'NONE', #11107, #24434, #21898 ) ;
#32061 = ORIENTED_EDGE ( 'NONE', *, *, #35267, .F. ) ;
#32062 = ORIENTED_EDGE ( 'NONE', *, *, #19863, .F. ) ;
#32063 = ADVANCED_FACE ( 'NONE', ( #19690 ), #8202, .T. ) ;
#32064 = CIRCLE ( 'NONE', #28026, 4.000000000000014211 ) ;
#32065 = CARTESIAN_POINT ( 'NONE',  ( -34.50000000000000000, -113.0140978167136581, -0.6247823525984268489 ) ) ;
#32066 = DIRECTION ( 'NONE',  ( -1.000000000000000000, 0.000000000000000000, 0.000000000000000000 ) ) ;
#32067 = EDGE_LOOP ( 'NONE', ( #34104, #17515, #729, #34414 ) ) ;
#32068 = CARTESIAN_POINT ( 'NONE',  ( -35.54388159064475872, -112.6276912846090568, 8.816024454178448266 ) ) ;
#32069 = AXIS2_PLACEMENT_3D ( 'NONE', #9163, #23204, #22841 ) ;
#32070 = AXIS2_PLACEMENT_3D ( 'NONE', #30606, #13870, #33310 ) ;
#32071 = CYLINDRICAL_SURFACE ( 'NONE', #26873, 20.00000000000000355 ) ;
#32072 = FACE_OUTER_BOUND ( 'NONE', #22708, .T. ) ;
#32073 = ORIENTED_EDGE ( 'NONE', *, *, #15628, .T. ) ;
#32074 = ORIENTED_EDGE ( 'NONE', *, *, #25481, .F. ) ;
#32075 = DIRECTION ( 'NONE',  ( 0.000000000000000000, 0.000000000000000000, 1.000000000000000000 ) ) ;
#32076 = EDGE_CURVE ( 'NONE', #23216, #18735, #31753, .T. ) ;
#32077 = CIRCLE ( 'NONE', #21134, 4.800000000000004263 ) ;
#32078 = SHAPE_REPRESENTATION_RELATIONSHIP ( 'NONE' , 'NONE' ,  #18063, #13375 ) ;
#32079 = PLANE ( 'NONE',  #22464 ) ;
#32080 = ORIENTED_EDGE ( 'NONE', *, *, #3765, .F. ) ;
#32081 = ORIENTED_EDGE ( 'NONE', *, *, #8594, .T. ) ;
#32082 = CARTESIAN_POINT ( 'NONE',  ( -34.50000000000000000, -114.8474311500471572, -2.624782352598442614 ) ) ;
#32083 = CARTESIAN_POINT ( 'NONE',  ( 7.999999999999992895, 0.000000000000000000, 0.000000000000000000 ) ) ;
#32084 = ORIENTED_EDGE ( 'NONE', *, *, #24670, .T. ) ;
#32085 = ORIENTED_EDGE ( 'NONE', *, *, #6011, .T. ) ;
#32086 = CARTESIAN_POINT ( 'NONE',  ( 7.999999999999992895, 47.22458491092821475, 5.098390039074404356 ) ) ;
#32087 = VECTOR ( 'NONE', #2234, 1000.000000000000000 ) ;
#32088 = CARTESIAN_POINT ( 'NONE',  ( -38.00000000000000711, -113.9929510916434339, 12.39849696637031151 ) ) ;
#32089 = DIRECTION ( 'NONE',  ( 1.000000000000000000, -5.339440136655842133E-16, -1.047965281155519420E-16 ) ) ;
#32090 = DIRECTION ( 'NONE',  ( 0.000000000000000000, 0.000000000000000000, 1.000000000000000000 ) ) ;
#32091 = CARTESIAN_POINT ( 'NONE',  ( -34.50000000000000000, -113.9465028010160381, 10.50071319044726081 ) ) ;
#32092 = CIRCLE ( 'NONE', #5655, 47.49900000000003075 ) ;
#32093 = CARTESIAN_POINT ( 'NONE',  ( -37.46874999999995737, -115.9929510916434481, 13.11852480586264846 ) ) ;
#32094 = LINE ( 'NONE', #2230, #8409 ) ;
#32095 = VECTOR ( 'NONE', #7533, 1000.000000000000000 ) ;
#32096 = CARTESIAN_POINT ( 'NONE',  ( 63.00000000000001421, -25.01350700525240356, 84.74619386235809770 ) ) ;
#32097 = VERTEX_POINT ( 'NONE', #5862 ) ;
#32098 = DIRECTION ( 'NONE',  ( 0.000000000000000000, 0.000000000000000000, 1.000000000000000000 ) ) ;
#32099 = CARTESIAN_POINT ( 'NONE',  ( 0.000000000000000000, -0.9861715913088822116, 17.47118961583599273 ) ) ;
#32100 = DIRECTION ( 'NONE',  ( -1.000000000000000000, 0.000000000000000000, 0.000000000000000000 ) ) ;
#32101 = ORIENTED_EDGE ( 'NONE', *, *, #4506, .F. ) ;
#32102 = CARTESIAN_POINT ( 'NONE',  ( 7.999999999999992895, -44.75336757549789013, 14.30704879393590545 ) ) ;
#32103 = EDGE_CURVE ( 'NONE', #31127, #11512, #11616, .T. ) ;
#32104 = CARTESIAN_POINT ( 'NONE',  ( -35.50000000000000711, -112.6919296022648638, -1.573728109100751116 ) ) ;
#32105 = DIRECTION ( 'NONE',  ( 0.000000000000000000, 0.000000000000000000, -1.000000000000000000 ) ) ;
#32106 = EDGE_CURVE ( 'NONE', #6382, #33849, #12199, .T. ) ;
#32107 = CARTESIAN_POINT ( 'NONE',  ( -35.50000000000000711, -114.5636144531578680, 9.676196722963288366 ) ) ;
#32108 = DIRECTION ( 'NONE',  ( 0.000000000000000000, 0.000000000000000000, -1.000000000000000000 ) ) ;
#32109 = ORIENTED_EDGE ( 'NONE', *, *, #11042, .T. ) ;
#32110 = DIRECTION ( 'NONE',  ( 0.000000000000000000, 0.000000000000000000, -1.000000000000000000 ) ) ;
#32111 = CARTESIAN_POINT ( 'NONE',  ( -35.50000000000000000, -111.0140978167138570, 0.5627176474015715968 ) ) ;
#32112 = FACE_OUTER_BOUND ( 'NONE', #11063, .T. ) ;
#32113 = EDGE_LOOP ( 'NONE', ( #35315, #1834, #3069, #25246 ) ) ;
#32114 = ORIENTED_EDGE ( 'NONE', *, *, #27311, .F. ) ;
#32115 = CARTESIAN_POINT ( 'NONE',  ( -36.02454729103298092, -114.4734759653044307, 6.097274454178449155 ) ) ;
#32116 = VECTOR ( 'NONE', #32566, 1000.000000000000000 ) ;
#32117 = EDGE_CURVE ( 'NONE', #11984, #17379, #26579, .T. ) ;
#32118 = LINE ( 'NONE', #29251, #16394 ) ;
#32119 = ORIENTED_EDGE ( 'NONE', *, *, #13452, .F. ) ;
#32120 = ORIENTED_EDGE ( 'NONE', *, *, #14284, .F. ) ;
#32121 = VECTOR ( 'NONE', #35550, 1000.000000000000000 ) ;
#32122 = CARTESIAN_POINT ( 'NONE',  ( -34.50000000000000000, -115.0140978167134165, -0.6247823525984399495 ) ) ;
#32123 = CARTESIAN_POINT ( 'NONE',  ( 7.999999999999992895, -41.20225022064621356, -23.63323037071446464 ) ) ;
#32124 = LINE ( 'NONE', #7093, #20833 ) ;
#32125 = CARTESIAN_POINT ( 'NONE',  ( -38.00000000000000711, -114.9929510916434339, 11.73841344789285657 ) ) ;
#32126 = LINE ( 'NONE', #4949, #34530 ) ;
#32127 = CARTESIAN_POINT ( 'NONE',  ( -34.50000000000000000, -112.3465879560236687, 1.629585756119413364 ) ) ;
#32128 = EDGE_CURVE ( 'NONE', #1546, #31584, #26007, .T. ) ;
#32129 = CARTESIAN_POINT ( 'NONE',  ( -34.50000000000000000, -114.9929510916434339, 12.44250253426871033 ) ) ;
#32130 = CARTESIAN_POINT ( 'NONE',  ( 7.999999999999992895, 37.91532898920963390, -28.61088654061597225 ) ) ;
#32131 = CARTESIAN_POINT ( 'NONE',  ( 0.000000000000000000, -0.3151488735046864553, -11.27190672109269798 ) ) ;
#32132 = ORIENTED_EDGE ( 'NONE', *, *, #26520, .F. ) ;
#32133 = AXIS2_PLACEMENT_3D ( 'NONE', #20987, #9671, #23345 ) ;
#32134 = CARTESIAN_POINT ( 'NONE',  ( -35.50000000000000000, -115.9929510916434481, 12.39849696637031684 ) ) ;
#32135 = CARTESIAN_POINT ( 'NONE',  ( -35.50000000000000711, -112.9813730236132585, -1.624774171495860786 ) ) ;
#32136 = LINE ( 'NONE', #7466, #23121 ) ;
#32137 = DIRECTION ( 'NONE',  ( -1.000000000000000000, 0.000000000000000000, 0.000000000000000000 ) ) ;
#32138 = CARTESIAN_POINT ( 'NONE',  ( 4.000000000000000000, 4.627536653468036720E-16, -54.99999999999999289 ) ) ;
#32139 = ORIENTED_EDGE ( 'NONE', *, *, #21565, .T. ) ;
#32140 = CIRCLE ( 'NONE', #5699, 10.99999999999999289 ) ;
#32141 = LINE ( 'NONE', #18450, #32026 ) ;
#32142 = DIRECTION ( 'NONE',  ( 0.000000000000000000, -0.5877852522924621459, -0.8090169943749553338 ) ) ;
#32143 = EDGE_CURVE ( 'NONE', #18651, #17346, #30601, .T. ) ;
#32144 = CARTESIAN_POINT ( 'NONE',  ( 70.00000600000001327, -25.98076211353320986, 80.99999999999992895 ) ) ;
#32145 = DIRECTION ( 'NONE',  ( -1.000000000000000000, 0.000000000000000000, 0.000000000000000000 ) ) ;
#32146 = EDGE_CURVE ( 'NONE', #25177, #34234, #19652, .T. ) ;
#32147 = EDGE_CURVE ( 'NONE', #15756, #7835, #8732, .T. ) ;
#32148 = CARTESIAN_POINT ( 'NONE',  ( -36.94073759706866156, -113.0000000000000000, 7.128524454178450043 ) ) ;
#32149 = CARTESIAN_POINT ( 'NONE',  ( -34.49999999999998579, -11.24969279549607748, 111.5585998451919778 ) ) ;
#32150 = CARTESIAN_POINT ( 'NONE',  ( -9.999999999999994671, 0.000000000000000000, 0.000000000000000000 ) ) ;
#32151 = VERTEX_POINT ( 'NONE', #22579 ) ;
#32152 = ORIENTED_EDGE ( 'NONE', *, *, #17197, .T. ) ;
#32153 = DIRECTION ( 'NONE',  ( -1.000000000000000000, 0.000000000000000000, 0.000000000000000000 ) ) ;
#32154 = CARTESIAN_POINT ( 'NONE',  ( 50.00000000000000711, -2.726571689596996976E-14, 114.0000000000000000 ) ) ;
#32155 = ORIENTED_EDGE ( 'NONE', *, *, #12113, .F. ) ;
#32156 = CARTESIAN_POINT ( 'NONE',  ( -35.54388159064475872, -115.3723087153909432, 8.683975545821551734 ) ) ;
#32157 = ADVANCED_FACE ( 'NONE', ( #28183 ), #23295, .T. ) ;
#32158 = ORIENTED_EDGE ( 'NONE', *, *, #26046, .F. ) ;
#32159 = EDGE_CURVE ( 'NONE', #24324, #26535, #2452, .T. ) ;
#32160 = FACE_OUTER_BOUND ( 'NONE', #1999, .T. ) ;
#32161 = ORIENTED_EDGE ( 'NONE', *, *, #11760, .F. ) ;
#32162 = ORIENTED_EDGE ( 'NONE', *, *, #26640, .T. ) ;
#32163 = DIRECTION ( 'NONE',  ( 0.000000000000000000, 0.000000000000000000, 1.000000000000000000 ) ) ;
#32164 = AXIS2_PLACEMENT_3D ( 'NONE', #34887, #21709, #2836 ) ;
#32165 = CARTESIAN_POINT ( 'NONE',  ( 0.000000000000000000, -7.317194182740271557, 18.61340026142649506 ) ) ;
#32166 = ORIENTED_EDGE ( 'NONE', *, *, #27794, .T. ) ;
#32167 = ORIENTED_EDGE ( 'NONE', *, *, #32537, .T. ) ;
#32168 = CIRCLE ( 'NONE', #12643, 20.00000000000000355 ) ;
#32169 = CARTESIAN_POINT ( 'NONE',  ( 8.000000000000000000, 16.31134495048494060, -6.336799421339643246 ) ) ;
#32170 = CARTESIAN_POINT ( 'NONE',  ( 0.000000000000000000, 2.123073309835863842, -47.45152853935333326 ) ) ;
#32172 = ORIENTED_EDGE ( 'NONE', *, *, #10966, .T. ) ;
#32171 = VECTOR ( 'NONE', #33334, 1000.000000000000000 ) ;
#32173 = DIRECTION ( 'NONE',  ( 1.000000000000000000, -0.000000000000000000, -0.000000000000000000 ) ) ;
#32174 = EDGE_CURVE ( 'NONE', #24192, #32530, #14473, .T. ) ;
#32175 = CARTESIAN_POINT ( 'NONE',  ( -2.321707774797454604, -4.824281976789094095, 0.000000000000000000 ) ) ;
#32176 = DIRECTION ( 'NONE',  ( 0.000000000000000000, -0.9848077530122062440, -0.1736481776669404065 ) ) ;
#32177 = EDGE_CURVE ( 'NONE', #34599, #5076, #28314, .T. ) ;
#32178 = LINE ( 'NONE', #12377, #25526 ) ;
#32179 = CARTESIAN_POINT ( 'NONE',  ( -38.37230871539094323, -112.5438815906447729, 8.441024454178448266 ) ) ;
#32180 = EDGE_CURVE ( 'NONE', #26214, #26454, #6430, .T. ) ;
#32181 = CARTESIAN_POINT ( 'NONE',  ( -34.50000000000000000, -115.9929492010520846, 10.50058572605509966 ) ) ;
#32182 = CARTESIAN_POINT ( 'NONE',  ( -29.99999999999998579, -45.00000000000000000, 0.000000000000000000 ) ) ;
#32183 = DIRECTION ( 'NONE',  ( 0.000000000000000000, 0.000000000000000000, 1.000000000000000000 ) ) ;
#32184 = LINE ( 'NONE', #26076, #949 ) ;
#32185 = DIRECTION ( 'NONE',  ( -1.000000000000000000, 0.000000000000000000, 0.000000000000000000 ) ) ;
#32186 = CARTESIAN_POINT ( 'NONE',  ( 7.999999999999992895, 44.75336757549799671, -14.30704879393557327 ) ) ;
#32187 = DIRECTION ( 'NONE',  ( 0.000000000000000000, 0.9510565162951545304, -0.3090169943749447867 ) ) ;
#32188 = EDGE_LOOP ( 'NONE', ( #6762, #24011 ) ) ;
#32189 = EDGE_CURVE ( 'NONE', #1301, #7659, #20591, .T. ) ;
#32190 = VECTOR ( 'NONE', #33941, 1000.000000000000000 ) ;
#32191 = ADVANCED_FACE ( 'NONE', ( #6217, #17351 ), #15181, .F. ) ;
#32192 = CARTESIAN_POINT ( 'NONE',  ( -38.45611840935523418, -112.6276912846090568, 4.933975545821551734 ) ) ;
#32193 = CARTESIAN_POINT ( 'NONE',  ( -34.49999999999998579, -12.31102132296306451, 91.73752798680880005 ) ) ;
#32194 = DIRECTION ( 'NONE',  ( 1.000000000000000000, -0.000000000000000000, 0.000000000000000000 ) ) ;
#32195 = ORIENTED_EDGE ( 'NONE', *, *, #3659, .F. ) ;
#32196 = AXIS2_PLACEMENT_3D ( 'NONE', #33615, #8946, #30926 ) ;
#32197 = ORIENTED_EDGE ( 'NONE', *, *, #31759, .T. ) ;
#32198 = DIRECTION ( 'NONE',  ( 0.000000000000000000, 0.000000000000000000, -1.000000000000000000 ) ) ;
#32199 = LINE ( 'NONE', #18864, #29582 ) ;
#32200 = ORIENTED_EDGE ( 'NONE', *, *, #20900, .F. ) ;
#32201 = VERTEX_POINT ( 'NONE', #17177 ) ;
#32202 = PRODUCT_DEFINITION_FORMATION_WITH_SPECIFIED_SOURCE ( 'ANY', '', #1781, .NOT_KNOWN. ) ;
#32203 = ORIENTED_EDGE ( 'NONE', *, *, #14740, .T. ) ;
#32204 = ADVANCED_FACE ( 'NONE', ( #3700 ), #1172, .T. ) ;
#32205 = DIRECTION ( 'NONE',  ( 0.000000000000000000, 0.7705132427757861446, 0.6374239897486934092 ) ) ;
#32206 = FACE_OUTER_BOUND ( 'NONE', #34541, .T. ) ;
#32207 = CARTESIAN_POINT ( 'NONE',  ( -48.00000000000000000, -7.138824979223756331E-15, 7.572676221055035700E-15 ) ) ;
#32208 = CARTESIAN_POINT ( 'NONE',  ( 7.999999999999992895, 13.85708833599969303, 45.43276465116672114 ) ) ;
#32209 = ORIENTED_EDGE ( 'NONE', *, *, #21404, .T. ) ;
#32210 = ORIENTED_EDGE ( 'NONE', *, *, #19957, .F. ) ;
#32211 = CARTESIAN_POINT ( 'NONE',  ( -35.50000000000000711, -112.6043641208289188, 1.789429170677330649 ) ) ;
#32212 =( REPRESENTATION_RELATIONSHIP ('NONE','NONE', #26607, #2005 ) REPRESENTATION_RELATIONSHIP_WITH_TRANSFORMATION ( #1501 )SHAPE_REPRESENTATION_RELATIONSHIP( ) );
#32213 = CARTESIAN_POINT ( 'NONE',  ( 8.000000000000000000, 3.872983346207416133, -1.000000000000000000 ) ) ;
#32214 = CARTESIAN_POINT ( 'NONE',  ( -21.15833593587365513, -12.00833024919776371, 94.79903810567661537 ) ) ;
#32215 = VERTEX_POINT ( 'NONE', #6919 ) ;
#32216 = CARTESIAN_POINT ( 'NONE',  ( 0.000000000000000000, 0.000000000000000000, 9.499000000000000554 ) ) ;
#32217 = ADVANCED_FACE ( 'NONE', ( #12149 ), #11781, .T. ) ;
#32218 = CIRCLE ( 'NONE', #21281, 12.55910585664918422 ) ;
#32219 = DIRECTION ( 'NONE',  ( 1.000000000000000000, -0.000000000000000000, -0.000000000000000000 ) ) ;
#32220 = EDGE_CURVE ( 'NONE', #18539, #5366, #25663, .T. ) ;
#32221 = CARTESIAN_POINT ( 'NONE',  ( -34.50000000000000000, -114.9929510916434339, 12.56351784598954424 ) ) ;
#32222 = CYLINDRICAL_SURFACE ( 'NONE', #35578, 20.00000000000000711 ) ;
#32223 = CARTESIAN_POINT ( 'NONE',  ( -37.24999999999992895, -114.9929510916434339, 13.11852480586264669 ) ) ;
#32224 = DIRECTION ( 'NONE',  ( -1.000000000000000000, 0.000000000000000000, 0.000000000000000000 ) ) ;
#32225 = AXIS2_PLACEMENT_3D ( 'NONE', #4260, #15557, #6940 ) ;
#32226 = CIRCLE ( 'NONE', #16684, 3.799999999999999822 ) ;
#32227 = CARTESIAN_POINT ( 'NONE',  ( -39.00000000000000000, -113.9929510916434339, 10.50625754673587053 ) ) ;
#32228 = CARTESIAN_POINT ( 'NONE',  ( 8.000000000000000000, 0.000000000000000000, 0.000000000000000000 ) ) ;
#32229 = CARTESIAN_POINT ( 'NONE',  ( -38.00000000000000711, -114.9929510916434339, 12.56351784598954779 ) ) ;
#32230 = ORIENTED_EDGE ( 'NONE', *, *, #28822, .F. ) ;
#32231 = PLANE ( 'NONE',  #7775 ) ;
#32232 = LINE ( 'NONE', #8085, #4858 ) ;
#32233 = ORIENTED_EDGE ( 'NONE', *, *, #23106, .F. ) ;
#32234 = CARTESIAN_POINT ( 'NONE',  ( -37.49414064056234253, -114.9929510916434339, 13.11852578240983291 ) ) ;
#32235 = ORIENTED_EDGE ( 'NONE', *, *, #18685, .F. ) ;
#32236 = ADVANCED_FACE ( 'NONE', ( #9090 ), #996, .T. ) ;
#32237 = CARTESIAN_POINT ( 'NONE',  ( -36.11231047232249125, -112.0245472910329880, 5.722274454178448266 ) ) ;
#32238 = ADVANCED_FACE ( 'NONE', ( #20223 ), #17345, .T. ) ;
#32239 = DIRECTION ( 'NONE',  ( -1.000000000000000000, 0.000000000000000000, 0.000000000000000000 ) ) ;
#32240 = ORIENTED_EDGE ( 'NONE', *, *, #12153, .F. ) ;
#32241 = VERTEX_POINT ( 'NONE', #31407 ) ;
#32242 = PLANE ( 'NONE',  #15719 ) ;
#32243 = AXIS2_PLACEMENT_3D ( 'NONE', #13925, #3488, #14438 ) ;
#32244 = VERTEX_POINT ( 'NONE', #24038 ) ;
#32245 = CARTESIAN_POINT ( 'NONE',  ( -38.18337828418795965, -110.9754527089670546, 2.534774454178448710 ) ) ;
#32246 = CIRCLE ( 'NONE', #9234, 15.49899999999998634 ) ;
#32247 = FACE_OUTER_BOUND ( 'NONE', #562, .T. ) ;
#32248 = LINE ( 'NONE', #23974, #33788 ) ;
#32249 = VERTEX_POINT ( 'NONE', #29793 ) ;
#32250 = VERTEX_POINT ( 'NONE', #23486 ) ;
#32251 = CARTESIAN_POINT ( 'NONE',  ( 70.00000600000001327, -25.98076211353320986, 80.99999999999992895 ) ) ;
#32252 = AXIS2_PLACEMENT_3D ( 'NONE', #27424, #13901, #24539 ) ;
#32253 = COLOUR_RGB ( '', 0.66274510, 0.83137255, 0.94901961) ;
#32254 = CIRCLE ( 'NONE', #20140, 3.799999999999999822 ) ;
#32255 = SURFACE_STYLE_FILL_AREA ( #21256 ) ;
#32256 = AXIS2_PLACEMENT_3D ( 'NONE', #21741, #33269, #32918 ) ;
#32257 = DIRECTION ( 'NONE',  ( 1.000000000000000000, -0.000000000000000000, -0.000000000000000000 ) ) ;
#32258 = ORIENTED_EDGE ( 'NONE', *, *, #25078, .T. ) ;
#32259 = ORIENTED_EDGE ( 'NONE', *, *, #28894, .T. ) ;
#32260 = CARTESIAN_POINT ( 'NONE',  ( -34.50000000000000000, -112.4803765279500993, 2.803636946313094569 ) ) ;
#32261 = PRODUCT_DEFINITION_SHAPE ( 'NONE', 'NONE',  #35641 ) ;
#32262 = DIRECTION ( 'NONE',  ( 0.000000000000000000, 0.000000000000000000, 1.000000000000000000 ) ) ;
#32263 = VERTEX_POINT ( 'NONE', #4417 ) ;
#32264 = CARTESIAN_POINT ( 'NONE',  ( 3.799999999999999822, 0.000000000000000000, -55.89999999999999858 ) ) ;
#32265 = EDGE_CURVE ( 'NONE', #26231, #20005, #26603, .T. ) ;
#32266 = CARTESIAN_POINT ( 'NONE',  ( -34.50000000000000000, -113.8814751941377352, 10.49295109164313722 ) ) ;
#32267 = CARTESIAN_POINT ( 'NONE',  ( 0.000000000000000000, 46.87740477351717061, -3.172455868805379442 ) ) ;
#32268 = CARTESIAN_POINT ( 'NONE',  ( 7.999999999999992895, 0.000000000000000000, 0.000000000000000000 ) ) ;
#32269 = CARTESIAN_POINT ( 'NONE',  ( -38.00000068757622529, -113.9929510916434339, 12.61439929482944855 ) ) ;
#32270 = CARTESIAN_POINT ( 'NONE',  ( -37.62959469683911351, -115.9929510916434481, 13.10254527216511633 ) ) ;
#32271 = CARTESIAN_POINT ( 'NONE',  ( 55.00000000000000000, -2.775557561562891351E-14, 110.0000000000000000 ) ) ;
#32272 = DIRECTION ( 'NONE',  ( 1.174092375852890457E-15, -4.222049128630259891E-16, -1.000000000000000000 ) ) ;
#32273 = VERTEX_POINT ( 'NONE', #2263 ) ;
#32274 = CIRCLE ( 'NONE', #24799, 20.00000000000000355 ) ;
#32275 =( GEOMETRIC_REPRESENTATION_CONTEXT ( 3 ) GLOBAL_UNCERTAINTY_ASSIGNED_CONTEXT ( ( #3849 ) ) GLOBAL_UNIT_ASSIGNED_CONTEXT ( ( #12860, #23113, #29250 ) ) REPRESENTATION_CONTEXT ( 'NONE', 'WORKASPACE' ) );
#32276 = CARTESIAN_POINT ( 'NONE',  ( 70.00000000000001421, -30.47068043442695284, 88.33026027086506815 ) ) ;
#32277 = FACE_OUTER_BOUND ( 'NONE', #32055, .T. ) ;
#32278 = AXIS2_PLACEMENT_3D ( 'NONE', #12594, #12233, #33843 ) ;
#32279 = DIRECTION ( 'NONE',  ( 1.000000000000000000, -0.000000000000000000, -0.000000000000000000 ) ) ;
#32280 = VERTEX_POINT ( 'NONE', #15360 ) ;
#32281 = DIRECTION ( 'NONE',  ( -1.000000000000000000, 0.000000000000000000, -0.000000000000000000 ) ) ;
#32282 = CARTESIAN_POINT ( 'NONE',  ( -35.50000000000000711, -112.0140978167138712, 0.7189676474015718188 ) ) ;
#32283 = LINE ( 'NONE', #7433, #6355 ) ;
#32284 = CARTESIAN_POINT ( 'NONE',  ( -35.50000000000000711, -114.9860996047076895, 10.38555023491505835 ) ) ;
#32285 = CARTESIAN_POINT ( 'NONE',  ( 4.000000000000000000, 4.898587196589412829E-16, -55.89999999999999858 ) ) ;
#32286 = ORIENTED_EDGE ( 'NONE', *, *, #12416, .T. ) ;
#32287 = DIRECTION ( 'NONE',  ( 1.032573497605238773E-16, -6.938893903907203726E-17, -1.000000000000000000 ) ) ;
#32288 = CARTESIAN_POINT ( 'NONE',  ( -35.50000000000000000, -112.3697613878167658, -2.522673865603075605 ) ) ;
#32289 = EDGE_LOOP ( 'NONE', ( #21259, #2471, #24667, #6911, #11677, #5687, #34074 ) ) ;
#32290 = EDGE_LOOP ( 'NONE', ( #557, #5776, #3155, #18390 ) ) ;
#32291 = CARTESIAN_POINT ( 'NONE',  ( -38.02454729103296671, -114.3549511594417396, 6.659774454178448266 ) ) ;
#32292 = CARTESIAN_POINT ( 'NONE',  ( 7.999999999999992895, 22.43957647427161461, 41.27978878573636479 ) ) ;
#32293 = ORIENTED_EDGE ( 'NONE', *, *, #18468, .F. ) ;
#32294 = EDGE_LOOP ( 'NONE', ( #13641, #21563, #21882, #8855 ) ) ;
#32295 = CARTESIAN_POINT ( 'NONE',  ( -34.50000000000000000, -113.0140978167138712, -0.3747823525984258497 ) ) ;
#32296 = AXIS2_PLACEMENT_3D ( 'NONE', #16028, #17, #32612 ) ;
#32297 = STYLED_ITEM ( 'NONE', ( #12094 ), #14621 ) ;
#32298 = CIRCLE ( 'NONE', #6409, 7.499999999999992895 ) ;
#32299 = CARTESIAN_POINT ( 'NONE',  ( 7.999999999999992895, 0.000000000000000000, 0.000000000000000000 ) ) ;
#32300 = DIRECTION ( 'NONE',  ( -1.000000000000000000, 0.000000000000000000, 0.000000000000000000 ) ) ;
#32301 = EDGE_CURVE ( 'NONE', #21336, #7400, #13050, .T. ) ;
#32302 = CARTESIAN_POINT ( 'NONE',  ( -38.00000000000000711, -114.9929510916434339, 12.59652202191340820 ) ) ;
#32303 = DIRECTION ( 'NONE',  ( 0.000000000000000000, 0.000000000000000000, 1.000000000000000000 ) ) ;
#32304 = CARTESIAN_POINT ( 'NONE',  ( 7.999999999999992895, -15.49408907645140943, -44.90087086784610904 ) ) ;
#32305 = CARTESIAN_POINT ( 'NONE',  ( -34.50000000000000000, -112.0140978167138712, -0.3747823525984256832 ) ) ;
#32306 = DIRECTION ( 'NONE',  ( -1.000000000000000000, 0.000000000000000000, 0.000000000000000000 ) ) ;
#32307 = CARTESIAN_POINT ( 'NONE',  ( 7.999999999999992895, -46.87740477351715640, 16.82754413119429415 ) ) ;
#32308 = EDGE_LOOP ( 'NONE', ( #10491, #15210, #24852, #22924 ) ) ;
#32309 = EDGE_CURVE ( 'NONE', #19478, #23898, #32124, .T. ) ;
#32310 = CARTESIAN_POINT ( 'NONE',  ( -37.42187499999996447, -115.9929510916434481, 13.11852480586264846 ) ) ;
#32311 = FACE_OUTER_BOUND ( 'NONE', #11915, .T. ) ;
#32312 = DIRECTION ( 'NONE',  ( -1.000000000000000000, 0.000000000000000000, 0.000000000000000000 ) ) ;
#32313 = CARTESIAN_POINT ( 'NONE',  ( 7.999999999999992895, 30.93515269692114344, 36.04401931830264516 ) ) ;
#32314 = CARTESIAN_POINT ( 'NONE',  ( 7.999999999999992895, 38.92705108641771261, -27.21837053747755419 ) ) ;
#32315 = ORIENTED_EDGE ( 'NONE', *, *, #11936, .F. ) ;
#32316 = DIRECTION ( 'NONE',  ( -5.339440136655842133E-16, -1.000000000000000000, 6.938893903907197563E-17 ) ) ;
#32317 = DIRECTION ( 'NONE',  ( 0.000000000000000000, 0.000000000000000000, 1.000000000000000000 ) ) ;
#32318 = DIRECTION ( 'NONE',  ( 1.000000000000000000, 1.734723475976807094E-16, 0.000000000000000000 ) ) ;
#32319 = CARTESIAN_POINT ( 'NONE',  ( 0.000000000000000000, 37.91532898920923600, 28.61088654061652647 ) ) ;
#32320 = COLOUR_RGB ( '', 0.72549020, 0.75294118, 0.79215686) ;
#32321 = CIRCLE ( 'NONE', #16783, 9.499000000000009436 ) ;
#32322 = CARTESIAN_POINT ( 'NONE',  ( 50.00005079999998969, 0.000000000000000000, 3.000000000000002665 ) ) ;
#32323 = DIRECTION ( 'NONE',  ( -1.174092375852890260E-15, 4.222049128630259891E-16, 1.000000000000000000 ) ) ;
#32324 = VERTEX_POINT ( 'NONE', #34479 ) ;
#32325 = ORIENTED_EDGE ( 'NONE', *, *, #32180, .T. ) ;
#32326 = FACE_OUTER_BOUND ( 'NONE', #6210, .T. ) ;
#32327 = CARTESIAN_POINT ( 'NONE',  ( 0.000000000000000000, -16.59870953437678409, -3.253005020244019718 ) ) ;
#32328 = CARTESIAN_POINT ( 'NONE',  ( -42.49999999999999289, -13.17619866229195047, 79.33933265213923391 ) ) ;
#32329 = ORIENTED_EDGE ( 'NONE', *, *, #10871, .T. ) ;
#32330 = CARTESIAN_POINT ( 'NONE',  ( -38.97545270896704039, -114.8876895276775087, 6.152725545821551734 ) ) ;
#32331 = ORIENTED_EDGE ( 'NONE', *, *, #2077, .F. ) ;
#32332 = EDGE_CURVE ( 'NONE', #169, #31131, #4775, .T. ) ;
#32333 = FILL_AREA_STYLE_COLOUR ( '', #23617 ) ;
#32335 = ORIENTED_EDGE ( 'NONE', *, *, #17168, .T. ) ;
#32334 =( GEOMETRIC_REPRESENTATION_CONTEXT ( 3 ) GLOBAL_UNCERTAINTY_ASSIGNED_CONTEXT ( ( #31593 ) ) GLOBAL_UNIT_ASSIGNED_CONTEXT ( ( #27102, #26933, #19323 ) ) REPRESENTATION_CONTEXT ( 'NONE', 'WORKASPACE' ) );
#32336 = ORIENTED_EDGE ( 'NONE', *, *, #8411, .F. ) ;
#32337 = CYLINDRICAL_SURFACE ( 'NONE', #2252, 7.199999999999994849 ) ;
#32338 = CARTESIAN_POINT ( 'NONE',  ( 8.000000000000007105, -11.27190672109260028, -0.3151488735048807444 ) ) ;
#32339 = ORIENTED_EDGE ( 'NONE', *, *, #31244, .F. ) ;
#32340 = ORIENTED_EDGE ( 'NONE', *, *, #15171, .F. ) ;
#32341 = EDGE_CURVE ( 'NONE', #16937, #33676, #29482, .T. ) ;
#32342 = DIRECTION ( 'NONE',  ( 0.000000000000000000, 0.000000000000000000, -1.000000000000000000 ) ) ;
#32343 = AXIS2_PLACEMENT_3D ( 'NONE', #32268, #29926, #7588 ) ;
#32344 = CARTESIAN_POINT ( 'NONE',  ( 1.520000000000021334, 0.000000000000000000, 0.000000000000000000 ) ) ;
#32345 = EDGE_CURVE ( 'NONE', #11865, #13559, #11078, .T. ) ;
#32346 = EDGE_CURVE ( 'NONE', #26576, #25349, #17365, .T. ) ;
#32347 = AXIS2_PLACEMENT_3D ( 'NONE', #1894, #12505, #18070 ) ;
#32348 = DIRECTION ( 'NONE',  ( 0.000000000000000000, 0.000000000000000000, 1.000000000000000000 ) ) ;
#32349 = DIRECTION ( 'NONE',  ( -1.000000000000000000, 0.000000000000000000, 0.000000000000000000 ) ) ;
#32350 = DIRECTION ( 'NONE',  ( 0.000000000000000000, 0.000000000000000000, -1.000000000000000000 ) ) ;
#32351 = DIRECTION ( 'NONE',  ( 0.000000000000000000, 0.000000000000000000, 1.000000000000000000 ) ) ;
#32352 = CARTESIAN_POINT ( 'NONE',  ( -39.02454729103295961, -114.7691647218148745, 5.159774454178449155 ) ) ;
#32353 = EDGE_CURVE ( 'NONE', #20425, #577, #24872, .T. ) ;
#32354 = CARTESIAN_POINT ( 'NONE',  ( -35.24442919769867899, -115.9929510916434481, 13.92914543265605509 ) ) ;
#32355 = CARTESIAN_POINT ( 'NONE',  ( 0.000000000000000000, -0.9861715913086358531, -17.47118961583604957 ) ) ;
#32356 = EDGE_CURVE ( 'NONE', #17756, #24596, #21979, .T. ) ;
#32357 = DIRECTION ( 'NONE',  ( 0.000000000000000000, 0.9848077530122073542, 0.1736481776669339394 ) ) ;
#32358 = AXIS2_PLACEMENT_3D ( 'NONE', #26890, #27060, #2580 ) ;
#32359 = DIRECTION ( 'NONE',  ( -1.000000000000000000, 0.000000000000000000, 0.000000000000000000 ) ) ;
#32360 = CARTESIAN_POINT ( 'NONE',  ( 0.000000000000000000, 0.000000000000000000, 36.00000000000000000 ) ) ;
#32361 = VECTOR ( 'NONE', #19668, 1000.000000000000000 ) ;
#32362 = CARTESIAN_POINT ( 'NONE',  ( 0.9999999999999453770, -6.008326913195871199, 0.000000000000000000 ) ) ;
#32363 = ORIENTED_EDGE ( 'NONE', *, *, #6154, .T. ) ;
#32364 = CARTESIAN_POINT ( 'NONE',  ( -38.99999999999999289, -114.0592624029313242, 6.246475545821550845 ) ) ;
#32365 = DIRECTION ( 'NONE',  ( -1.000000000000000000, 0.000000000000000000, 0.000000000000000000 ) ) ;
#32366 = DIRECTION ( 'NONE',  ( -1.000000000000000000, 0.000000000000000000, 0.000000000000000000 ) ) ;
#32367 = ORIENTED_EDGE ( 'NONE', *, *, #6648, .F. ) ;
#32368 = ORIENTED_EDGE ( 'NONE', *, *, #667, .T. ) ;
#32369 = AXIS2_PLACEMENT_3D ( 'NONE', #81, #16259, #27277 ) ;
#32370 = CARTESIAN_POINT ( 'NONE',  ( 0.000000000000000000, -5.667686777401384823, -46.64153600743608763 ) ) ;
#32371 = CIRCLE ( 'NONE', #15673, 52.00000000000000711 ) ;
#32372 = FACE_OUTER_BOUND ( 'NONE', #28309, .T. ) ;
#32373 = ORIENTED_EDGE ( 'NONE', *, *, #30244, .F. ) ;
#32374 = CIRCLE ( 'NONE', #16830, 15.49899999999998812 ) ;
#32375 = VERTEX_POINT ( 'NONE', #21130 ) ;
#32376 = EDGE_CURVE ( 'NONE', #12193, #28461, #18611, .T. ) ;
#32377 = FACE_OUTER_BOUND ( 'NONE', #26518, .T. ) ;
#32378 = PRODUCT_DEFINITION ( 'UNKNOWN', '', #31034, #24907 ) ;
#32379 = DIRECTION ( 'NONE',  ( -1.000000000000000000, 0.000000000000000000, -0.000000000000000000 ) ) ;
#32380 = DIRECTION ( 'NONE',  ( -1.000000000000000000, 7.285838599102611983E-17, -5.551115123125798726E-17 ) ) ;
#32381 = LINE ( 'NONE', #7536, #22492 ) ;
#32382 = VERTEX_POINT ( 'NONE', #20762 ) ;
#32383 = VERTEX_POINT ( 'NONE', #10512 ) ;
#32384 = AXIS2_PLACEMENT_3D ( 'NONE', #29874, #29690, #32922 ) ;
#32385 = CARTESIAN_POINT ( 'NONE',  ( -35.50000000000000711, -112.1859307030124739, 1.448610958621386224 ) ) ;
#32386 = VECTOR ( 'NONE', #13062, 1000.000000000000000 ) ;
#32387 = EDGE_CURVE ( 'NONE', #26849, #16937, #721, .T. ) ;
#32388 = CIRCLE ( 'NONE', #5939, 17.49900000000002720 ) ;
#32389 = CARTESIAN_POINT ( 'NONE',  ( 1.799999999999996048, 0.000000000000000000, 0.000000000000000000 ) ) ;
#32390 = EDGE_CURVE ( 'NONE', #7205, #14334, #8758, .T. ) ;
#32391 = EDGE_CURVE ( 'NONE', #13336, #34584, #6462, .T. ) ;
#32392 = DIRECTION ( 'NONE',  ( 0.000000000000000000, 0.000000000000000000, -1.000000000000000000 ) ) ;
#32393 = ORIENTED_EDGE ( 'NONE', *, *, #13055, .T. ) ;
#32394 = DIRECTION ( 'NONE',  ( -1.000000000000000000, 0.000000000000000000, -0.000000000000000000 ) ) ;
#32395 = CARTESIAN_POINT ( 'NONE',  ( -34.50000000000000000, -112.0140978167138712, 0.8127176474015721519 ) ) ;
#32396 = CARTESIAN_POINT ( 'NONE',  ( -34.50000000000000000, -114.2305202833893816, 9.534416457224700991 ) ) ;
#32397 = CIRCLE ( 'NONE', #16855, 4.000000000000000000 ) ;
#32398 = FACE_OUTER_BOUND ( 'NONE', #28935, .T. ) ;
#32399 = CARTESIAN_POINT ( 'NONE',  ( -35.69272627125609176, -114.9929510916434339, 13.01835785830562209 ) ) ;
#32400 = CARTESIAN_POINT ( 'NONE',  ( 0.000000000000000000, 0.000000000000000000, 65.00000000000000000 ) ) ;
#32401 = AXIS2_PLACEMENT_3D ( 'NONE', #9788, #17164, #28171 ) ;
#32402 = CARTESIAN_POINT ( 'NONE',  ( -34.50000000000000000, -114.9929510916434339, 10.53376102667243508 ) ) ;
#32403 = DIRECTION ( 'NONE',  ( 0.000000000000000000, 0.000000000000000000, 1.000000000000000000 ) ) ;
#32404 = EDGE_CURVE ( 'NONE', #9009, #3103, #2475, .T. ) ;
#32405 = CARTESIAN_POINT ( 'NONE',  ( -42.49999999999999289, -24.48076211353301801, 67.99999999999991473 ) ) ;
#32406 = VERTEX_POINT ( 'NONE', #18429 ) ;
#32407 = FACE_BOUND ( 'NONE', #29271, .T. ) ;
#32408 = DIRECTION ( 'NONE',  ( -1.000000000000000000, 0.000000000000000000, 0.000000000000000000 ) ) ;
#32409 = ORIENTED_EDGE ( 'NONE', *, *, #3857, .F. ) ;
#32410 = CARTESIAN_POINT ( 'NONE',  ( -38.00000000000000711, -114.9929510916434339, 12.57451923796417503 ) ) ;
#32411 = ORIENTED_EDGE ( 'NONE', *, *, #4421, .F. ) ;
#32412 = CARTESIAN_POINT ( 'NONE',  ( -38.30190309005061522, -116.9754527089670546, 1.972274454178448932 ) ) ;
#32413 = LINE ( 'NONE', #23964, #7063 ) ;
#32414 = ORIENTED_EDGE ( 'NONE', *, *, #7310, .F. ) ;
#32415 = AXIS2_PLACEMENT_3D ( 'NONE', #30328, #3141, #30502 ) ;
#32416 = VERTEX_POINT ( 'NONE', #16070 ) ;
#32417 = CARTESIAN_POINT ( 'NONE',  ( 7.999999999999992895, 46.87740477351717061, 16.82754413119462455 ) ) ;
#32418 = ORIENTED_EDGE ( 'NONE', *, *, #19805, .F. ) ;
#32419 = CARTESIAN_POINT ( 'NONE',  ( -34.02454729103298092, -115.3019030900506294, 3.097274454178448710 ) ) ;
#32420 = EDGE_CURVE ( 'NONE', #19376, #34867, #11641, .T. ) ;
#32421 = CARTESIAN_POINT ( 'NONE',  ( 0.000000000000000000, 0.000000000000000000, 0.000000000000000000 ) ) ;
#32422 = CIRCLE ( 'NONE', #35318, 9.499000000000009436 ) ;
#32423 = DIRECTION ( 'NONE',  ( -1.174092375852890260E-15, 4.222049128630259891E-16, 1.000000000000000000 ) ) ;
#32424 = VECTOR ( 'NONE', #28726, 1000.000000000000000 ) ;
#32425 = EDGE_LOOP ( 'NONE', ( #22541, #22092, #17939, #34347 ) ) ;
#32427 = ORIENTED_EDGE ( 'NONE', *, *, #16834, .F. ) ;
#32426 = EDGE_CURVE ( 'NONE', #30950, #5984, #15647, .T. ) ;
#32428 = CARTESIAN_POINT ( 'NONE',  ( 70.00001200000002655, -23.96628619204960486, 88.49514555341697530 ) ) ;
#32429 = DIRECTION ( 'NONE',  ( 0.000000000000000000, 0.3090169943749477288, -0.9510565162951534202 ) ) ;
#32430 = ORIENTED_EDGE ( 'NONE', *, *, #15157, .T. ) ;
#32431 = ORIENTED_EDGE ( 'NONE', *, *, #20212, .F. ) ;
#32432 = CARTESIAN_POINT ( 'NONE',  ( -34.50000000000000000, -111.0140978167138570, -0.4997823525984338988 ) ) ;
#32433 = EDGE_CURVE ( 'NONE', #32783, #19338, #13946, .T. ) ;
#32434 = DIRECTION ( 'NONE',  ( 0.000000000000000000, 0.000000000000000000, 1.000000000000000000 ) ) ;
#32435 = ORIENTED_EDGE ( 'NONE', *, *, #18898, .T. ) ;
#32436 = EDGE_CURVE ( 'NONE', #519, #21217, #35555, .T. ) ;
#32437 = CARTESIAN_POINT ( 'NONE',  ( -35.50000000000000711, -114.0882517521923489, 9.510534276948430232 ) ) ;
#32438 = CARTESIAN_POINT ( 'NONE',  ( -34.50000000000000000, -113.9929510916434339, 10.56126450660895699 ) ) ;
#32439 = DIRECTION ( 'NONE',  ( -1.000000000000000000, 0.000000000000000000, -0.000000000000000000 ) ) ;
#32440 = DIRECTION ( 'NONE',  ( 0.000000000000000000, 0.000000000000000000, -1.000000000000000000 ) ) ;
#32441 = CARTESIAN_POINT ( 'NONE',  ( -37.99974912065192001, -113.9929510916434339, 12.63488142334838749 ) ) ;
#32442 = CARTESIAN_POINT ( 'NONE',  ( -37.99899697755054717, -115.9929510916434481, 12.65121853911336913 ) ) ;
#32443 = LINE ( 'NONE', #18752, #22763 ) ;
#32445 = VECTOR ( 'NONE', #5376, 1000.000000000000000 ) ;
#32444 = LINE ( 'NONE', #10486, #16936 ) ;
#32446 = AXIS2_PLACEMENT_3D ( 'NONE', #17642, #29188, #12616 ) ;
#32447 = EDGE_LOOP ( 'NONE', ( #10112, #33098, #12401, #21580 ) ) ;
#32448 = LINE ( 'NONE', #7956, #5179 ) ;
#32449 = DIRECTION ( 'NONE',  ( -1.000000000000000000, 0.000000000000000000, 0.000000000000000000 ) ) ;
#32450 = CYLINDRICAL_SURFACE ( 'NONE', #23759, 7.199999999999993960 ) ;
#32451 = VERTEX_POINT ( 'NONE', #2605 ) ;
#32452 = CARTESIAN_POINT ( 'NONE',  ( 0.000000000000000000, 0.000000000000000000, 0.000000000000000000 ) ) ;
#32453 = CARTESIAN_POINT ( 'NONE',  ( -35.50000000000000000, -113.0140978167138712, 0.7189676474015717078 ) ) ;
#32454 = DIRECTION ( 'NONE',  ( -1.783119874454246424E-31, -1.187911941725854497E-31, 1.000000000000000000 ) ) ;
#32455 = CARTESIAN_POINT ( 'NONE',  ( -35.50000000000000711, -114.9922651054798308, 10.46846006712531008 ) ) ;
#32456 = CYLINDRICAL_SURFACE ( 'NONE', #30301, 4.000000000000000000 ) ;
#32457 = EDGE_CURVE ( 'NONE', #3694, #2456, #13755, .T. ) ;
#32458 = ORIENTED_EDGE ( 'NONE', *, *, #21395, .F. ) ;
#32459 = EDGE_CURVE ( 'NONE', #28584, #20378, #9344, .T. ) ;
#32460 = DIRECTION ( 'NONE',  ( 0.000000000000000000, 0.000000000000000000, 1.000000000000000000 ) ) ;
#32461 = CARTESIAN_POINT ( 'NONE',  ( -35.50000000000000000, -111.0687598768285369, 1.355111303971038073 ) ) ;
#32462 = EDGE_LOOP ( 'NONE', ( #35342, #10292, #6081, #27163 ) ) ;
#32463 = ORIENTED_EDGE ( 'NONE', *, *, #33014, .T. ) ;
#32464 = CARTESIAN_POINT ( 'NONE',  ( -38.02454729103296671, -114.3549511594417396, 8.159774454178448266 ) ) ;
#32465 = DIRECTION ( 'NONE',  ( 1.000000000000000000, -1.110223024625156540E-16, 0.000000000000000000 ) ) ;
#32466 = ORIENTED_EDGE ( 'NONE', *, *, #1133, .T. ) ;
#32467 = ORIENTED_EDGE ( 'NONE', *, *, #2296, .T. ) ;
#32468 = CARTESIAN_POINT ( 'NONE',  ( -34.50000000000000000, -113.6807644833805995, -0.6247823525984269599 ) ) ;
#32469 = DIRECTION ( 'NONE',  ( -0.000000000000000000, 0.000000000000000000, -1.000000000000000000 ) ) ;
#32470 = DIRECTION ( 'NONE',  ( 0.000000000000000000, -0.3681245526846653737, -0.9297764858882564543 ) ) ;
#32471 = CARTESIAN_POINT ( 'NONE',  ( -38.00000000000000711, -114.9929510916434339, 10.85830208992306822 ) ) ;
#32472 = LINE ( 'NONE', #5134, #11518 ) ;
#32473 = DIRECTION ( 'NONE',  ( 0.000000000000000000, 0.000000000000000000, -1.000000000000000000 ) ) ;
#32474 = CARTESIAN_POINT ( 'NONE',  ( -34.50000000000000000, -112.0460568841087223, -0.8839717462762063382 ) ) ;
#32475 = VECTOR ( 'NONE', #35165, 1000.000000000000000 ) ;
#32476 = DIRECTION ( 'NONE',  ( -1.000000000000000000, 0.000000000000000000, 0.000000000000000000 ) ) ;
#32477 = CARTESIAN_POINT ( 'NONE',  ( 8.000000000000000000, -11.06713717293248855, 13.55483219355725844 ) ) ;
#32478 = ORIENTED_EDGE ( 'NONE', *, *, #241, .T. ) ;
#32479 = CARTESIAN_POINT ( 'NONE',  ( -35.50000000000000711, -114.1152303497977414, 9.513755561829650986 ) ) ;
#32480 = DIRECTION ( 'NONE',  ( -1.000000000000000000, -0.000000000000000000, 0.000000000000000000 ) ) ;
#32481 = FACE_OUTER_BOUND ( 'NONE', #7920, .T. ) ;
#32482 = DIRECTION ( 'NONE',  ( -1.000000000000000000, 0.000000000000000000, 0.000000000000000000 ) ) ;
#32483 = DIRECTION ( 'NONE',  ( 0.000000000000000000, 0.000000000000000000, 1.000000000000000000 ) ) ;
#32484 = ORIENTED_EDGE ( 'NONE', *, *, #3742, .F. ) ;
#32485 = DIRECTION ( 'NONE',  ( -1.836970198721029934E-16, 1.000000000000000000, 0.000000000000000000 ) ) ;
#32486 = DIRECTION ( 'NONE',  ( 0.000000000000000000, 0.000000000000000000, 1.000000000000000000 ) ) ;
#32487 = AXIS2_PLACEMENT_3D ( 'NONE', #15731, #4617, #34312 ) ;
#32488 = CIRCLE ( 'NONE', #24456, 4.000000000000000000 ) ;
#32489 = DIRECTION ( 'NONE',  ( -1.000000000000000000, -0.000000000000000000, 0.000000000000000000 ) ) ;
#32490 = DIRECTION ( 'NONE',  ( -1.000000000000000000, 0.000000000000000000, 0.000000000000000000 ) ) ;
#32491 = DIRECTION ( 'NONE',  ( 0.000000000000000000, 0.000000000000000000, -1.000000000000000000 ) ) ;
#32492 = CARTESIAN_POINT ( 'NONE',  ( 0.000000000000000000, 0.000000000000000000, 0.000000000000000000 ) ) ;
#32493 = VECTOR ( 'NONE', #1197, 1000.000000000000000 ) ;
#32494 = ORIENTED_EDGE ( 'NONE', *, *, #19823, .T. ) ;
#32495 = ORIENTED_EDGE ( 'NONE', *, *, #26955, .F. ) ;
#32496 = CIRCLE ( 'NONE', #11222, 8.000000000000000000 ) ;
#32497 = ADVANCED_FACE ( 'NONE', ( #14562 ), #5473, .T. ) ;
#32498 = DIRECTION ( 'NONE',  ( -1.000000000000000000, 0.000000000000000000, 0.000000000000000000 ) ) ;
#32499 = FACE_OUTER_BOUND ( 'NONE', #29510, .T. ) ;
#32500 = CARTESIAN_POINT ( 'NONE',  ( 4.000000000000000000, 19.60123832284022782, -3.973846525876241653 ) ) ;
#32501 = VERTEX_POINT ( 'NONE', #29964 ) ;
#32502 = CARTESIAN_POINT ( 'NONE',  ( -37.76916472181486739, -116.0245472910329880, 8.965225545821551734 ) ) ;
#32503 = ORIENTED_EDGE ( 'NONE', *, *, #20929, .T. ) ;
#32504 = SURFACE_SIDE_STYLE ('',( #27128 ) ) ;
#32505 = AXIS2_PLACEMENT_3D ( 'NONE', #12253, #12430, #9007 ) ;
#32506 = ORIENTED_EDGE ( 'NONE', *, *, #23305, .T. ) ;
#32507 = ORIENTED_EDGE ( 'NONE', *, *, #13421, .F. ) ;
#32508 = CYLINDRICAL_SURFACE ( 'NONE', #35035, 8.000000000000001776 ) ;
#32509 = ADVANCED_FACE ( 'NONE', ( #8157 ), #16243, .T. ) ;
#32510 = FACE_OUTER_BOUND ( 'NONE', #27332, .T. ) ;
#32511 = ORIENTED_EDGE ( 'NONE', *, *, #23090, .T. ) ;
#32512 = ORIENTED_EDGE ( 'NONE', *, *, #15695, .F. ) ;
#32513 = AXIS2_PLACEMENT_3D ( 'NONE', #4437, #23682, #32142 ) ;
#32514 = DIRECTION ( 'NONE',  ( -1.000000000000000000, 0.000000000000000000, 0.000000000000000000 ) ) ;
#32515 = CARTESIAN_POINT ( 'NONE',  ( 63.00000000000001421, -26.38406014851796400, 79.52301627764160230 ) ) ;
#32516 = DIRECTION ( 'NONE',  ( -1.000000000000000000, 0.000000000000000000, 0.000000000000000000 ) ) ;
#32517 = CIRCLE ( 'NONE', #16980, 3.799999999999999822 ) ;
#32518 = AXIS2_PLACEMENT_3D ( 'NONE', #24586, #19336, #19511 ) ;
#32519 = CYLINDRICAL_SURFACE ( 'NONE', #25148, 5.000000000000004441 ) ;
#32520 = CARTESIAN_POINT ( 'NONE',  ( 0.000000000000000000, -18.48663108841356717, -3.384281271888017084 ) ) ;
#32521 = CIRCLE ( 'NONE', #25648, 20.00000000000000711 ) ;
#32522 = CARTESIAN_POINT ( 'NONE',  ( -37.05926240293131713, -115.9999999999999858, 4.878524454178449155 ) ) ;
#32523 = CARTESIAN_POINT ( 'NONE',  ( -36.50000000000010658, -115.9929510916434481, 14.11852480586265024 ) ) ;
#32524 = DIRECTION ( 'NONE',  ( 0.000000000000000000, 0.000000000000000000, 1.000000000000000000 ) ) ;
#32525 = DIRECTION ( 'NONE',  ( 1.000000000000000000, 0.000000000000000000, -1.691777834109591064E-31 ) ) ;
#32526 = VECTOR ( 'NONE', #3414, 1000.000000000000000 ) ;
#32527 = LINE ( 'NONE', #25681, #21619 ) ;
#32528 = CYLINDRICAL_SURFACE ( 'NONE', #33611, 20.00000000000000355 ) ;
#32529 = DIRECTION ( 'NONE',  ( 0.000000000000000000, 0.000000000000000000, 1.000000000000000000 ) ) ;
#32530 = VERTEX_POINT ( 'NONE', #30966 ) ;
#32531 = CARTESIAN_POINT ( 'NONE',  ( -36.23083527818512550, -111.9754527089670404, 3.715225545821550845 ) ) ;
#32532 = DIRECTION ( 'NONE',  ( 1.174092375852885330E-15, 4.222049128630153888E-16, 1.000000000000000000 ) ) ;
#32533 = CARTESIAN_POINT ( 'NONE',  ( 4.000000000000003553, -3.968388925834960723, 21.63912866391138934 ) ) ;
#32534 = CARTESIAN_POINT ( 'NONE',  ( 0.000000000000000000, 0.000000000000000000, -40.40000000000000568 ) ) ;
#32535 = VERTEX_POINT ( 'NONE', #3614 ) ;
#32536 = ORIENTED_EDGE ( 'NONE', *, *, #1246, .F. ) ;
#32537 = EDGE_CURVE ( 'NONE', #7261, #4978, #35241, .T. ) ;
#32539 = PRESENTATION_STYLE_ASSIGNMENT (( #13470 ) ) ;
#32538 = PRODUCT_DEFINITION_SHAPE ( 'NONE', 'NONE',  #35649 ) ;
#32540 = CIRCLE ( 'NONE', #16436, 9.499000000000000554 ) ;
#32541 = FACE_BOUND ( 'NONE', #4283, .T. ) ;
#32542 = ORIENTED_EDGE ( 'NONE', *, *, #8000, .T. ) ;
#32543 = EDGE_CURVE ( 'NONE', #18045, #1374, #19136, .T. ) ;
#32544 = ORIENTED_EDGE ( 'NONE', *, *, #30556, .F. ) ;
#32545 = AXIS2_PLACEMENT_3D ( 'NONE', #3802, #14760, #3988 ) ;
#32546 = AXIS2_PLACEMENT_3D ( 'NONE', #25200, #19427, #2888 ) ;
#32547 = VECTOR ( 'NONE', #9822, 1000.000000000000000 ) ;
#32548 = CARTESIAN_POINT ( 'NONE',  ( 7.999999999999992895, 0.000000000000000000, 0.000000000000000000 ) ) ;
#32549 = CARTESIAN_POINT ( 'NONE',  ( -35.02454729103298092, -113.1123104723225055, 8.402725545821551734 ) ) ;
#32550 = EDGE_CURVE ( 'NONE', #17170, #27299, #23131, .T. ) ;
#32551 = CIRCLE ( 'NONE', #27960, 3.799999999999999822 ) ;
#32552 = DIRECTION ( 'NONE',  ( 1.000000000000000000, 0.000000000000000000, 0.000000000000000000 ) ) ;
#32553 = DIRECTION ( 'NONE',  ( 0.000000000000000000, 0.000000000000000000, 1.000000000000000000 ) ) ;
#32555 = ORIENTED_EDGE ( 'NONE', *, *, #19666, .F. ) ;
#32554 = AXIS2_PLACEMENT_3D ( 'NONE', #3540, #25867, #14317 ) ;
#32556 = ORIENTED_EDGE ( 'NONE', *, *, #13449, .F. ) ;
#32557 = CARTESIAN_POINT ( 'NONE',  ( -35.50000000000000711, -112.8511839106603247, -1.611965039240275122 ) ) ;
#32558 = DIRECTION ( 'NONE',  ( 0.000000000000000000, 0.000000000000000000, 1.000000000000000000 ) ) ;
#32559 = CARTESIAN_POINT ( 'NONE',  ( 7.999999999999992895, -41.20225022064621356, -23.63323037071446464 ) ) ;
#32560 = EDGE_LOOP ( 'NONE', ( #1727, #10731, #31176, #21690 ) ) ;
#32561 = FACE_OUTER_BOUND ( 'NONE', #5251, .T. ) ;
#32562 = CIRCLE ( 'NONE', #18843, 20.00000000000000711 ) ;
#32563 = CARTESIAN_POINT ( 'NONE',  ( -34.50000000000000000, -116.0141056290913610, -0.5935324770972248976 ) ) ;
#32564 = CARTESIAN_POINT ( 'NONE',  ( -37.69578139638701941, -114.9929510916434339, 14.10650203519847778 ) ) ;
#32565 = VECTOR ( 'NONE', #13637, 1000.000000000000000 ) ;
#32566 = DIRECTION ( 'NONE',  ( 0.000000000000000000, 1.000000000000000000, 0.000000000000000000 ) ) ;
#32567 = CARTESIAN_POINT ( 'NONE',  ( -35.50000000000000000, -113.9929510916432207, 10.50625754673563250 ) ) ;
#32568 = DIRECTION ( 'NONE',  ( -1.000000000000000000, -0.000000000000000000, -0.000000000000000000 ) ) ;
#32569 = CARTESIAN_POINT ( 'NONE',  ( -34.50000000000000000, -114.9860996047076895, 10.38555023491505835 ) ) ;
#32570 = DIRECTION ( 'NONE',  ( -1.000000000000000000, 0.000000000000000000, 0.000000000000000000 ) ) ;
#32571 = EDGE_CURVE ( 'NONE', #12650, #5366, #12229, .T. ) ;
#32572 = CIRCLE ( 'NONE', #17032, 4.000000000000000000 ) ;
#32573 = CARTESIAN_POINT ( 'NONE',  ( -21.15833593587365513, -22.68172400785649501, 82.28589838486220742 ) ) ;
#32574 = PRESENTATION_STYLE_ASSIGNMENT (( #16172 ) ) ;
#32575 = ORIENTED_EDGE ( 'NONE', *, *, #12873, .F. ) ;
#32576 = VECTOR ( 'NONE', #13948, 1000.000000000000000 ) ;
#32577 = CARTESIAN_POINT ( 'NONE',  ( 1.519999999999993578, 0.000000000000000000, 0.000000000000000000 ) ) ;
#32578 = CARTESIAN_POINT ( 'NONE',  ( 70.00000000000001421, 87.62632027716348659, 34.45236684482946288 ) ) ;
#32579 = ORIENTED_EDGE ( 'NONE', *, *, #26466, .T. ) ;
#32580 = CARTESIAN_POINT ( 'NONE',  ( -35.99181955245763476, -114.9929510916434339, 13.11847460610632687 ) ) ;
#32581 = EDGE_LOOP ( 'NONE', ( #34760, #17780, #8589, #33314 ) ) ;
#32582 = CARTESIAN_POINT ( 'NONE',  ( -36.23083527818512550, -116.0245472910329880, 4.784774454178448266 ) ) ;
#32583 = CIRCLE ( 'NONE', #29156, 4.000000000000000000 ) ;
#32584 = DIRECTION ( 'NONE',  ( -1.000000000000000000, 0.000000000000000000, 0.000000000000000000 ) ) ;
#32585 = AXIS2_PLACEMENT_3D ( 'NONE', #21681, #16089, #2280 ) ;
#32586 = VERTEX_POINT ( 'NONE', #27446 ) ;
#32587 = ORIENTED_EDGE ( 'NONE', *, *, #27527, .F. ) ;
#32588 = ADVANCED_FACE ( 'NONE', ( #10694 ), #22018, .T. ) ;
#32589 = CARTESIAN_POINT ( 'NONE',  ( 50.00005079999999680, 5.400000000000021672, 1.000000000000001776 ) ) ;
#32590 = DIRECTION ( 'NONE',  ( 1.000000000000000000, -0.000000000000000000, 0.000000000000000000 ) ) ;
#32591 = ADVANCED_FACE ( 'NONE', ( #33848, #64 ), #10879, .T. ) ;
#32592 = EDGE_CURVE ( 'NONE', #10721, #35401, #21658, .T. ) ;
#32593 = VERTEX_POINT ( 'NONE', #18967 ) ;
#32594 = CARTESIAN_POINT ( 'NONE',  ( -35.69809690994938478, -111.0245472910330022, 5.722274454178450043 ) ) ;
#32595 = AXIS2_PLACEMENT_3D ( 'NONE', #7153, #2138, #26788 ) ;
#32596 = DIRECTION ( 'NONE',  ( 1.000000000000000000, -4.336808689941997226E-15, -1.084202172485499306E-15 ) ) ;
#32597 = CIRCLE ( 'NONE', #2172, 20.00000000000000711 ) ;
#32598 = CARTESIAN_POINT ( 'NONE',  ( 4.000000000000000000, 4.627536653468036720E-16, 55.00000000000000000 ) ) ;
#32599 = EDGE_LOOP ( 'NONE', ( #10005, #10436 ) ) ;
#32600 = ORIENTED_EDGE ( 'NONE', *, *, #13092, .F. ) ;
#32601 = CARTESIAN_POINT ( 'NONE',  ( -1.599999999999989653, -4.588090364676975566E-14, 7.020000000000020890 ) ) ;
#32602 = ADVANCED_FACE ( 'NONE', ( #712 ), #6124, .T. ) ;
#32603 = VECTOR ( 'NONE', #22210, 1000.000000000000000 ) ;
#32604 = EDGE_CURVE ( 'NONE', #26363, #33969, #17171, .T. ) ;
#32605 = DIRECTION ( 'NONE',  ( -1.000000000000000000, 0.000000000000000000, 0.000000000000000000 ) ) ;
#32606 = ORIENTED_EDGE ( 'NONE', *, *, #24381, .T. ) ;
#32607 = ORIENTED_EDGE ( 'NONE', *, *, #15402, .T. ) ;
#32608 = CARTESIAN_POINT ( 'NONE',  ( -34.50000000000000000, -111.0140978167138570, -0.5622823525984297355 ) ) ;
#32609 = VECTOR ( 'NONE', #19804, 1000.000000000000000 ) ;
#32610 = AXIS2_PLACEMENT_3D ( 'NONE', #2326, #10943, #35091 ) ;
#32611 = CIRCLE ( 'NONE', #398, 7.199999999999993072 ) ;
#32612 = DIRECTION ( 'NONE',  ( 0.000000000000000000, 0.000000000000000000, 1.000000000000000000 ) ) ;
#32613 = ORIENTED_EDGE ( 'NONE', *, *, #33275, .T. ) ;
#32614 = CARTESIAN_POINT ( 'NONE',  ( -35.50000000000000711, -114.9929510916434339, 10.52000928670414126 ) ) ;
#32615 = CARTESIAN_POINT ( 'NONE',  ( -34.50000000000000000, -113.9929510916434339, 12.53051367006571581 ) ) ;
#32616 = CARTESIAN_POINT ( 'NONE',  ( -90.00000000000002842, 0.000000000000000000, 6.938893903907228378E-15 ) ) ;
#32617 = DIRECTION ( 'NONE',  ( -1.000000000000000000, 0.000000000000000000, 0.000000000000000000 ) ) ;
#32618 = CARTESIAN_POINT ( 'NONE',  ( -37.52044295795950291, -113.9929510916434339, 13.11812344617477422 ) ) ;
#32619 = ADVANCED_FACE ( 'NONE', ( #894 ), #11874, .T. ) ;
#32620 = CARTESIAN_POINT ( 'NONE',  ( -36.03906250000000000, -115.9929510916434481, 13.11852480586264846 ) ) ;
#32621 = AXIS2_PLACEMENT_3D ( 'NONE', #33952, #11794, #17366 ) ;
#32622 = CARTESIAN_POINT ( 'NONE',  ( 7.999999999999992895, 0.000000000000000000, 0.000000000000000000 ) ) ;
#32623 = CYLINDRICAL_SURFACE ( 'NONE', #19806, 47.49900000000001654 ) ;
#32624 = AXIS2_PLACEMENT_3D ( 'NONE', #11103, #24961, #18656 ) ;
#32625 = EDGE_CURVE ( 'NONE', #32655, #34510, #34030, .T. ) ;
#32626 = VERTEX_POINT ( 'NONE', #20846 ) ;
#32627 = EDGE_CURVE ( 'NONE', #26146, #33746, #21802, .T. ) ;
#32628 = CARTESIAN_POINT ( 'NONE',  ( 0.000000000000000000, 45.78515115856044559, 12.64416602183680816 ) ) ;
#32629 = LINE ( 'NONE', #21452, #18553 ) ;
#32630 = DIRECTION ( 'NONE',  ( -1.000000000000000000, 0.000000000000000000, 0.000000000000000000 ) ) ;
#32631 = CIRCLE ( 'NONE', #26892, 0.04100000000000673939 ) ;
#32632 = VECTOR ( 'NONE', #3680, 1000.000000000000000 ) ;
#32633 = ORIENTED_EDGE ( 'NONE', *, *, #32798, .F. ) ;
#32634 = CIRCLE ( 'NONE', #997, 4.200000000000014388 ) ;
#32635 = DIRECTION ( 'NONE',  ( 0.000000000000000000, 0.000000000000000000, 1.000000000000000000 ) ) ;
#32636 = EDGE_LOOP ( 'NONE', ( #1623, #12756, #27434, #25444 ) ) ;
#32637 = CARTESIAN_POINT ( 'NONE',  ( -35.50000000000000711, -116.0140896356112989, -0.6575071456984549201 ) ) ;
#32638 = DIRECTION ( 'NONE',  ( -1.000000000000000000, 0.000000000000000000, 0.000000000000000000 ) ) ;
#32639 = EDGE_CURVE ( 'NONE', #9389, #29599, #20631, .T. ) ;
#32640 = EDGE_CURVE ( 'NONE', #32501, #20175, #17800, .T. ) ;
#32641 = AXIS2_PLACEMENT_3D ( 'NONE', #27478, #16460, #10375 ) ;
#32642 = CARTESIAN_POINT ( 'NONE',  ( -35.50000000000000711, -114.9929510916434339, 12.17846912687782712 ) ) ;
#32643 = LINE ( 'NONE', #23829, #3859 ) ;
#32644 = ORIENTED_EDGE ( 'NONE', *, *, #31984, .F. ) ;
#32645 = CARTESIAN_POINT ( 'NONE',  ( -44.00000000000000000, 4.000000000000000000, 0.000000000000000000 ) ) ;
#32646 = CARTESIAN_POINT ( 'NONE',  ( -35.50000000000000000, -112.5389594332240222, 2.818899826424027477 ) ) ;
#32647 = VERTEX_POINT ( 'NONE', #20313 ) ;
#32648 = ORIENTED_EDGE ( 'NONE', *, *, #12544, .T. ) ;
#32649 = CARTESIAN_POINT ( 'NONE',  ( -37.35495115944176092, -112.9754527089670688, 7.034774454178450043 ) ) ;
#32650 =( LENGTH_UNIT ( ) NAMED_UNIT ( * ) SI_UNIT ( .MILLI., .METRE. ) );
#32651 = EDGE_CURVE ( 'NONE', #10949, #22703, #26425, .T. ) ;
#32652 = CIRCLE ( 'NONE', #30367, 20.00000000000000711 ) ;
#32653 = CARTESIAN_POINT ( 'NONE',  ( 1.600000000000004086, -12.74999999999999822, -1.200000000000006617 ) ) ;
#32654 = ORIENTED_EDGE ( 'NONE', *, *, #23357, .F. ) ;
#32655 = VERTEX_POINT ( 'NONE', #9535 ) ;
#32656 = CARTESIAN_POINT ( 'NONE',  ( -34.50000000000000000, -113.0140978167138712, 0.3752176474015639918 ) ) ;
#32657 = DIRECTION ( 'NONE',  ( -1.000000000000000000, 0.000000000000000000, 0.000000000000000000 ) ) ;
#32658 = VECTOR ( 'NONE', #25765, 1000.000000000000000 ) ;
#32659 = AXIS2_PLACEMENT_3D ( 'NONE', #29177, #4527, #15456 ) ;
#32660 = PLANE ( 'NONE',  #34447 ) ;
#32661 = EDGE_CURVE ( 'NONE', #23024, #14077, #12240, .T. ) ;
#32662 = AXIS2_PLACEMENT_3D ( 'NONE', #14380, #25386, #700 ) ;
#32663 = CARTESIAN_POINT ( 'NONE',  ( 7.999999999999992895, -46.11014828289837197, -9.022736828081189486 ) ) ;
#32664 = VECTOR ( 'NONE', #19043, 1000.000000000000000 ) ;
#32665 = CARTESIAN_POINT ( 'NONE',  ( -35.50000000000000000, -113.9000545103886850, 10.49516883415891577 ) ) ;
#32666 = DIRECTION ( 'NONE',  ( 0.000000000000000000, 0.8090169943749448977, 0.5877852522924766898 ) ) ;
#32667 = CARTESIAN_POINT ( 'NONE',  ( 0.000000000000000000, 0.000000000000000000, 0.000000000000000000 ) ) ;
#32668 = VECTOR ( 'NONE', #9157, 1000.000000000000000 ) ;
#32669 = CARTESIAN_POINT ( 'NONE',  ( -34.50000000000000000, -112.6919296022648638, -1.573728109100751116 ) ) ;
#32670 = EDGE_CURVE ( 'NONE', #14164, #6382, #25864, .T. ) ;
#32671 = CARTESIAN_POINT ( 'NONE',  ( -36.12500000000014211, -115.9929510916434481, 14.11852480586265024 ) ) ;
#32672 = DIRECTION ( 'NONE',  ( 1.000000000000000000, 0.000000000000000000, 0.000000000000000000 ) ) ;
#32673 = ADVANCED_FACE ( 'NONE', ( #31322 ), #17624, .T. ) ;
#32674 = DIRECTION ( 'NONE',  ( 0.000000000000000000, 0.000000000000000000, 1.000000000000000000 ) ) ;
#32675 = ORIENTED_EDGE ( 'NONE', *, *, #35542, .F. ) ;
#32676 = CARTESIAN_POINT ( 'NONE',  ( -35.50000000000000711, -114.1021862393805577, 9.512197583835053649 ) ) ;
#32677 = CARTESIAN_POINT ( 'NONE',  ( -34.49999999999998579, -27.48076211353304998, 71.08058909292485339 ) ) ;
#32678 = CARTESIAN_POINT ( 'NONE',  ( 4.000000000000000000, 4.627536653468036720E-16, 45.89999999999999858 ) ) ;
#32679 = DIRECTION ( 'NONE',  ( -1.000000000000000000, 6.056754644426116516E-31, -1.734723475976807094E-16 ) ) ;
#32680 = VERTEX_POINT ( 'NONE', #20499 ) ;
#32681 = FACE_OUTER_BOUND ( 'NONE', #20481, .T. ) ;
#32682 = CARTESIAN_POINT ( 'NONE',  ( 0.000000000000000000, 0.000000000000000000, 0.000000000000000000 ) ) ;
#32683 = CARTESIAN_POINT ( 'NONE',  ( 7.999999999999992895, -37.91532898920942074, 28.61088654061626357 ) ) ;
#32684 = CARTESIAN_POINT ( 'NONE',  ( -44.00000000000000000, 0.000000000000000000, 0.000000000000000000 ) ) ;
#32685 = ADVANCED_FACE ( 'NONE', ( #23029 ), #9882, .T. ) ;
#32686 = AXIS2_PLACEMENT_3D ( 'NONE', #26225, #7134, #28751 ) ;
#32687 = CARTESIAN_POINT ( 'NONE',  ( 8.000000000000000000, 0.000000000000000000, 0.000000000000000000 ) ) ;
#32688 = DIRECTION ( 'NONE',  ( 0.000000000000000000, 0.000000000000000000, 1.000000000000000000 ) ) ;
#32689 = ORIENTED_EDGE ( 'NONE', *, *, #7913, .F. ) ;
#32690 = VERTEX_POINT ( 'NONE', #23397 ) ;
#32691 = AXIS2_PLACEMENT_3D ( 'NONE', #943, #11400, #33009 ) ;
#32692 = CARTESIAN_POINT ( 'NONE',  ( 0.000000000000000000, -2.912696353505664248, -21.80633394113455736 ) ) ;
#32693 = CARTESIAN_POINT ( 'NONE',  ( -3.413765605486555721, -14.29811891091961584, -1.200000000000006617 ) ) ;
#32694 = CARTESIAN_POINT ( 'NONE',  ( -50.00000000000000000, 6.123233995736780087E-16, 5.000000000000011546 ) ) ;
#32695 = ORIENTED_EDGE ( 'NONE', *, *, #11943, .F. ) ;
#32696 = CARTESIAN_POINT ( 'NONE',  ( -38.99999999999999289, -114.0592624029313242, 4.746475545821550845 ) ) ;
#32697 = VERTEX_POINT ( 'NONE', #26105 ) ;
#32698 = VECTOR ( 'NONE', #3553, 1000.000000000000000 ) ;
#32699 = ORIENTED_EDGE ( 'NONE', *, *, #21736, .T. ) ;
#32700 = ORIENTED_EDGE ( 'NONE', *, *, #10815, .F. ) ;
#32701 = PLANE ( 'NONE',  #25803 ) ;
#32702 = CARTESIAN_POINT ( 'NONE',  ( -30.00000000000000000, 45.00000000000000000, 5.510910596163089556E-15 ) ) ;
#32703 = VERTEX_POINT ( 'NONE', #18162 ) ;
#32704 = VERTEX_POINT ( 'NONE', #28632 ) ;
#32705 = CARTESIAN_POINT ( 'NONE',  ( 8.000000000000000000, 0.000000000000000000, 0.000000000000000000 ) ) ;
#32706 = FACE_OUTER_BOUND ( 'NONE', #16554, .T. ) ;
#32707 = DIRECTION ( 'NONE',  ( -1.836970198721029934E-16, 1.000000000000000000, 0.000000000000000000 ) ) ;
#32708 = CARTESIAN_POINT ( 'NONE',  ( 70.00000000000001421, -31.33892132276156062, 83.40622150580404082 ) ) ;
#32709 = DIRECTION ( 'NONE',  ( -1.000000000000000000, 0.000000000000000000, 0.000000000000000000 ) ) ;
#32710 = CIRCLE ( 'NONE', #7980, 7.999999999999992895 ) ;
#32711 = EDGE_CURVE ( 'NONE', #13216, #26461, #6880, .T. ) ;
#32712 = FACE_BOUND ( 'NONE', #32599, .T. ) ;
#32713 = CARTESIAN_POINT ( 'NONE',  ( -37.98325232167028531, -115.9929510916434481, 14.04194344061727584 ) ) ;
#32714 = DIRECTION ( 'NONE',  ( 1.000000000000000000, -0.000000000000000000, -0.000000000000000000 ) ) ;
#32715 = DIRECTION ( 'NONE',  ( -1.000000000000000000, 0.000000000000000000, 0.000000000000000000 ) ) ;
#32716 = CARTESIAN_POINT ( 'NONE',  ( 0.000000000000000000, -9.637487275700962641, -10.15474465512060398 ) ) ;
#32717 = CARTESIAN_POINT ( 'NONE',  ( -39.49999999999999289, -11.24969279549607748, 111.5585998451919778 ) ) ;
#32718 = DIRECTION ( 'NONE',  ( 0.000000000000000000, 0.8660254037844333785, 0.5000000000000092149 ) ) ;
#32719 = CARTESIAN_POINT ( 'NONE',  ( -39.49999999999999289, -5.633167542791597704, 121.0048025873810218 ) ) ;
#32720 = VERTEX_POINT ( 'NONE', #28980 ) ;
#32721 = CARTESIAN_POINT ( 'NONE',  ( -38.99999999999999289, -114.0592624029313242, 4.746475545821550845 ) ) ;
#32722 = CARTESIAN_POINT ( 'NONE',  ( 7.999999999999992895, 20.99948489194422763, 42.60488980472790388 ) ) ;
#32723 = DIRECTION ( 'NONE',  ( -1.000000000000000000, 0.000000000000000000, 0.000000000000000000 ) ) ;
#32724 = DIRECTION ( 'NONE',  ( -1.000000000000000000, -0.000000000000000000, -0.000000000000000000 ) ) ;
#32725 = ORIENTED_EDGE ( 'NONE', *, *, #34140, .F. ) ;
#32726 = ORIENTED_EDGE ( 'NONE', *, *, #2731, .F. ) ;
#32727 = CARTESIAN_POINT ( 'NONE',  ( 7.999999999999992895, 0.2227391519123156360, -46.98410307550729215 ) ) ;
#32728 = ORIENTED_EDGE ( 'NONE', *, *, #3535, .F. ) ;
#32729 = AXIS2_PLACEMENT_3D ( 'NONE', #3361, #630, #5865 ) ;
#32730 = ORIENTED_EDGE ( 'NONE', *, *, #34096, .T. ) ;
#32731 = AXIS2_PLACEMENT_3D ( 'NONE', #9934, #28679, #14969 ) ;
#32732 = CARTESIAN_POINT ( 'NONE',  ( 55.00000000000000000, -25.98076211353320275, 78.99999999999992895 ) ) ;
#32733 = CARTESIAN_POINT ( 'NONE',  ( 7.999999999999992895, -18.53613841426757602, -48.58406706613921244 ) ) ;
#32734 = CIRCLE ( 'NONE', #10903, 20.00000000000000355 ) ;
#32735 = AXIS2_PLACEMENT_3D ( 'NONE', #7986, #22852, #9174 ) ;
#32736 =( LENGTH_UNIT ( ) NAMED_UNIT ( * ) SI_UNIT ( .MILLI., .METRE. ) );
#32737 = DIRECTION ( 'NONE',  ( -1.000000000000000000, 0.000000000000000000, 0.000000000000000000 ) ) ;
#32738 = VERTEX_POINT ( 'NONE', #23754 ) ;
#32739 = VERTEX_POINT ( 'NONE', #3790 ) ;
#32740 = CARTESIAN_POINT ( 'NONE',  ( 50.00000000000000000, -25.98076211353320275, 84.99999999999992895 ) ) ;
#32741 = DIRECTION ( 'NONE',  ( -1.000000000000000000, -0.000000000000000000, 0.000000000000000000 ) ) ;
#32742 = ORIENTED_EDGE ( 'NONE', *, *, #32768, .T. ) ;
#32743 = CARTESIAN_POINT ( 'NONE',  ( -9.999999999999994671, 0.000000000000000000, 0.000000000000000000 ) ) ;
#32744 = CARTESIAN_POINT ( 'NONE',  ( -34.50000000000000000, -116.0140978167138712, -0.4685323525984310677 ) ) ;
#32745 = EDGE_CURVE ( 'NONE', #10703, #10849, #34396, .T. ) ;
#32746 = CARTESIAN_POINT ( 'NONE',  ( -37.46093750000000711, -114.9929510916434339, 14.11852480586264846 ) ) ;
#32747 = EDGE_CURVE ( 'NONE', #33531, #1331, #25929, .T. ) ;
#32748 = DIRECTION ( 'NONE',  ( 1.226634733346697831E-16, 0.7071067811865466846, 0.7071067811865483499 ) ) ;
#32749 = CARTESIAN_POINT ( 'NONE',  ( -35.50000000000000000, -113.9929510916434339, 10.50625754673586876 ) ) ;
#32750 = DIRECTION ( 'NONE',  ( -0.000000000000000000, 0.000000000000000000, -1.000000000000000000 ) ) ;
#32751 = CARTESIAN_POINT ( 'NONE',  ( -34.50000000000000000, -114.9929510916434339, 10.94631322572069365 ) ) ;
#32752 = DIRECTION ( 'NONE',  ( 0.000000000000000000, 0.000000000000000000, 1.000000000000000000 ) ) ;
#32753 = DIRECTION ( 'NONE',  ( 0.000000000000000000, 0.8660254037844333785, 0.5000000000000092149 ) ) ;
#32754 = CARTESIAN_POINT ( 'NONE',  ( -50.00000000000000000, 0.000000000000000000, 8.000000000000000000 ) ) ;
#32755 = DIRECTION ( 'NONE',  ( 0.000000000000000000, 0.000000000000000000, -1.000000000000000000 ) ) ;
#32756 = AXIS2_PLACEMENT_3D ( 'NONE', #29877, #32394, #2349 ) ;
#32757 = CARTESIAN_POINT ( 'NONE',  ( -44.00000000000000000, 11.00000000000000000, 1.347111479062088405E-15 ) ) ;
#32758 = DIRECTION ( 'NONE',  ( -1.000000000000000000, 0.000000000000000000, 0.000000000000000000 ) ) ;
#32759 = ORIENTED_EDGE ( 'NONE', *, *, #25639, .F. ) ;
#32760 = FACE_OUTER_BOUND ( 'NONE', #20521, .T. ) ;
#32761 = VERTEX_POINT ( 'NONE', #31668 ) ;
#32762 = EDGE_CURVE ( 'NONE', #5490, #20834, #7003, .T. ) ;
#32763 = CIRCLE ( 'NONE', #2890, 20.00000000000001066 ) ;
#32764 = PRODUCT_DEFINITION_FORMATION_WITH_SPECIFIED_SOURCE ( 'ANY', '', #34550, .NOT_KNOWN. ) ;
#32765 = CARTESIAN_POINT ( 'NONE',  ( -34.00000000000000000, -114.0592624029313242, 1.503524454178448710 ) ) ;
#32766 = CARTESIAN_POINT ( 'NONE',  ( 4.000000000000003553, -25.61928775981074935, 45.25098998563470332 ) ) ;
#32767 = ORIENTED_EDGE ( 'NONE', *, *, #18491, .F. ) ;
#32768 = EDGE_CURVE ( 'NONE', #29296, #35453, #1622, .T. ) ;
#32769 = ORIENTED_EDGE ( 'NONE', *, *, #12221, .T. ) ;
#32770 = CARTESIAN_POINT ( 'NONE',  ( 0.000000000000000000, 6.860320204751148232, 13.89802171851385459 ) ) ;
#32771 = DIRECTION ( 'NONE',  ( 0.000000000000000000, -0.9822872507286903865, 0.1873813145857150808 ) ) ;
#32772 = ORIENTED_EDGE ( 'NONE', *, *, #25971, .F. ) ;
#32773 = CARTESIAN_POINT ( 'NONE',  ( -38.18337828418795965, -110.9754527089670546, 7.034774454178450043 ) ) ;
#32774 = LINE ( 'NONE', #30080, #19555 ) ;
#32775 = DIRECTION ( 'NONE',  ( 1.000000000000000000, -5.339440136655842133E-16, -1.047965281155519420E-16 ) ) ;
#32776 = ORIENTED_EDGE ( 'NONE', *, *, #18568, .F. ) ;
#32777 = ORIENTED_EDGE ( 'NONE', *, *, #8553, .F. ) ;
#32778 = DIRECTION ( 'NONE',  ( -1.000000000000000000, 0.000000000000000000, 0.000000000000000000 ) ) ;
#32779 = CIRCLE ( 'NONE', #22994, 17.49900000000000944 ) ;
#32780 = EDGE_CURVE ( 'NONE', #19260, #34014, #15451, .T. ) ;
#32781 = SURFACE_STYLE_USAGE ( .BOTH. , #21786 ) ;
#32782 = DIRECTION ( 'NONE',  ( 0.000000000000000000, 0.000000000000000000, 1.000000000000000000 ) ) ;
#32783 = VERTEX_POINT ( 'NONE', #34743 ) ;
#32784 = ORIENTED_EDGE ( 'NONE', *, *, #14324, .T. ) ;
#32785 = CIRCLE ( 'NONE', #9777, 22.00000000000000000 ) ;
#32786 = CARTESIAN_POINT ( 'NONE',  ( -34.50000000000000000, -111.0140978167138570, 0.8127176474015720409 ) ) ;
#32787 = DIRECTION ( 'NONE',  ( -1.000000000000000000, 0.000000000000000000, 0.000000000000000000 ) ) ;
#32788 = AXIS2_PLACEMENT_3D ( 'NONE', #7474, #20606, #31606 ) ;
#32789 = CIRCLE ( 'NONE', #17243, 20.00000000000000355 ) ;
#32790 = ORIENTED_EDGE ( 'NONE', *, *, #28887, .F. ) ;
#32791 = AXIS2_PLACEMENT_3D ( 'NONE', #23249, #20348, #31359 ) ;
#32792 = CARTESIAN_POINT ( 'NONE',  ( -35.50000000000000711, -114.0998638248492085, 9.511920366020609308 ) ) ;
#32793 = ADVANCED_FACE ( 'NONE', ( #1084 ), #12055, .F. ) ;
#32794 = CARTESIAN_POINT ( 'NONE',  ( -36.15625000000007816, -113.9929510916434339, 14.11852480586265024 ) ) ;
#32795 = EDGE_CURVE ( 'NONE', #29599, #31713, #25311, .T. ) ;
#32796 = LINE ( 'NONE', #8289, #21770 ) ;
#32797 = CARTESIAN_POINT ( 'NONE',  ( 8.000000000000000000, -16.31134495048487310, 6.336799421339755156 ) ) ;
#32798 = EDGE_CURVE ( 'NONE', #8708, #16103, #9184, .T. ) ;
#32799 = CARTESIAN_POINT ( 'NONE',  ( -34.51922597003733273, -113.9929510916434339, 12.86289566494349224 ) ) ;
#32800 = FACE_OUTER_BOUND ( 'NONE', #12583, .T. ) ;
#32801 = CARTESIAN_POINT ( 'NONE',  ( -35.50000000000000711, -114.9929510916434339, 10.55026311463432087 ) ) ;
#32802 = LINE ( 'NONE', #15862, #19870 ) ;
#32803 = CARTESIAN_POINT ( 'NONE',  ( 4.000000000000003553, -3.268936481846215880, 13.61301047812921183 ) ) ;
#32804 = VERTEX_POINT ( 'NONE', #27001 ) ;
#32805 = ADVANCED_FACE ( 'NONE', ( #21394 ), #24122, .T. ) ;
#32806 = CYLINDRICAL_SURFACE ( 'NONE', #20659, 19.99999999999998579 ) ;
#32807 = DIRECTION ( 'NONE',  ( -1.000000000000000000, 0.000000000000000000, 0.000000000000000000 ) ) ;
#32808 = DIRECTION ( 'NONE',  ( -1.000000000000000000, 1.110223024625156540E-16, 0.000000000000000000 ) ) ;
#32809 = ADVANCED_FACE ( 'NONE', ( #18345 ), #18877, .T. ) ;
#32810 = ORIENTED_EDGE ( 'NONE', *, *, #20733, .F. ) ;
#32811 = AXIS2_PLACEMENT_3D ( 'NONE', #9852, #1590, #26249 ) ;
#32812 = CARTESIAN_POINT ( 'NONE',  ( 0.000000000000000000, 38.92705108641771261, -27.21837053747755419 ) ) ;
#32813 = ORIENTED_EDGE ( 'NONE', *, *, #8238, .F. ) ;
#32814 = CARTESIAN_POINT ( 'NONE',  ( -35.50000000000000000, -113.9344536409997630, 0.9850770315317123327 ) ) ;
#32815 = CYLINDRICAL_SURFACE ( 'NONE', #3521, 7.199999999999993072 ) ;
#32816 = CARTESIAN_POINT ( 'NONE',  ( -37.74901162816869515, -114.6652019342044042, 3.566024454178448710 ) ) ;
#32817 = AXIS2_PLACEMENT_3D ( 'NONE', #10322, #10134, #7250 ) ;
#32818 = AXIS2_PLACEMENT_3D ( 'NONE', #35325, #10645, #16021 ) ;
#32819 = CARTESIAN_POINT ( 'NONE',  ( -35.49999931242378892, -114.9929510916434339, 12.61439929482945566 ) ) ;
#32820 = CYLINDRICAL_SURFACE ( 'NONE', #26287, 13.99999999999999822 ) ;
#32821 = EDGE_LOOP ( 'NONE', ( #15320, #28125, #12642, #25475 ) ) ;
#32822 = DIRECTION ( 'NONE',  ( 1.000000000000000000, -0.000000000000000000, -0.000000000000000000 ) ) ;
#32823 = CARTESIAN_POINT ( 'NONE',  ( -35.50000000000000000, -112.4803765279500993, 2.803636946313094569 ) ) ;
#32824 = ORIENTED_EDGE ( 'NONE', *, *, #24701, .F. ) ;
#32825 = ORIENTED_EDGE ( 'NONE', *, *, #22830, .F. ) ;
#32826 = CARTESIAN_POINT ( 'NONE',  ( -37.88768952767750164, -115.9754527089670262, 3.472274454178448266 ) ) ;
#32827 = ADVANCED_FACE ( 'NONE', ( #29875 ), #29346, .F. ) ;
#32828 = CARTESIAN_POINT ( 'NONE',  ( 0.000000000000000000, 0.000000000000000000, -49.10000000000000142 ) ) ;
#32829 = EDGE_LOOP ( 'NONE', ( #7049, #13373, #14333, #22984 ) ) ;
#32830 = ORIENTED_EDGE ( 'NONE', *, *, #22224, .F. ) ;
#32831 = CARTESIAN_POINT ( 'NONE',  ( -34.50000000000000000, -115.0140978167138428, -0.6247823525986679893 ) ) ;
#32832 = DIRECTION ( 'NONE',  ( 1.084202172485497408E-16, -6.938893903907204958E-17, -1.000000000000000000 ) ) ;
#32833 = CIRCLE ( 'NONE', #2932, 5.000000000000011546 ) ;
#32834 = CARTESIAN_POINT ( 'NONE',  ( 4.000000000000003553, 40.47821179127763003, -32.64221760512714354 ) ) ;
#32835 = DIRECTION ( 'NONE',  ( -1.000000000000000000, 0.000000000000000000, 0.000000000000000000 ) ) ;
#32836 = CARTESIAN_POINT ( 'NONE',  ( -35.50000000000000000, -113.9929510916434339, 10.51725893871049067 ) ) ;
#32837 = CARTESIAN_POINT ( 'NONE',  ( 8.000000000000000000, 1.693188892523745936, 15.40623615209872632 ) ) ;
#32838 = EDGE_CURVE ( 'NONE', #29619, #13072, #20683, .T. ) ;
#32839 = CARTESIAN_POINT ( 'NONE',  ( 7.999999999999992895, 38.92705108641732892, 27.21837053747812263 ) ) ;
#32840 = EDGE_CURVE ( 'NONE', #24139, #15081, #24729, .T. ) ;
#32841 = AXIS2_PLACEMENT_3D ( 'NONE', #34634, #7602, #29412 ) ;
#32842 =( GEOMETRIC_REPRESENTATION_CONTEXT ( 3 ) GLOBAL_UNCERTAINTY_ASSIGNED_CONTEXT ( ( #5716 ) ) GLOBAL_UNIT_ASSIGNED_CONTEXT ( ( #3302, #33525, #11564 ) ) REPRESENTATION_CONTEXT ( 'NONE', 'WORKASPACE' ) );
#32843 = VECTOR ( 'NONE', #30400, 1000.000000000000000 ) ;
#32844 = CARTESIAN_POINT ( 'NONE',  ( -34.50000000000000000, -115.3362660311619692, -1.573728109101206085 ) ) ;
#32845 = CARTESIAN_POINT ( 'NONE',  ( -35.50000000000000000, -114.2899554544714960, 8.528375582263644006 ) ) ;
#32846 = CARTESIAN_POINT ( 'NONE',  ( 7.999999999999992895, 46.11014828289842882, -9.022736828080857308 ) ) ;
#32847 = PRODUCT_DEFINITION_SHAPE ( 'NONE', 'NONE',  #35651 ) ;
#32848 = DIRECTION ( 'NONE',  ( 0.000000000000000000, 0.2486898871648553222, -0.9685831611286309650 ) ) ;
#32849 = ORIENTED_EDGE ( 'NONE', *, *, #30852, .F. ) ;
#32850 = CARTESIAN_POINT ( 'NONE',  ( -37.75185693410092824, -115.9929510916434481, 13.05539834812634759 ) ) ;
#32851 = DIRECTION ( 'NONE',  ( -1.000000000000000000, 0.000000000000000000, 0.000000000000000000 ) ) ;
#32852 = DIRECTION ( 'NONE',  ( 0.000000000000000000, -0.9659258262890686453, 0.2588190451025194072 ) ) ;
#32853 = CARTESIAN_POINT ( 'NONE',  ( -1.600000000000018074, 7.019999999999929408, -1.040834085586084257E-14 ) ) ;
#32854 = EDGE_CURVE ( 'NONE', #16713, #29785, #27349, .T. ) ;
#32855 = ORIENTED_EDGE ( 'NONE', *, *, #15388, .T. ) ;
#32856 = CARTESIAN_POINT ( 'NONE',  ( 0.000000000000000000, 16.92083251265324861, 4.460989585141029501 ) ) ;
#32857 = CARTESIAN_POINT ( 'NONE',  ( 0.000000000000000000, -9.433698091065020108, -1.111908866155191022 ) ) ;
#32858 = CARTESIAN_POINT ( 'NONE',  ( 0.000000000000000000, 0.9861715913087641949, 17.47118961583601759 ) ) ;
#32859 = DIRECTION ( 'NONE',  ( -1.000000000000000000, 0.000000000000000000, 0.000000000000000000 ) ) ;
#32860 = CIRCLE ( 'NONE', #27111, 7.199999999999993072 ) ;
#32861 = PLANE ( 'NONE',  #1482 ) ;
#32862 = FACE_OUTER_BOUND ( 'NONE', #4799, .T. ) ;
#32863 = ORIENTED_EDGE ( 'NONE', *, *, #20822, .T. ) ;
#32864 = ORIENTED_EDGE ( 'NONE', *, *, #12876, .T. ) ;
#32865 = DIRECTION ( 'NONE',  ( -1.000000000000000000, 0.000000000000000000, 0.000000000000000000 ) ) ;
#32866 = FACE_OUTER_BOUND ( 'NONE', #12252, .T. ) ;
#32867 = CARTESIAN_POINT ( 'NONE',  ( -10.00000000000000000, 0.000000000000000000, 0.000000000000000000 ) ) ;
#32868 = ORIENTED_EDGE ( 'NONE', *, *, #4850, .F. ) ;
#32869 = CARTESIAN_POINT ( 'NONE',  ( -37.88768952767750875, -112.0245472910329880, 9.527725545821557063 ) ) ;
#32870 = ORIENTED_EDGE ( 'NONE', *, *, #14047, .F. ) ;
#32871 = AXIS2_PLACEMENT_3D ( 'NONE', #20100, #28405, #3748 ) ;
#32872 = STYLED_ITEM ( 'NONE', ( #12992 ), #8640 ) ;
#32873 = EDGE_CURVE ( 'NONE', #24623, #9377, #10259, .T. ) ;
#32874 = ORIENTED_EDGE ( 'NONE', *, *, #16477, .F. ) ;
#32875 = ORIENTED_EDGE ( 'NONE', *, *, #3046, .F. ) ;
#32876 = DIRECTION ( 'NONE',  ( 0.000000000000000000, -0.3420201433256566115, -0.9396926207859127578 ) ) ;
#32877 = ADVANCED_FACE ( 'NONE', ( #30051 ), #4693, .F. ) ;
#32878 = EDGE_CURVE ( 'NONE', #33836, #27200, #27619, .T. ) ;
#32879 = DIRECTION ( 'NONE',  ( 0.000000000000000000, -0.3420201433256566115, -0.9396926207859127578 ) ) ;
#32880 = ORIENTED_EDGE ( 'NONE', *, *, #2972, .F. ) ;
#32881 = CARTESIAN_POINT ( 'NONE',  ( -35.50000000000000711, -114.9929510916434339, 10.51175824272318415 ) ) ;
#32882 = CARTESIAN_POINT ( 'NONE',  ( -10.50000000000000178, 1.285879139104719253E-15, -1.200000000000006617 ) ) ;
#32883 = EDGE_CURVE ( 'NONE', #15669, #7480, #9762, .T. ) ;
#32884 = CARTESIAN_POINT ( 'NONE',  ( 46.00000000000000000, 0.000000000000000000, 70.00000000000000000 ) ) ;
#32885 = ADVANCED_FACE ( 'NONE', ( #21562 ), #24295, .F. ) ;
#32886 = DIRECTION ( 'NONE',  ( -1.000000000000000000, 0.000000000000000000, 0.000000000000000000 ) ) ;
#32887 = LINE ( 'NONE', #30369, #30085 ) ;
#32888 = PLANE ( 'NONE',  #20882 ) ;
#32889 = AXIS2_PLACEMENT_3D ( 'NONE', #26331, #24514, #13531 ) ;
#32890 =( GEOMETRIC_REPRESENTATION_CONTEXT ( 3 ) GLOBAL_UNCERTAINTY_ASSIGNED_CONTEXT ( ( #12054 ) ) GLOBAL_UNIT_ASSIGNED_CONTEXT ( ( #13181, #30262, #12 ) ) REPRESENTATION_CONTEXT ( 'NONE', 'WORKASPACE' ) );
#32891 = CARTESIAN_POINT ( 'NONE',  ( -36.03125000000003553, -115.9929510916434481, 14.11852480586265024 ) ) ;
#32893 = CARTESIAN_POINT ( 'NONE',  ( 0.000000000000000000, -15.49408907645140943, -44.90087086784610904 ) ) ;
#32892 = VECTOR ( 'NONE', #3526, 1000.000000000000000 ) ;
#32894 = FACE_OUTER_BOUND ( 'NONE', #19683, .T. ) ;
#32895 = CARTESIAN_POINT ( 'NONE',  ( -3.799999999999999822, 0.000000000000000000, -39.50000000000000711 ) ) ;
#32896 = DIRECTION ( 'NONE',  ( 0.000000000000000000, 0.000000000000000000, -1.000000000000000000 ) ) ;
#32897 = CARTESIAN_POINT ( 'NONE',  ( -1.000000000000000888, -6.008326913195953800, -0.7999999999999951594 ) ) ;
#32898 = FACE_OUTER_BOUND ( 'NONE', #31656, .T. ) ;
#32899 = ORIENTED_EDGE ( 'NONE', *, *, #13905, .F. ) ;
#32900 = CARTESIAN_POINT ( 'NONE',  ( -38.37230871539094323, -115.4561184093552413, 7.558975545821551734 ) ) ;
#32901 = DIRECTION ( 'NONE',  ( -1.000000000000000000, 0.000000000000000000, 0.000000000000000000 ) ) ;
#32902 = DIRECTION ( 'NONE',  ( 1.000000000000000000, 0.000000000000000000, 0.000000000000000000 ) ) ;
#32903 = CARTESIAN_POINT ( 'NONE',  ( -4.000000000000000000, 0.000000000000000000, 65.00000000000000000 ) ) ;
#32904 = ORIENTED_EDGE ( 'NONE', *, *, #5652, .T. ) ;
#32905 = AXIS2_PLACEMENT_3D ( 'NONE', #1494, #23088, #20565 ) ;
#32906 = EDGE_LOOP ( 'NONE', ( #21208, #18260 ) ) ;
#32907 = DIRECTION ( 'NONE',  ( -1.000000000000000000, -1.502314598737170371E-16, 8.673617379883843187E-17 ) ) ;
#32908 = DIRECTION ( 'NONE',  ( 1.000000000000000000, 0.000000000000000000, 0.000000000000000000 ) ) ;
#32909 = ORIENTED_EDGE ( 'NONE', *, *, #22938, .T. ) ;
#32910 = ORIENTED_EDGE ( 'NONE', *, *, #8151, .F. ) ;
#32911 = EDGE_CURVE ( 'NONE', #33000, #3384, #24163, .T. ) ;
#32912 = EDGE_CURVE ( 'NONE', #13354, #30986, #29898, .T. ) ;
#32913 = CARTESIAN_POINT ( 'NONE',  ( 1.799999999999996048, 0.000000000000000000, 0.000000000000000000 ) ) ;
#32914 = AXIS2_PLACEMENT_3D ( 'NONE', #26524, #9229, #4029 ) ;
#32915 = DIRECTION ( 'NONE',  ( 0.000000000000000000, 0.000000000000000000, 1.000000000000000000 ) ) ;
#32916 = CIRCLE ( 'NONE', #21978, 17.49900000000000233 ) ;
#32917 = AXIS2_PLACEMENT_3D ( 'NONE', #15718, #34834, #35026 ) ;
#32918 = DIRECTION ( 'NONE',  ( 3.885678848705451963E-18, 0.9730768813850324550, 0.2304807647374924884 ) ) ;
#32919 = CARTESIAN_POINT ( 'NONE',  ( 8.000000000000007105, 0.000000000000000000, 0.000000000000000000 ) ) ;
#32920 = ORIENTED_EDGE ( 'NONE', *, *, #32661, .F. ) ;
#32921 = ORIENTED_EDGE ( 'NONE', *, *, #8226, .T. ) ;
#32922 = DIRECTION ( 'NONE',  ( 2.668805347656626185E-16, -1.000000000000000000, 0.000000000000000000 ) ) ;
#32923 = DIRECTION ( 'NONE',  ( 0.000000000000000000, 0.000000000000000000, 1.000000000000000000 ) ) ;
#32924 = ORIENTED_EDGE ( 'NONE', *, *, #31320, .F. ) ;
#32925 = DIRECTION ( 'NONE',  ( 0.000000000000000000, 0.000000000000000000, 1.000000000000000000 ) ) ;
#32926 = AXIS2_PLACEMENT_3D ( 'NONE', #19109, #30107, #5446 ) ;
#32927 = CARTESIAN_POINT ( 'NONE',  ( -34.50000000000000000, -112.3995503592287690, -1.424448457485529618 ) ) ;
#32928 = CARTESIAN_POINT ( 'NONE',  ( -36.62499999999902656, -114.9929510916434339, 14.11852480586264846 ) ) ;
#32929 = CARTESIAN_POINT ( 'NONE',  ( -35.50000000000000000, -113.9929510916435618, 10.50625754673588474 ) ) ;
#32930 = FACE_OUTER_BOUND ( 'NONE', #13831, .T. ) ;
#32931 = CARTESIAN_POINT ( 'NONE',  ( -34.50120407906360498, -114.9929510916434339, 12.67985367974112343 ) ) ;
#32932 = DIRECTION ( 'NONE',  ( 0.000000000000000000, 1.000000000000000000, 0.000000000000000000 ) ) ;
#32933 = FACE_OUTER_BOUND ( 'NONE', #18222, .T. ) ;
#32934 = SURFACE_STYLE_USAGE ( .BOTH. , #33775 ) ;
#32935 = DIRECTION ( 'NONE',  ( -1.000000000000000000, 0.000000000000000000, -0.000000000000000000 ) ) ;
#32936 = DIRECTION ( 'NONE',  ( 0.000000000000000000, 0.000000000000000000, -1.000000000000000000 ) ) ;
#32937 = CARTESIAN_POINT ( 'NONE',  ( -42.49999999999999289, -25.98076211353322051, 84.99999999999992895 ) ) ;
#32938 = VECTOR ( 'NONE', #24219, 1000.000000000000000 ) ;
#32939 = ORIENTED_EDGE ( 'NONE', *, *, #18922, .T. ) ;
#32940 = VECTOR ( 'NONE', #21229, 1000.000000000000000 ) ;
#32941 = LINE ( 'NONE', #8785, #13003 ) ;
#32942 = ORIENTED_EDGE ( 'NONE', *, *, #34621, .T. ) ;
#32943 = CARTESIAN_POINT ( 'NONE',  ( -39.97545270896702618, -112.6980969099493990, 3.847274454178448710 ) ) ;
#32944 = CARTESIAN_POINT ( 'NONE',  ( -50.00000000000000000, 19.99999999999998934, 120.0000000000000000 ) ) ;
#32945 = VERTEX_POINT ( 'NONE', #18523 ) ;
#32946 = ORIENTED_EDGE ( 'NONE', *, *, #18244, .F. ) ;
#32947 = DIRECTION ( 'NONE',  ( 0.000000000000000000, 0.000000000000000000, -1.000000000000000000 ) ) ;
#32948 = DIRECTION ( 'NONE',  ( -1.000000000000000000, 0.000000000000000000, 0.000000000000000000 ) ) ;
#32949 = ORIENTED_EDGE ( 'NONE', *, *, #31321, .T. ) ;
#32950 = CARTESIAN_POINT ( 'NONE',  ( -34.83677480945821259, -116.0794154965774965, 4.183975545821551734 ) ) ;
#32951 = AXIS2_PLACEMENT_3D ( 'NONE', #9773, #29407, #9412 ) ;
#32952 = CIRCLE ( 'NONE', #31228, 20.00000000000000711 ) ;
#32953 = DIRECTION ( 'NONE',  ( 0.000000000000000000, 0.000000000000000000, 1.000000000000000000 ) ) ;
#32954 = EDGE_CURVE ( 'NONE', #24482, #8147, #13799, .T. ) ;
#32955 = PLANE ( 'NONE',  #2741 ) ;
#32957 = ORIENTED_EDGE ( 'NONE', *, *, #3009, .T. ) ;
#32956 = AXIS2_PLACEMENT_3D ( 'NONE', #18546, #15649, #12800 ) ;
#32958 = ORIENTED_EDGE ( 'NONE', *, *, #1423, .T. ) ;
#32959 = VECTOR ( 'NONE', #9275, 1000.000000000000000 ) ;
#32960 = LINE ( 'NONE', #21961, #6742 ) ;
#32961 = SURFACE_STYLE_FILL_AREA ( #21962 ) ;
#32962 = LINE ( 'NONE', #538, #33397 ) ;
#32963 = EDGE_LOOP ( 'NONE', ( #12908, #11635, #1863, #32600 ) ) ;
#32964 = VERTEX_POINT ( 'NONE', #13146 ) ;
#32965 = CARTESIAN_POINT ( 'NONE',  ( -35.50000000000000000, -112.7319952733504635, 2.855726801009121463 ) ) ;
#32966 = VECTOR ( 'NONE', #4039, 1000.000000000000114 ) ;
#32967 = AXIS2_PLACEMENT_3D ( 'NONE', #30018, #30714, #10749 ) ;
#32968 = EDGE_CURVE ( 'NONE', #24250, #21944, #3449, .T. ) ;
#32969 = PLANE ( 'NONE',  #6994 ) ;
#32970 = CIRCLE ( 'NONE', #17420, 20.00000000000000355 ) ;
#32971 = ORIENTED_EDGE ( 'NONE', *, *, #10564, .F. ) ;
#32972 = CARTESIAN_POINT ( 'NONE',  ( -35.50000000000000711, -114.0185793162512908, 9.502217742515812304 ) ) ;
#32973 = CARTESIAN_POINT ( 'NONE',  ( -34.50000000000000000, -113.9929510916434339, 12.60752341388803721 ) ) ;
#32974 = DIRECTION ( 'NONE',  ( -1.000000000000000000, 0.000000000000000000, 0.000000000000000000 ) ) ;
#32975 = DIRECTION ( 'NONE',  ( 1.000000000000000000, 0.000000000000000000, 0.000000000000000000 ) ) ;
#32976 = CARTESIAN_POINT ( 'NONE',  ( -34.50000000000000000, -113.9929510916438460, 10.50625754673626133 ) ) ;
#32977 = CARTESIAN_POINT ( 'NONE',  ( -39.00000000000000711, -114.9929510916434339, 12.56351784598954779 ) ) ;
#32978 = CARTESIAN_POINT ( 'NONE',  ( -35.50000000000000711, -114.1021862393805577, 9.512197583835053649 ) ) ;
#32979 = PRESENTATION_STYLE_ASSIGNMENT (( #22158 ) ) ;
#32980 = VECTOR ( 'NONE', #27000, 1000.000000000000000 ) ;
#32981 = DIRECTION ( 'NONE',  ( 0.000000000000000000, 0.000000000000000000, 1.000000000000000000 ) ) ;
#32982 = VERTEX_POINT ( 'NONE', #30408 ) ;
#32983 = ORIENTED_EDGE ( 'NONE', *, *, #938, .T. ) ;
#32984 = DIRECTION ( 'NONE',  ( 1.000000000000000000, 0.000000000000000000, 0.000000000000000000 ) ) ;
#32985 = DIRECTION ( 'NONE',  ( 0.000000000000000000, 0.9510565162951523099, 0.3090169943749513926 ) ) ;
#32986 = VERTEX_POINT ( 'NONE', #19732 ) ;
#32987 = DIRECTION ( 'NONE',  ( 0.000000000000000000, 0.000000000000000000, -1.000000000000000000 ) ) ;
#32988 = ORIENTED_EDGE ( 'NONE', *, *, #29757, .F. ) ;
#32989 = AXIS2_PLACEMENT_3D ( 'NONE', #20522, #12258, #28464 ) ;
#32990 = AXIS2_PLACEMENT_3D ( 'NONE', #4249, #3534, #30889 ) ;
#32991 = CARTESIAN_POINT ( 'NONE',  ( -35.50000000000000000, -113.0140978167138712, 0.5627176474015715968 ) ) ;
#32992 = CARTESIAN_POINT ( 'NONE',  ( 0.000000000000000000, 24.47917365150010127, -45.87777302070911389 ) ) ;
#32993 = CARTESIAN_POINT ( 'NONE',  ( -38.02454729103296671, -114.3549511594417396, 2.159774454178448710 ) ) ;
#32994 = AXIS2_PLACEMENT_3D ( 'NONE', #25651, #4229, #983 ) ;
#32995 = DIRECTION ( 'NONE',  ( 0.000000000000000000, 0.000000000000000000, 1.000000000000000000 ) ) ;
#32996 = ORIENTED_EDGE ( 'NONE', *, *, #27166, .T. ) ;
#32997 = LINE ( 'NONE', #8311, #22214 ) ;
#32998 = ADVANCED_FACE ( 'NONE', ( #27704 ), #8764, .T. ) ;
#32999 = CARTESIAN_POINT ( 'NONE',  ( -35.50000000000000711, -113.1256619669233885, 1.895633585076891947 ) ) ;
#33000 = VERTEX_POINT ( 'NONE', #30223 ) ;
#33001 = ORIENTED_EDGE ( 'NONE', *, *, #31089, .F. ) ;
#33002 = EDGE_CURVE ( 'NONE', #29093, #17785, #24819, .T. ) ;
#33003 = CARTESIAN_POINT ( 'NONE',  ( -34.97545270896703329, -113.2308352781851539, 4.409774454178448266 ) ) ;
#33004 = DIRECTION ( 'NONE',  ( 0.000000000000000000, -1.000000000000000000, 0.000000000000000000 ) ) ;
#33006 = ORIENTED_EDGE ( 'NONE', *, *, #25567, .F. ) ;
#33005 = CIRCLE ( 'NONE', #22644, 22.00000000000000000 ) ;
#33007 = VERTEX_POINT ( 'NONE', #19405 ) ;
#33008 = CARTESIAN_POINT ( 'NONE',  ( -34.50000000000000000, -115.0140978167139707, -0.6247823525984387283 ) ) ;
#33009 = DIRECTION ( 'NONE',  ( 0.000000000000000000, 0.000000000000000000, 1.000000000000000000 ) ) ;
#33010 = EDGE_CURVE ( 'NONE', #7529, #2044, #34492, .T. ) ;
#33011 = DIRECTION ( 'NONE',  ( -1.734723475976807094E-16, 9.406921877466749789E-15, -1.000000000000000000 ) ) ;
#33012 = EDGE_CURVE ( 'NONE', #20345, #9, #3040, .T. ) ;
#33013 = DIRECTION ( 'NONE',  ( -1.000000000000000000, 0.000000000000000000, 0.000000000000000000 ) ) ;
#33014 = EDGE_CURVE ( 'NONE', #34614, #19983, #18392, .T. ) ;
#33015 = AXIS2_PLACEMENT_3D ( 'NONE', #30434, #695, #14207 ) ;
#33016 = CARTESIAN_POINT ( 'NONE',  ( -35.50000000000000000, -113.9929510916434339, 10.53376102667243508 ) ) ;
#33017 = VECTOR ( 'NONE', #12792, 1000.000000000000000 ) ;
#33018 = PLANE ( 'NONE',  #27085 ) ;
#33019 = CARTESIAN_POINT ( 'NONE',  ( 7.999999999999992895, 0.000000000000000000, 0.000000000000000000 ) ) ;
#33020 = CARTESIAN_POINT ( 'NONE',  ( -34.50000000000000000, -111.0140978167138570, 0.3752176474015639918 ) ) ;
#33021 = CARTESIAN_POINT ( 'NONE',  ( -37.88878409051687157, -115.9929510916434481, 14.07058620477052280 ) ) ;
#33022 = UNCERTAINTY_MEASURE_WITH_UNIT (LENGTH_MEASURE( 1.000000000000000082E-05 ), #22934, 'distance_accuracy_value', 'NONE');
#33023 = DIRECTION ( 'NONE',  ( 0.000000000000000000, 0.000000000000000000, 1.000000000000000000 ) ) ;
#33024 = DIRECTION ( 'NONE',  ( 0.000000000000000000, 0.000000000000000000, 1.000000000000000000 ) ) ;
#33025 = DIRECTION ( 'NONE',  ( 0.000000000000000000, 0.000000000000000000, -1.000000000000000000 ) ) ;
#33026 = EDGE_LOOP ( 'NONE', ( #20878, #18587, #830, #17572 ) ) ;
#33027 = CARTESIAN_POINT ( 'NONE',  ( -37.56526046546249376, -115.9929510916434481, 13.11451721564129258 ) ) ;
#33028 = CARTESIAN_POINT ( 'NONE',  ( -34.49999999999998579, -23.26666049839546702, 88.29903810567660116 ) ) ;
#33029 = PLANE ( 'NONE',  #1900 ) ;
#33030 = EDGE_CURVE ( 'NONE', #6171, #19728, #8036, .T. ) ;
#33031 = DIRECTION ( 'NONE',  ( -1.000000000000000000, -0.000000000000000000, -0.000000000000000000 ) ) ;
#33032 = ORIENTED_EDGE ( 'NONE', *, *, #32625, .F. ) ;
#33033 = CARTESIAN_POINT ( 'NONE',  ( -34.49999999999998579, -11.98076211353319742, 83.49999999999992895 ) ) ;
#33034 = DIRECTION ( 'NONE',  ( -1.000000000000000000, 0.000000000000000000, -0.000000000000000000 ) ) ;
#33035 = CARTESIAN_POINT ( 'NONE',  ( 7.999999999999992895, 0.000000000000000000, 0.000000000000000000 ) ) ;
#33036 = DIRECTION ( 'NONE',  ( -1.000000000000000000, -1.836970198721029934E-16, -0.000000000000000000 ) ) ;
#33037 = CONTEXT_DEPENDENT_SHAPE_REPRESENTATION ( #22992, #28487 ) ;
#33038 = FACE_BOUND ( 'NONE', #33290, .T. ) ;
#33039 = DIRECTION ( 'NONE',  ( -1.000000000000000000, 0.000000000000000000, 0.000000000000000000 ) ) ;
#33040 = ORIENTED_EDGE ( 'NONE', *, *, #21285, .F. ) ;
#33041 = DIRECTION ( 'NONE',  ( -0.000000000000000000, 0.000000000000000000, 1.000000000000000000 ) ) ;
#33042 = EDGE_CURVE ( 'NONE', #20385, #26642, #11648, .T. ) ;
#33043 = AXIS2_PLACEMENT_3D ( 'NONE', #34715, #1950, #21366 ) ;
#33044 = DIRECTION ( 'NONE',  ( 0.000000000000000000, 0.000000000000000000, 1.000000000000000000 ) ) ;
#33045 = DIRECTION ( 'NONE',  ( 0.000000000000000000, 0.000000000000000000, 1.000000000000000000 ) ) ;
#33046 = ORIENTED_EDGE ( 'NONE', *, *, #33902, .T. ) ;
#33047 = EDGE_CURVE ( 'NONE', #25950, #18471, #16694, .T. ) ;
#33048 = CARTESIAN_POINT ( 'NONE',  ( -36.23083527818512550, -111.9754527089670404, 9.715225545821551734 ) ) ;
#33049 = EDGE_CURVE ( 'NONE', #34547, #14078, #17216, .T. ) ;
#33050 = ORIENTED_EDGE ( 'NONE', *, *, #18972, .F. ) ;
#33051 = VECTOR ( 'NONE', #4880, 1000.000000000000000 ) ;
#33052 =( NAMED_UNIT ( * ) PLANE_ANGLE_UNIT ( ) SI_UNIT ( $, .RADIAN. ) );
#33053 = ORIENTED_EDGE ( 'NONE', *, *, #25760, .F. ) ;
#33054 = ORIENTED_EDGE ( 'NONE', *, *, #6183, .T. ) ;
#33055 = CYLINDRICAL_SURFACE ( 'NONE', #30397, 7.199999999999993960 ) ;
#33056 = EDGE_CURVE ( 'NONE', #10826, #33486, #27049, .T. ) ;
#33057 = EDGE_CURVE ( 'NONE', #25880, #25236, #11312, .T. ) ;
#33058 = DIRECTION ( 'NONE',  ( 0.000000000000000000, 0.3681245526846786964, -0.9297764858882511252 ) ) ;
#33059 = DIRECTION ( 'NONE',  ( 0.000000000000000000, 0.3420201433256692680, -0.9396926207859080948 ) ) ;
#33060 = CARTESIAN_POINT ( 'NONE',  ( 7.999999999999992895, -44.47301969247433817, -16.68249143361957820 ) ) ;
#33061 = CARTESIAN_POINT ( 'NONE',  ( 8.000000000000000000, -8.605879768205133118, -12.89022243466717299 ) ) ;
#33062 = DIRECTION ( 'NONE',  ( 0.000000000000000000, 0.000000000000000000, 1.000000000000000000 ) ) ;
#33063 = PLANE ( 'NONE',  #8752 ) ;
#33064 = VECTOR ( 'NONE', #25679, 1000.000000000000000 ) ;
#33065 = VECTOR ( 'NONE', #5006, 1000.000000000000000 ) ;
#33066 = CARTESIAN_POINT ( 'NONE',  ( 50.00000000000000000, 10.00000000000000888, -15.00000000000000178 ) ) ;
#33067 = CARTESIAN_POINT ( 'NONE',  ( -35.98977351030467986, -115.9929510916434481, 14.11852173794918563 ) ) ;
#33068 = FACE_OUTER_BOUND ( 'NONE', #12013, .T. ) ;
#33069 = ADVANCED_FACE ( 'NONE', ( #8595 ), #16525, .T. ) ;
#33070 = CIRCLE ( 'NONE', #2037, 12.99999999999999467 ) ;
#33071 = DIRECTION ( 'NONE',  ( -1.000000000000000000, 0.000000000000000000, 0.000000000000000000 ) ) ;
#33072 = CARTESIAN_POINT ( 'NONE',  ( 8.000000000000000000, 19.35373470438985422, 10.46102064772347795 ) ) ;
#33073 = CARTESIAN_POINT ( 'NONE',  ( 50.00000000000000711, -25.98076211353320275, 84.99999999999994316 ) ) ;
#33074 = VECTOR ( 'NONE', #35018, 1000.000000000000114 ) ;
#33075 = EDGE_CURVE ( 'NONE', #18320, #30963, #27536, .T. ) ;
#33076 = DIRECTION ( 'NONE',  ( 0.000000000000000000, 0.8660254037844379305, 0.5000000000000011102 ) ) ;
#33077 = DIRECTION ( 'NONE',  ( 1.000000000000000000, 0.000000000000000000, -0.000000000000000000 ) ) ;
#33078 = ORIENTED_EDGE ( 'NONE', *, *, #34139, .F. ) ;
#33079 = CARTESIAN_POINT ( 'NONE',  ( -35.54388159064475872, -115.3723087153909432, 8.683975545821551734 ) ) ;
#33080 = CARTESIAN_POINT ( 'NONE',  ( 0.000000000000000000, 0.000000000000000000, 0.000000000000000000 ) ) ;
#33081 = DIRECTION ( 'NONE',  ( 0.000000000000000000, 0.000000000000000000, -1.000000000000000000 ) ) ;
#33082 = DIRECTION ( 'NONE',  ( -1.000000000000000000, 0.000000000000000000, 0.000000000000000000 ) ) ;
#33083 = ORIENTED_EDGE ( 'NONE', *, *, #34467, .T. ) ;
#33084 = AXIS2_PLACEMENT_3D ( 'NONE', #28858, #17319, #20367 ) ;
#33085 = ORIENTED_EDGE ( 'NONE', *, *, #25604, .T. ) ;
#33086 = CARTESIAN_POINT ( 'NONE',  ( 0.000000000000000000, -15.92965478239607968, -15.17386234660401101 ) ) ;
#33087 = CARTESIAN_POINT ( 'NONE',  ( 0.000000000000000000, -16.59870953437682672, 10.45300502024378986 ) ) ;
#33088 = ORIENTED_EDGE ( 'NONE', *, *, #788, .T. ) ;
#33089 = ADVANCED_FACE ( 'NONE', ( #16866 ), #22105, .T. ) ;
#33090 = ORIENTED_EDGE ( 'NONE', *, *, #21, .F. ) ;
#33091 = ADVANCED_FACE ( 'NONE', ( #18997 ), #2636, .T. ) ;
#33092 = CARTESIAN_POINT ( 'NONE',  ( 7.999999999999992895, -22.43957647427129842, -41.27978878573651400 ) ) ;
#33093 = AXIS2_PLACEMENT_3D ( 'NONE', #4258, #15195, #25501 ) ;
#33094 = FACE_OUTER_BOUND ( 'NONE', #9414, .T. ) ;
#33095 =( NAMED_UNIT ( * ) SI_UNIT ( $, .STERADIAN. ) SOLID_ANGLE_UNIT ( ) );
#33096 = AXIS2_PLACEMENT_3D ( 'NONE', #13078, #23691, #4626 ) ;
#33097 = DIRECTION ( 'NONE',  ( -1.000000000000000000, 0.000000000000000000, 0.000000000000000000 ) ) ;
#33098 = ORIENTED_EDGE ( 'NONE', *, *, #23549, .T. ) ;
#33099 = EDGE_LOOP ( 'NONE', ( #23021, #4153, #11872, #19320 ) ) ;
#33100 = DIRECTION ( 'NONE',  ( 0.000000000000000000, 0.000000000000000000, -1.000000000000000000 ) ) ;
#33101 = CARTESIAN_POINT ( 'NONE',  ( -34.49999999999998579, -14.17619866229204106, 94.12476896299857287 ) ) ;
#33102 = ORIENTED_EDGE ( 'NONE', *, *, #13892, .T. ) ;
#33103 = DIRECTION ( 'NONE',  ( 0.000000000000000000, 0.000000000000000000, 1.000000000000000000 ) ) ;
#33104 = AXIS2_PLACEMENT_3D ( 'NONE', #15108, #3628, #9550 ) ;
#33105 = CARTESIAN_POINT ( 'NONE',  ( -34.50000000000000000, -114.9307644833806137, -1.624782352598427959 ) ) ;
#33106 = CARTESIAN_POINT ( 'NONE',  ( -36.06250000000002132, -114.9929510916434339, 14.11852480586264846 ) ) ;
#33107 = CARTESIAN_POINT ( 'NONE',  ( -38.00000000000000711, -114.9929510916434339, 10.85830208992306822 ) ) ;
#33108 = DIRECTION ( 'NONE',  ( 0.000000000000000000, 0.000000000000000000, -1.000000000000000000 ) ) ;
#33109 = CARTESIAN_POINT ( 'NONE',  ( -36.03906250000000000, -114.9929510916434339, 14.11852480586264846 ) ) ;
#33110 = CARTESIAN_POINT ( 'NONE',  ( 7.999999999999992895, -9.744342220503080298, -46.48873837489808380 ) ) ;
#33111 = ORIENTED_EDGE ( 'NONE', *, *, #15178, .F. ) ;
#33112 = EDGE_CURVE ( 'NONE', #12635, #1256, #18640, .T. ) ;
#33113 = DIRECTION ( 'NONE',  ( -1.000000000000000000, 0.000000000000000000, 0.000000000000000000 ) ) ;
#33114 = DIRECTION ( 'NONE',  ( 1.000000000000000000, -0.000000000000000000, 0.000000000000000000 ) ) ;
#33115 = PLANE ( 'NONE',  #15267 ) ;
#33116 = DIRECTION ( 'NONE',  ( -1.000000000000000000, 0.000000000000000000, 0.000000000000000000 ) ) ;
#33117 = EDGE_CURVE ( 'NONE', #1430, #22165, #31035, .T. ) ;
#33118 = AXIS2_PLACEMENT_3D ( 'NONE', #2281, #7641, #12707 ) ;
#33119 = VERTEX_POINT ( 'NONE', #32693 ) ;
#33120 = DIRECTION ( 'NONE',  ( 0.000000000000000000, 0.000000000000000000, 1.000000000000000000 ) ) ;
#33121 = ORIENTED_EDGE ( 'NONE', *, *, #31745, .F. ) ;
#33122 = CARTESIAN_POINT ( 'NONE',  ( -39.97545270896702618, -112.6980969099493990, 5.347274454178449155 ) ) ;
#33123 = DIRECTION ( 'NONE',  ( -1.000000000000000000, 0.000000000000000000, -0.000000000000000000 ) ) ;
#33124 = CIRCLE ( 'NONE', #35442, 9.499000000000004107 ) ;
#33125 = ORIENTED_EDGE ( 'NONE', *, *, #27762, .F. ) ;
#33126 = VERTEX_POINT ( 'NONE', #22050 ) ;
#33127 = AXIS2_PLACEMENT_3D ( 'NONE', #13984, #5883, #25507 ) ;
#33128 = LINE ( 'NONE', #30075, #24605 ) ;
#33129 = CYLINDRICAL_SURFACE ( 'NONE', #799, 3.799999999999999822 ) ;
#33130 = ORIENTED_EDGE ( 'NONE', *, *, #33806, .F. ) ;
#33131 = CIRCLE ( 'NONE', #34286, 3.799999999999999822 ) ;
#33132 = DIRECTION ( 'NONE',  ( 1.000000000000000000, -0.000000000000000000, -0.000000000000000000 ) ) ;
#33133 = CARTESIAN_POINT ( 'NONE',  ( -21.15833593587365513, -10.50833024919764469, 77.79903810567677169 ) ) ;
#33134 = ORIENTED_EDGE ( 'NONE', *, *, #7291, .T. ) ;
#33135 = ORIENTED_EDGE ( 'NONE', *, *, #28274, .F. ) ;
#33136 = DIRECTION ( 'NONE',  ( -1.000000000000000000, 0.000000000000000000, -0.000000000000000000 ) ) ;
#33137 = CARTESIAN_POINT ( 'NONE',  ( 0.000000000000000000, -3.268936481846215880, 13.61301047812921183 ) ) ;
#33138 = ORIENTED_EDGE ( 'NONE', *, *, #35283, .F. ) ;
#33139 = ORIENTED_EDGE ( 'NONE', *, *, #12517, .T. ) ;
#33140 = CARTESIAN_POINT ( 'NONE',  ( -35.50000000000000000, -113.0071371610607684, 2.888584676720006961 ) ) ;
#33141 = PRODUCT_DEFINITION_SHAPE ( 'NONE', 'NONE',  #35650 ) ;
#33142 = AXIS2_PLACEMENT_3D ( 'NONE', #21629, #32635, #25057 ) ;
#33143 = DIRECTION ( 'NONE',  ( -1.000000000000000000, 0.000000000000000000, 0.000000000000000000 ) ) ;
#33144 = ORIENTED_EDGE ( 'NONE', *, *, #30200, .T. ) ;
#33145 = CARTESIAN_POINT ( 'NONE',  ( -35.50000000000000711, -114.9929510916434339, 12.57451923796416082 ) ) ;
#33146 = CIRCLE ( 'NONE', #30823, 4.000000000000000000 ) ;
#33147 = VECTOR ( 'NONE', #15963, 1000.000000000000000 ) ;
#33148 = CARTESIAN_POINT ( 'NONE',  ( -34.50481333282507279, -113.9929510916434339, 12.74107470552716315 ) ) ;
#33149 = AXIS2_PLACEMENT_3D ( 'NONE', #28198, #11991, #31072 ) ;
#33150 = CYLINDRICAL_SURFACE ( 'NONE', #11375, 6.000000000000005329 ) ;
#33151 = CARTESIAN_POINT ( 'NONE',  ( 7.999999999999992895, -0.6505223195686569149, 51.99593080916758936 ) ) ;
#33152 = CARTESIAN_POINT ( 'NONE',  ( -34.50000000000000000, -113.9929510916434339, 10.51175824272318415 ) ) ;
#33153 = DIRECTION ( 'NONE',  ( 1.000000000000000000, 0.000000000000000000, 0.000000000000000000 ) ) ;
#33154 = CARTESIAN_POINT ( 'NONE',  ( -35.50000000000000711, -114.1861579685891712, 9.524983039397698192 ) ) ;
#33155 = AXIS2_PLACEMENT_3D ( 'NONE', #13288, #18851, #27148 ) ;
#33156 = CARTESIAN_POINT ( 'NONE',  ( 7.999999999999992895, -51.19683565102439360, -9.104066087303991139 ) ) ;
#33157 = CARTESIAN_POINT ( 'NONE',  ( -39.49999999999999289, -14.67619866229204284, 94.12476896299857287 ) ) ;
#33158 = EDGE_CURVE ( 'NONE', #28443, #15919, #2891, .T. ) ;
#33159 = ORIENTED_EDGE ( 'NONE', *, *, #12975, .F. ) ;
#33160 = ORIENTED_EDGE ( 'NONE', *, *, #628, .T. ) ;
#33161 = DIRECTION ( 'NONE',  ( -1.000000000000000000, 0.000000000000000000, 0.000000000000000000 ) ) ;
#33162 = DIRECTION ( 'NONE',  ( -1.000000000000000000, 0.000000000000000000, 0.000000000000000000 ) ) ;
#33163 = VECTOR ( 'NONE', #8080, 1000.000000000000000 ) ;
#33164 = ORIENTED_EDGE ( 'NONE', *, *, #17483, .F. ) ;
#33165 = DIRECTION ( 'NONE',  ( 0.000000000000000000, 0.8660254037844362651, 0.5000000000000042188 ) ) ;
#33166 = VERTEX_POINT ( 'NONE', #27292 ) ;
#33167 = VECTOR ( 'NONE', #8575, 1000.000000000000114 ) ;
#33168 = CARTESIAN_POINT ( 'NONE',  ( -35.50000000000000000, -113.0140978167140702, 0.8752176474015694874 ) ) ;
#33169 = CARTESIAN_POINT ( 'NONE',  ( 0.000000000000000000, 0.000000000000000000, -25.00000000000000000 ) ) ;
#33170 = CARTESIAN_POINT ( 'NONE',  ( -38.45611840935523418, -115.3723087153909432, 3.566024454178448710 ) ) ;
#33171 = EDGE_CURVE ( 'NONE', #21169, #30069, #33352, .T. ) ;
#33172 = DIRECTION ( 'NONE',  ( 0.000000000000000000, 0.7705132427757904745, -0.6374239897486881912 ) ) ;
#33173 = AXIS2_PLACEMENT_3D ( 'NONE', #14320, #31076, #22595 ) ;
#33174 = VERTEX_POINT ( 'NONE', #21873 ) ;
#33175 = VECTOR ( 'NONE', #10677, 1000.000000000000000 ) ;
#33176 = FILL_AREA_STYLE ('',( #571 ) ) ;
#33177 = CARTESIAN_POINT ( 'NONE',  ( -35.50000000000000711, -112.1859307030124739, 1.448610958621386224 ) ) ;
#33178 = ORIENTED_EDGE ( 'NONE', *, *, #8871, .T. ) ;
#33179 = ORIENTED_EDGE ( 'NONE', *, *, #35297, .F. ) ;
#33180 = AXIS2_PLACEMENT_3D ( 'NONE', #7870, #32194, #18859 ) ;
#33181 = CARTESIAN_POINT ( 'NONE',  ( -36.11231047232249125, -112.0245472910329880, 8.722274454178448266 ) ) ;
#33182 = VECTOR ( 'NONE', #10533, 1000.000000000000000 ) ;
#33183 = CARTESIAN_POINT ( 'NONE',  ( 7.999999999999992895, -44.61570720899084819, -14.73072383765613935 ) ) ;
#33184 = ORIENTED_EDGE ( 'NONE', *, *, #32220, .F. ) ;
#33185 = ORIENTED_EDGE ( 'NONE', *, *, #34804, .F. ) ;
#33186 = CARTESIAN_POINT ( 'NONE',  ( -34.50000000000000000, -115.0140978167138712, -0.1247823525984438492 ) ) ;
#33187 = CARTESIAN_POINT ( 'NONE',  ( 7.999999999999992895, -20.99948489194452250, 42.60488980472776177 ) ) ;
#33188 = DIRECTION ( 'NONE',  ( 1.000000000000000000, 0.000000000000000000, 0.000000000000000000 ) ) ;
#33189 = VECTOR ( 'NONE', #27639, 1000.000000000000000 ) ;
#33190 = CIRCLE ( 'NONE', #24562, 47.49900000000000944 ) ;
#33191 = CARTESIAN_POINT ( 'NONE',  ( -35.50000000000000000, -113.9929510916434623, 10.50436693183592141 ) ) ;
#33192 = CYLINDRICAL_SURFACE ( 'NONE', #28794, 7.020000000000045759 ) ;
#33193 = CYLINDRICAL_SURFACE ( 'NONE', #13662, 52.00000000000000711 ) ;
#33194 = CARTESIAN_POINT ( 'NONE',  ( -34.50000000000000000, -115.8137639216009234, -1.239329810084483841 ) ) ;
#33195 = VECTOR ( 'NONE', #26237, 1000.000000000000000 ) ;
#33196 = CIRCLE ( 'NONE', #4485, 11.00000000000001066 ) ;
#33197 = CARTESIAN_POINT ( 'NONE',  ( -37.49023442168701337, -115.9929510916434481, 14.11852773550420359 ) ) ;
#33198 = CARTESIAN_POINT ( 'NONE',  ( 4.000000000000000000, 4.898587196589412829E-16, 55.00000000000000000 ) ) ;
#33199 = CIRCLE ( 'NONE', #23431, 52.00000000000000711 ) ;
#33200 = DIRECTION ( 'NONE',  ( -1.000000000000000000, 0.000000000000000000, -0.000000000000000000 ) ) ;
#33201 = ADVANCED_FACE ( 'NONE', ( #21693 ), #2290, .T. ) ;
#33202 = ADVANCED_FACE ( 'NONE', ( #15931 ), #13429, .T. ) ;
#33203 = AXIS2_PLACEMENT_3D ( 'NONE', #35263, #32724, #21537 ) ;
#33204 = ORIENTED_EDGE ( 'NONE', *, *, #3176, .F. ) ;
#33205 = DIRECTION ( 'NONE',  ( 0.000000000000000000, -1.000000000000000000, 0.000000000000000000 ) ) ;
#33206 = CARTESIAN_POINT ( 'NONE',  ( 0.000000000000000000, -49.25004636492401033, 16.68630974939741662 ) ) ;
#33207 = VECTOR ( 'NONE', #24495, 999.9999999999998863 ) ;
#33208 = CARTESIAN_POINT ( 'NONE',  ( 0.000000000000000000, 5.482169781018835231, 16.00140663693125376 ) ) ;
#33209 = VERTEX_POINT ( 'NONE', #7652 ) ;
#33210 = DIRECTION ( 'NONE',  ( -1.000000000000000000, 0.000000000000000000, 0.000000000000000000 ) ) ;
#33211 = CARTESIAN_POINT ( 'NONE',  ( 0.000000000000000000, 0.000000000000000000, 0.000000000000000000 ) ) ;
#33212 = CARTESIAN_POINT ( 'NONE',  ( -10.50000000000000178, 1.285879139104719253E-15, -8.088905766426390583E-30 ) ) ;
#33213 = DIRECTION ( 'NONE',  ( 0.000000000000000000, 0.5735764363510502672, -0.8191520442889889120 ) ) ;
#33214 = EDGE_CURVE ( 'NONE', #11602, #26795, #21704, .T. ) ;
#33215 = DIRECTION ( 'NONE',  ( 0.000000000000000000, 0.000000000000000000, 1.000000000000000000 ) ) ;
#33216 = CYLINDRICAL_SURFACE ( 'NONE', #17601, 19.99999999999998579 ) ;
#33217 = CIRCLE ( 'NONE', #2199, 52.00000000000000711 ) ;
#33218 = ORIENTED_EDGE ( 'NONE', *, *, #597, .F. ) ;
#33219 = CARTESIAN_POINT ( 'NONE',  ( -34.49999999999998579, -14.67619866229204284, 94.12476896299857287 ) ) ;
#33220 = AXIS2_PLACEMENT_3D ( 'NONE', #8210, #3007, #5353 ) ;
#33221 = CARTESIAN_POINT ( 'NONE',  ( 50.00000000000000711, 0.000000000000000000, 70.00000000000000000 ) ) ;
#33222 = CARTESIAN_POINT ( 'NONE',  ( 7.999999999999992895, 29.60891106212840285, -37.14118181634734839 ) ) ;
#33223 = VERTEX_POINT ( 'NONE', #10724 ) ;
#33224 = CARTESIAN_POINT ( 'NONE',  ( -36.52652403469559061, -114.9754527089670262, 2.777725545821551734 ) ) ;
#33225 = ORIENTED_EDGE ( 'NONE', *, *, #28415, .F. ) ;
#33226 = AXIS2_PLACEMENT_3D ( 'NONE', #2837, #22241, #3006 ) ;
#33227 = AXIS2_PLACEMENT_3D ( 'NONE', #8979, #8801, #13699 ) ;
#33228 = ORIENTED_EDGE ( 'NONE', *, *, #24082, .T. ) ;
#33229 = ORIENTED_EDGE ( 'NONE', *, *, #14525, .F. ) ;
#33230 = DIRECTION ( 'NONE',  ( 1.000000000000000000, -0.000000000000000000, 0.000000000000000000 ) ) ;
#33231 = VECTOR ( 'NONE', #17783, 1000.000000000000000 ) ;
#33232 = DIRECTION ( 'NONE',  ( -1.000000000000000000, 0.000000000000000000, 0.000000000000000000 ) ) ;
#33233 = EDGE_CURVE ( 'NONE', #22962, #23663, #7905, .T. ) ;
#33234 = CARTESIAN_POINT ( 'NONE',  ( -50.00000000000000000, 0.000000000000000000, 11.00000000000000000 ) ) ;
#33235 = CARTESIAN_POINT ( 'NONE',  ( -35.50000000000000711, -114.1489256397697289, 9.518467544735724317 ) ) ;
#33236 = DIRECTION ( 'NONE',  ( -1.000000000000000000, 0.000000000000000000, 0.000000000000000000 ) ) ;
#33237 = LINE ( 'NONE', #33404, #5096 ) ;
#33238 = CARTESIAN_POINT ( 'NONE',  ( -34.50000000000000000, -114.0000000000003411, 9.500000000000035527 ) ) ;
#33239 = CARTESIAN_POINT ( 'NONE',  ( -34.49999999999998579, -38.78532556477446036, 90.66066734786069503 ) ) ;
#33240 = ADVANCED_FACE ( 'NONE', ( #32866 ), #2824, .T. ) ;
#33241 = ADVANCED_FACE ( 'NONE', ( #32499 ), #5504, .T. ) ;
#33242 = DIRECTION ( 'NONE',  ( 0.000000000000000000, -0.8443279255020201823, 0.5358267949789886631 ) ) ;
#33243 = EDGE_CURVE ( 'NONE', #2456, #1876, #16100, .T. ) ;
#33244 = CARTESIAN_POINT ( 'NONE',  ( -36.00976557831293690, -115.9929510916434481, 14.11852773550420359 ) ) ;
#33245 = CYLINDRICAL_SURFACE ( 'NONE', #6734, 11.00000000000000000 ) ;
#33246 = AXIS2_PLACEMENT_3D ( 'NONE', #13968, #30014, #28014 ) ;
#33247 = CARTESIAN_POINT ( 'NONE',  ( 0.000000000000000000, 11.11653975335807587, -12.74840161668719851 ) ) ;
#33248 = CIRCLE ( 'NONE', #19440, 52.00000000000000711 ) ;
#33249 = DIRECTION ( 'NONE',  ( 0.000000000000000000, 0.000000000000000000, -1.000000000000000000 ) ) ;
#33250 = DIRECTION ( 'NONE',  ( 0.000000000000000000, 0.000000000000000000, -1.000000000000000000 ) ) ;
#33251 = CARTESIAN_POINT ( 'NONE',  ( 0.000000000000000000, 32.00046193115196758, -34.40241257139653186 ) ) ;
#33252 = CARTESIAN_POINT ( 'NONE',  ( -4.000000000000000000, 0.000000000000000000, -39.50000000000000711 ) ) ;
#33253 = ORIENTED_EDGE ( 'NONE', *, *, #25097, .T. ) ;
#33254 = ADVANCED_FACE ( 'NONE', ( #2458 ), #29995, .T. ) ;
#33255 = CARTESIAN_POINT ( 'NONE',  ( -35.00000000000000000, -113.9407375970686900, 9.996475545821549957 ) ) ;
#33256 = CARTESIAN_POINT ( 'NONE',  ( 1.600000000000004086, -12.74999999999999822, 0.000000000000000000 ) ) ;
#33257 = LINE ( 'NONE', #298, #33167 ) ;
#33258 = CARTESIAN_POINT ( 'NONE',  ( 0.000000000000000000, -14.48509162075955281, -8.733917826871511636 ) ) ;
#33259 = ADVANCED_FACE ( 'NONE', ( #26764 ), #13783, .T. ) ;
#33260 = EDGE_LOOP ( 'NONE', ( #24991, #27476, #15088, #32824 ) ) ;
#33261 = ORIENTED_EDGE ( 'NONE', *, *, #16487, .T. ) ;
#33262 = LINE ( 'NONE', #8579, #26292 ) ;
#33263 = CARTESIAN_POINT ( 'NONE',  ( 4.000000000000003553, 19.35373470438985777, 10.46102064772347795 ) ) ;
#33264 = VERTEX_POINT ( 'NONE', #13085 ) ;
#33265 = VERTEX_POINT ( 'NONE', #6202 ) ;
#33266 = CARTESIAN_POINT ( 'NONE',  ( -29.99999999999999645, -26.99999999999999645, 113.9999999999999858 ) ) ;
#33267 = DIRECTION ( 'NONE',  ( 0.000000000000000000, 0.000000000000000000, 1.000000000000000000 ) ) ;
#33268 = CIRCLE ( 'NONE', #5676, 15.49899999999998457 ) ;
#33269 = DIRECTION ( 'NONE',  ( 0.9999999999999998890, -5.499590109476241981E-19, -1.453711963017409949E-17 ) ) ;
#33270 = EDGE_CURVE ( 'NONE', #334, #17706, #13676, .T. ) ;
#33271 = DIRECTION ( 'NONE',  ( 0.000000000000000000, 0.000000000000000000, 1.000000000000000000 ) ) ;
#33272 = ORIENTED_EDGE ( 'NONE', *, *, #13714, .T. ) ;
#33273 = ORIENTED_EDGE ( 'NONE', *, *, #35324, .F. ) ;
#33274 = TOROIDAL_SURFACE ( 'NONE', #11427, 7.800000000000023803, 0.2000000000000003164 ) ;
#33275 = EDGE_CURVE ( 'NONE', #25710, #2681, #18832, .T. ) ;
#33276 = DIRECTION ( 'NONE',  ( 0.000000000000000000, -0.5877852522924621459, -0.8090169943749553338 ) ) ;
#33277 = DIRECTION ( 'NONE',  ( 0.000000000000000000, 0.000000000000000000, -1.000000000000000000 ) ) ;
#33278 = EDGE_CURVE ( 'NONE', #14164, #29056, #28170, .T. ) ;
#33279 = EDGE_LOOP ( 'NONE', ( #7082, #820, #33950, #19772 ) ) ;
#33280 = FACE_OUTER_BOUND ( 'NONE', #22055, .T. ) ;
#33281 = CARTESIAN_POINT ( 'NONE',  ( -34.50000000000000000, -112.0140978167138712, -0.3122823525984337878 ) ) ;
#33282 = CARTESIAN_POINT ( 'NONE',  ( -37.24999999999992895, -114.9929510916434339, 14.11852480586264846 ) ) ;
#33283 = EDGE_CURVE ( 'NONE', #32626, #27376, #1598, .T. ) ;
#33284 = CARTESIAN_POINT ( 'NONE',  ( -35.50000000000000000, -113.9929510916434339, 10.51725893871049067 ) ) ;
#33285 = CARTESIAN_POINT ( 'NONE',  ( 0.000000000000000000, -1.000000000000001554, 30.00000000000000000 ) ) ;
#33286 = EDGE_CURVE ( 'NONE', #33174, #26283, #19679, .T. ) ;
#33287 = CARTESIAN_POINT ( 'NONE',  ( -36.31249999999995026, -114.9929510916434339, 14.11852480586264846 ) ) ;
#33288 = CARTESIAN_POINT ( 'NONE',  ( 8.000000000000000000, -16.94522934049218676, 8.128228055638807348 ) ) ;
#33289 = DIRECTION ( 'NONE',  ( -1.000000000000000000, 0.000000000000000000, 0.000000000000000000 ) ) ;
#33290 = EDGE_LOOP ( 'NONE', ( #12557, #14163 ) ) ;
#33291 = DIRECTION ( 'NONE',  ( -1.000000000000000000, -0.000000000000000000, 0.000000000000000000 ) ) ;
#33292 = CARTESIAN_POINT ( 'NONE',  ( 70.00000000000001421, 49.63000703270403591, 62.56502393413636298 ) ) ;
#33293 = ORIENTED_EDGE ( 'NONE', *, *, #23294, .F. ) ;
#33294 = DIRECTION ( 'NONE',  ( -1.000000000000000000, 0.000000000000000000, 0.000000000000000000 ) ) ;
#33295 = ORIENTED_EDGE ( 'NONE', *, *, #32838, .F. ) ;
#33296 = CARTESIAN_POINT ( 'NONE',  ( -37.05926240293133134, -116.9999999999999858, 3.378524454178448710 ) ) ;
#33297 = CARTESIAN_POINT ( 'NONE',  ( 2.000000000000001776, 0.000000000000000000, 0.000000000000000000 ) ) ;
#33298 = CARTESIAN_POINT ( 'NONE',  ( -35.50000000000000711, -113.0557643173828524, -1.624792769101735868 ) ) ;
#33299 = ADVANCED_FACE ( 'NONE', ( #30696 ), #25293, .T. ) ;
#33300 = EDGE_LOOP ( 'NONE', ( #31084, #2556 ) ) ;
#33301 = AXIS2_PLACEMENT_3D ( 'NONE', #29609, #15895, #20006 ) ;
#33302 = ORIENTED_EDGE ( 'NONE', *, *, #32883, .T. ) ;
#33303 = CYLINDRICAL_SURFACE ( 'NONE', #20566, 52.00000000000000711 ) ;
#33304 = CARTESIAN_POINT ( 'NONE',  ( 0.000000000000000000, 5.400000000000000355, 0.000000000000000000 ) ) ;
#33305 = ORIENTED_EDGE ( 'NONE', *, *, #11800, .F. ) ;
#33306 = CARTESIAN_POINT ( 'NONE',  ( 4.000000000000003553, -19.74581912682808493, -48.10512059033414545 ) ) ;
#33307 = CARTESIAN_POINT ( 'NONE',  ( 0.000000000000000000, -31.08872492059928305, -41.68322423723133596 ) ) ;
#33308 = ORIENTED_EDGE ( 'NONE', *, *, #28326, .T. ) ;
#33309 = VERTEX_POINT ( 'NONE', #19853 ) ;
#33310 = DIRECTION ( 'NONE',  ( 0.000000000000000000, 0.1253332335643046469, -0.9921147013144777649 ) ) ;
#33311 = EDGE_CURVE ( 'NONE', #33746, #17384, #27823, .T. ) ;
#33312 = CARTESIAN_POINT ( 'NONE',  ( 50.00000000000000000, 0.000000000000000000, -11.00000000000000000 ) ) ;
#33313 = VERTEX_POINT ( 'NONE', #13951 ) ;
#33314 = ORIENTED_EDGE ( 'NONE', *, *, #16239, .T. ) ;
#33315 = CARTESIAN_POINT ( 'NONE',  ( -35.50000000000000000, -112.6572589393539516, 2.844055607295835397 ) ) ;
#33316 = ADVANCED_FACE ( 'NONE', ( #613 ), #25113, .T. ) ;
#33317 = EDGE_CURVE ( 'NONE', #15169, #31693, #10799, .T. ) ;
#33318 = EDGE_LOOP ( 'NONE', ( #2993, #22889 ) ) ;
#33319 = CARTESIAN_POINT ( 'NONE',  ( -35.50000000000000711, -114.9929510916434339, 12.59652202191340642 ) ) ;
#33320 = AXIS2_PLACEMENT_3D ( 'NONE', #12603, #23576, #34571 ) ;
#33321 = CARTESIAN_POINT ( 'NONE',  ( -34.50000000000000000, -113.9929510916434339, 11.21034663311132107 ) ) ;
#33322 = FACE_OUTER_BOUND ( 'NONE', #28000, .T. ) ;
#33323 = EDGE_CURVE ( 'NONE', #31368, #31306, #10234, .T. ) ;
#33324 = CARTESIAN_POINT ( 'NONE',  ( 0.000000000000000000, -44.75336757549767697, -14.30704879393654494 ) ) ;
#33325 = CIRCLE ( 'NONE', #13221, 3.799999999999999822 ) ;
#33326 = EDGE_CURVE ( 'NONE', #16219, #24282, #11947, .T. ) ;
#33327 = CARTESIAN_POINT ( 'NONE',  ( -34.50000000000000000, -113.9929510916434339, 12.59652202191340464 ) ) ;
#33328 = CARTESIAN_POINT ( 'NONE',  ( -38.69949915733018742, -114.9929510916434339, 13.54034599209165712 ) ) ;
#33329 = CARTESIAN_POINT ( 'NONE',  ( -35.50000000000000711, -114.9929510916434339, 11.21034663311131929 ) ) ;
#33330 = DIRECTION ( 'NONE',  ( 1.000000000000000000, -0.000000000000000000, 0.000000000000000000 ) ) ;
#33331 = DIRECTION ( 'NONE',  ( -1.000000000000000000, 0.000000000000000000, 0.000000000000000000 ) ) ;
#33332 = ORIENTED_EDGE ( 'NONE', *, *, #25979, .T. ) ;
#33333 = ORIENTED_EDGE ( 'NONE', *, *, #6815, .F. ) ;
#33334 = DIRECTION ( 'NONE',  ( -1.000000000000000000, 0.000000000000000000, 0.000000000000000000 ) ) ;
#33335 = CYLINDRICAL_SURFACE ( 'NONE', #19146, 52.00000000000000711 ) ;
#33336 = VERTEX_POINT ( 'NONE', #6025 ) ;
#33337 = DIRECTION ( 'NONE',  ( -1.000000000000000000, 0.000000000000000000, 0.000000000000000000 ) ) ;
#33338 = EDGE_LOOP ( 'NONE', ( #25574, #34090, #30745, #19393 ) ) ;
#33339 = CARTESIAN_POINT ( 'NONE',  ( -35.50000000000000000, -115.0140978167138712, -0.6247823525985405357 ) ) ;
#33340 = LINE ( 'NONE', #8664, #9266 ) ;
#33341 = CARTESIAN_POINT ( 'NONE',  ( -37.76916472181487450, -111.9754527089670404, 5.534774454178449155 ) ) ;
#33342 = CIRCLE ( 'NONE', #17799, 17.49900000000001654 ) ;
#33343 = DIRECTION ( 'NONE',  ( -1.000000000000000000, -1.734723475976807094E-16, 0.000000000000000000 ) ) ;
#33344 = VERTEX_POINT ( 'NONE', #16985 ) ;
#33345 = CIRCLE ( 'NONE', #31057, 0.7500000000000039968 ) ;
#33346 = CARTESIAN_POINT ( 'NONE',  ( 4.000000000000003553, -7.162210897275381072, -51.50439529848838305 ) ) ;
#33347 = CARTESIAN_POINT ( 'NONE',  ( -35.50000000000000711, -112.0140978167138712, 0.7502176474015694874 ) ) ;
#33348 = ORIENTED_EDGE ( 'NONE', *, *, #27347, .T. ) ;
#33349 = ORIENTED_EDGE ( 'NONE', *, *, #21020, .T. ) ;
#33350 = CARTESIAN_POINT ( 'NONE',  ( -38.45611840935523418, -115.3723087153909432, 8.066024454178448266 ) ) ;
#33351 = ORIENTED_EDGE ( 'NONE', *, *, #10929, .F. ) ;
#33352 = CIRCLE ( 'NONE', #11505, 52.00000000000000711 ) ;
#33353 = DIRECTION ( 'NONE',  ( 0.000000000000000000, 0.000000000000000000, 1.000000000000000000 ) ) ;
#33354 = ORIENTED_EDGE ( 'NONE', *, *, #1659, .F. ) ;
#33355 = ORIENTED_EDGE ( 'NONE', *, *, #17819, .T. ) ;
#33356 = CARTESIAN_POINT ( 'NONE',  ( -34.50000000000000000, -112.0140978167138712, 0.7502176474015694874 ) ) ;
#33357 = DIRECTION ( 'NONE',  ( 0.000000000000000000, 0.000000000000000000, -1.000000000000000000 ) ) ;
#33358 = ADVANCED_FACE ( 'NONE', ( #17337 ), #33744, .T. ) ;
#33359 = ORIENTED_EDGE ( 'NONE', *, *, #22086, .F. ) ;
#33360 = CARTESIAN_POINT ( 'NONE',  ( 7.999999999999992895, 24.72041153920734047, 40.55929306992698002 ) ) ;
#33361 =( REPRESENTATION_RELATIONSHIP ('NONE','NONE', #26607, #31430 ) REPRESENTATION_RELATIONSHIP_WITH_TRANSFORMATION ( #27472 )SHAPE_REPRESENTATION_RELATIONSHIP( ) );
#33362 = CARTESIAN_POINT ( 'NONE',  ( -35.50005019975638021, -113.9929510916434339, 12.62670525340498351 ) ) ;
#33363 = DIRECTION ( 'NONE',  ( 0.000000000000000000, 0.000000000000000000, -1.000000000000000000 ) ) ;
#33364 = AXIS2_PLACEMENT_3D ( 'NONE', #3886, #15183, #34119 ) ;
#33365 = DIRECTION ( 'NONE',  ( 1.000000000000000000, -0.000000000000000000, 0.000000000000000000 ) ) ;
#33366 = CARTESIAN_POINT ( 'NONE',  ( -34.50000000000000000, -116.0140978167138712, -0.1247823525984439463 ) ) ;
#33367 = CARTESIAN_POINT ( 'NONE',  ( -39.00000000000000000, -115.9929510916434481, 10.50625754673587053 ) ) ;
#33368 = CARTESIAN_POINT ( 'NONE',  ( 8.000000000000000000, 13.24207120356965461, 14.98824707027445768 ) ) ;
#33369 = AXIS2_PLACEMENT_3D ( 'NONE', #26075, #1406, #22467 ) ;
#33370 = DIRECTION ( 'NONE',  ( 0.000000000000000000, 0.000000000000000000, 1.000000000000000000 ) ) ;
#33371 = VERTEX_POINT ( 'NONE', #33560 ) ;
#33372 = VECTOR ( 'NONE', #25283, 1000.000000000000000 ) ;
#33373 = PLANE ( 'NONE',  #439 ) ;
#33374 = CARTESIAN_POINT ( 'NONE',  ( -29.99999999999999645, -26.99999999999999645, 113.9999999999999858 ) ) ;
#33375 = DIRECTION ( 'NONE',  ( 0.000000000000000000, 0.000000000000000000, 1.000000000000000000 ) ) ;
#33376 = ORIENTED_EDGE ( 'NONE', *, *, #29564, .T. ) ;
#33377 = DIRECTION ( 'NONE',  ( -1.000000000000000000, 0.000000000000000000, 0.000000000000000000 ) ) ;
#33378 = FACE_OUTER_BOUND ( 'NONE', #23065, .T. ) ;
#33379 = FACE_OUTER_BOUND ( 'NONE', #15788, .T. ) ;
#33380 = LINE ( 'NONE', #8705, #25343 ) ;
#33381 = CARTESIAN_POINT ( 'NONE',  ( -21.15833593587365513, -39.95319397786859383, 75.20096189432314304 ) ) ;
#33382 = CARTESIAN_POINT ( 'NONE',  ( -44.00000000000000000, -10.99999999999999289, 0.000000000000000000 ) ) ;
#33383 = VERTEX_POINT ( 'NONE', #30518 ) ;
#33384 = DIRECTION ( 'NONE',  ( -1.000000000000000000, 0.000000000000000000, -0.000000000000000000 ) ) ;
#33385 = CARTESIAN_POINT ( 'NONE',  ( -9.999999999999994671, 0.000000000000000000, 0.000000000000000000 ) ) ;
#33386 = LINE ( 'NONE', #11430, #166 ) ;
#33387 = VERTEX_POINT ( 'NONE', #9075 ) ;
#33388 = CIRCLE ( 'NONE', #5245, 19.99999999999998579 ) ;
#33389 = CARTESIAN_POINT ( 'NONE',  ( -37.66520193420439711, -114.7490116281687023, 3.058975545821551734 ) ) ;
#33390 = EDGE_LOOP ( 'NONE', ( #16894, #28283, #11001, #7138 ) ) ;
#33391 =( LENGTH_UNIT ( ) NAMED_UNIT ( * ) SI_UNIT ( .MILLI., .METRE. ) );
#33392 = ORIENTED_EDGE ( 'NONE', *, *, #31731, .T. ) ;
#33393 = ORIENTED_EDGE ( 'NONE', *, *, #23165, .T. ) ;
#33394 = DIRECTION ( 'NONE',  ( 0.000000000000000000, 0.000000000000000000, -1.000000000000000000 ) ) ;
#33395 = EDGE_CURVE ( 'NONE', #35062, #17795, #23438, .T. ) ;
#33396 = PRESENTATION_LAYER_ASSIGNMENT (  '', '', ( #30529 ) ) ;
#33397 = VECTOR ( 'NONE', #21963, 1000.000000000000000 ) ;
#33398 = CARTESIAN_POINT ( 'NONE',  ( -35.50000000000000711, -114.3474311500471430, -1.624782352598427959 ) ) ;
#33399 = DIRECTION ( 'NONE',  ( -1.000000000000000000, 0.000000000000000000, 0.000000000000000000 ) ) ;
#33400 = AXIS2_PLACEMENT_3D ( 'NONE', #24814, #10779, #5384 ) ;
#33401 = CARTESIAN_POINT ( 'NONE',  ( -35.50000000000000711, -114.2598117360253696, 9.542047897280109936 ) ) ;
#33402 = CARTESIAN_POINT ( 'NONE',  ( -9.999999999999994671, 0.000000000000000000, 0.000000000000000000 ) ) ;
#33403 = ADVANCED_FACE ( 'NONE', ( #33924 ), #31041, .T. ) ;
#33404 = CARTESIAN_POINT ( 'NONE',  ( 3.872983346207517386, -1.000000000000028644, 65.00000000000000000 ) ) ;
#33405 = CARTESIAN_POINT ( 'NONE',  ( -34.50000000000000000, -114.9925223117477202, 10.47601618151863079 ) ) ;
#33406 = DIRECTION ( 'NONE',  ( 0.000000000000000000, -0.5877852522924621459, -0.8090169943749555559 ) ) ;
#33407 = UNCERTAINTY_MEASURE_WITH_UNIT (LENGTH_MEASURE( 1.000000000000000082E-05 ), #4430, 'distance_accuracy_value', 'NONE');
#33408 = CARTESIAN_POINT ( 'NONE',  ( 7.999999999999992895, -25.61928775981012762, -45.25098998563503727 ) ) ;
#33409 = CARTESIAN_POINT ( 'NONE',  ( -35.50000000000000000, -114.5266723804073195, 8.577838247824468354 ) ) ;
#33410 = CARTESIAN_POINT ( 'NONE',  ( -35.50000000000000711, -112.0221129971568104, -0.7553032835231431319 ) ) ;
#33411 = DIRECTION ( 'NONE',  ( -1.000000000000000000, 0.000000000000000000, 0.000000000000000000 ) ) ;
#33412 = CYLINDRICAL_SURFACE ( 'NONE', #32554, 7.199999999999993072 ) ;
#33413 = FACE_BOUND ( 'NONE', #26315, .T. ) ;
#33414 = DIRECTION ( 'NONE',  ( -1.000000000000000000, -0.000000000000000000, -0.000000000000000000 ) ) ;
#33415 = DIRECTION ( 'NONE',  ( -1.000000000000000000, -0.000000000000000000, -0.000000000000000000 ) ) ;
#33416 = VERTEX_POINT ( 'NONE', #27652 ) ;
#33417 = VECTOR ( 'NONE', #26313, 1000.000000000000000 ) ;
#33418 = CARTESIAN_POINT ( 'NONE',  ( -34.97545270896703329, -114.7691647218148745, 8.590225545821551734 ) ) ;
#33419 = AXIS2_PLACEMENT_3D ( 'NONE', #2341, #35278, #32553 ) ;
#33420 = FACE_OUTER_BOUND ( 'NONE', #33099, .T. ) ;
#33421 = CARTESIAN_POINT ( 'NONE',  ( 0.000000000000000000, 42.41764978026606769, 20.20639853260304619 ) ) ;
#33422 = EDGE_CURVE ( 'NONE', #19029, #17673, #11360, .T. ) ;
#33423 = CYLINDRICAL_SURFACE ( 'NONE', #18831, 4.800000000000000711 ) ;
#33424 = ORIENTED_EDGE ( 'NONE', *, *, #1887, .F. ) ;
#33425 = ORIENTED_EDGE ( 'NONE', *, *, #4160, .T. ) ;
#33426 = CYLINDRICAL_SURFACE ( 'NONE', #28663, 15.49899999999998457 ) ;
#33427 = DIRECTION ( 'NONE',  ( 0.000000000000000000, 0.7071067811865483499, -0.7071067811865466846 ) ) ;
#33428 = VERTEX_POINT ( 'NONE', #11429 ) ;
#33429 = ORIENTED_EDGE ( 'NONE', *, *, #8348, .F. ) ;
#33430 = EDGE_CURVE ( 'NONE', #7962, #17785, #4496, .T. ) ;
#33431 = DIRECTION ( 'NONE',  ( 0.000000000000000000, 0.8660254037844380415, 0.5000000000000012212 ) ) ;
#33432 = EDGE_CURVE ( 'NONE', #15848, #34028, #33128, .T. ) ;
#33433 = DIRECTION ( 'NONE',  ( 0.000000000000000000, 0.000000000000000000, 1.000000000000000000 ) ) ;
#33434 = CIRCLE ( 'NONE', #3588, 47.49900000000001654 ) ;
#33435 = APPLICATION_PROTOCOL_DEFINITION ( 'draft international standard', 'automotive_design', 1998, #14895 ) ;
#33436 = DIRECTION ( 'NONE',  ( -1.000000000000000000, 0.000000000000000000, 0.000000000000000000 ) ) ;
#33437 = EDGE_LOOP ( 'NONE', ( #14387, #31658, #18474, #6465 ) ) ;
#33438 = ORIENTED_EDGE ( 'NONE', *, *, #24181, .F. ) ;
#33439 = DIRECTION ( 'NONE',  ( 0.000000000000000000, 0.000000000000000000, 1.000000000000000000 ) ) ;
#33440 = EDGE_CURVE ( 'NONE', #34283, #2896, #28606, .T. ) ;
#33441 = DIRECTION ( 'NONE',  ( 1.000000000000000000, 0.000000000000000000, 0.000000000000000000 ) ) ;
#33442 = CIRCLE ( 'NONE', #17916, 10.99999999999999645 ) ;
#33443 = ORIENTED_EDGE ( 'NONE', *, *, #34780, .T. ) ;
#33444 = AXIS2_PLACEMENT_3D ( 'NONE', #31272, #9836, #20439 ) ;
#33445 = CARTESIAN_POINT ( 'NONE',  ( 0.1085714285714300953, -3.798448662927791819, 0.000000000000000000 ) ) ;
#33446 = EDGE_CURVE ( 'NONE', #6691, #19596, #18255, .T. ) ;
#33447 = CARTESIAN_POINT ( 'NONE',  ( -34.50000000000000000, -115.0140978167138712, -0.1247823525984438492 ) ) ;
#33448 = DIRECTION ( 'NONE',  ( -1.000000000000000000, 0.000000000000000000, 0.000000000000000000 ) ) ;
#33449 = CARTESIAN_POINT ( 'NONE',  ( -42.49999999999999289, -11.98076211353319742, 83.49999999999992895 ) ) ;
#33450 = CARTESIAN_POINT ( 'NONE',  ( -34.50000000000000000, -114.2356323198232673, 8.521029492159460261 ) ) ;
#33451 = FACE_BOUND ( 'NONE', #24929, .T. ) ;
#33452 = DIRECTION ( 'NONE',  ( 0.000000000000000000, -1.000000000000000000, 0.000000000000000000 ) ) ;
#33453 = CARTESIAN_POINT ( 'NONE',  ( -37.34375000000001421, -114.9929510916434339, 14.11852480586264846 ) ) ;
#33454 = CARTESIAN_POINT ( 'NONE',  ( 8.000000000000007105, 7.613867765417711375, -5.679790370315948245 ) ) ;
#33455 = LINE ( 'NONE', #8779, #595 ) ;
#33456 = AXIS2_PLACEMENT_3D ( 'NONE', #10802, #19063, #21759 ) ;
#33457 = CARTESIAN_POINT ( 'NONE',  ( 0.000000000000000000, 0.000000000000000000, 0.000000000000000000 ) ) ;
#33458 = CARTESIAN_POINT ( 'NONE',  ( 0.000000000000000000, -2.710505431213761085E-17, -45.89999999999999858 ) ) ;
#33459 = ORIENTED_EDGE ( 'NONE', *, *, #26516, .T. ) ;
#33460 = DIRECTION ( 'NONE',  ( 1.000000000000000000, -5.339440136655842133E-16, -1.047965281155519420E-16 ) ) ;
#33461 = EDGE_LOOP ( 'NONE', ( #13914, #18420, #25011, #8228 ) ) ;
#33462 = CARTESIAN_POINT ( 'NONE',  ( -38.30190309005061522, -116.9754527089670546, 3.472274454178448710 ) ) ;
#33463 = DIRECTION ( 'NONE',  ( -1.000000000000000000, 0.000000000000000000, 0.000000000000000000 ) ) ;
#33464 = EDGE_CURVE ( 'NONE', #20157, #27614, #34948, .T. ) ;
#33465 = CARTESIAN_POINT ( 'NONE',  ( -35.50000000000000711, -112.0140978167138712, -0.4997823525984337878 ) ) ;
#33466 = VERTEX_POINT ( 'NONE', #18905 ) ;
#33467 = VERTEX_POINT ( 'NONE', #30252 ) ;
#33468 = CARTESIAN_POINT ( 'NONE',  ( 8.000000000000000000, -16.59870953437682672, 10.45300502024378453 ) ) ;
#33469 = PRODUCT_RELATED_PRODUCT_CATEGORY ( 'part', '', ( #28786 ) ) ;
#33470 = DIRECTION ( 'NONE',  ( 0.000000000000000000, 1.000000000000000000, 0.000000000000000000 ) ) ;
#33471 = ORIENTED_EDGE ( 'NONE', *, *, #11890, .T. ) ;
#33472 = AXIS2_PLACEMENT_3D ( 'NONE', #3883, #11607, #17530 ) ;
#33473 = DIRECTION ( 'NONE',  ( 0.000000000000000000, 0.000000000000000000, 1.000000000000000000 ) ) ;
#33474 = ADVANCED_FACE ( 'NONE', ( #8093 ), #10632, .T. ) ;
#33475 = FACE_BOUND ( 'NONE', #18907, .T. ) ;
#33476 = ORIENTED_EDGE ( 'NONE', *, *, #10831, .F. ) ;
#33477 = VERTEX_POINT ( 'NONE', #32770 ) ;
#33478 = EDGE_CURVE ( 'NONE', #23042, #24581, #2371, .T. ) ;
#33479 = DIRECTION ( 'NONE',  ( -1.000000000000000000, 0.000000000000000000, -0.000000000000000000 ) ) ;
#33480 = EDGE_CURVE ( 'NONE', #27296, #13147, #32077, .T. ) ;
#33481 = FACE_OUTER_BOUND ( 'NONE', #2491, .T. ) ;
#33482 = ORIENTED_EDGE ( 'NONE', *, *, #2697, .F. ) ;
#33483 = ORIENTED_EDGE ( 'NONE', *, *, #15129, .F. ) ;
#33484 = AXIS2_PLACEMENT_3D ( 'NONE', #18982, #10706, #7999 ) ;
#33485 = CARTESIAN_POINT ( 'NONE',  ( -35.50000000000000000, -111.0360125565790383, 1.176611260687384419 ) ) ;
#33486 = VERTEX_POINT ( 'NONE', #5591 ) ;
#33487 = CARTESIAN_POINT ( 'NONE',  ( -35.50040135968785648, -114.9929510916434339, 12.63896776382214071 ) ) ;
#33488 = EDGE_CURVE ( 'NONE', #7962, #22358, #5243, .T. ) ;
#33489 = CARTESIAN_POINT ( 'NONE',  ( -37.69578139638701941, -113.9929510916434339, 14.10650203519847778 ) ) ;
#33490 = AXIS2_PLACEMENT_3D ( 'NONE', #6883, #32617, #19099 ) ;
#33491 = DIRECTION ( 'NONE',  ( -1.000000000000000000, 0.000000000000000000, 0.000000000000000000 ) ) ;
#33492 = DIRECTION ( 'NONE',  ( 1.000000000000000000, 0.000000000000000000, 0.000000000000000000 ) ) ;
#33493 = AXIS2_PLACEMENT_3D ( 'NONE', #9798, #26372, #1705 ) ;
#33494 = CARTESIAN_POINT ( 'NONE',  ( -34.50481333282507279, -113.9929510916434339, 12.74107470552716315 ) ) ;
#33495 = CARTESIAN_POINT ( 'NONE',  ( -38.95206139890800046, -114.9929510916434339, 13.00730889637963728 ) ) ;
#33496 = CARTESIAN_POINT ( 'NONE',  ( -35.50000000000000711, -114.2598117360253696, 9.542047897280109936 ) ) ;
#33497 = CARTESIAN_POINT ( 'NONE',  ( 0.000000000000000000, 0.000000000000000000, 0.000000000000000000 ) ) ;
#33498 = DIRECTION ( 'NONE',  ( -1.000000000000000000, 0.000000000000000000, 0.000000000000000000 ) ) ;
#33499 = ORIENTED_EDGE ( 'NONE', *, *, #18723, .F. ) ;
#33500 = ORIENTED_EDGE ( 'NONE', *, *, #10998, .T. ) ;
#33501 = CYLINDRICAL_SURFACE ( 'NONE', #2308, 20.00000000000000355 ) ;
#33502 = CARTESIAN_POINT ( 'NONE',  ( 0.000000000000000000, 13.56094713063571078, 50.20060470671747055 ) ) ;
#33503 = EDGE_CURVE ( 'NONE', #19156, #3462, #19074, .T. ) ;
#33504 = ORIENTED_EDGE ( 'NONE', *, *, #25807, .T. ) ;
#33505 = AXIS2_PLACEMENT_3D ( 'NONE', #10064, #6830, #12239 ) ;
#33506 = CARTESIAN_POINT ( 'NONE',  ( 4.000000000000000000, -17.56975900509186062, 9.555290079479195953 ) ) ;
#33507 = ORIENTED_EDGE ( 'NONE', *, *, #30607, .T. ) ;
#33508 = VECTOR ( 'NONE', #28331, 1000.000000000000000 ) ;
#33509 = CARTESIAN_POINT ( 'NONE',  ( -35.50000000000000000, -115.0140978167138712, -0.6247823525984418369 ) ) ;
#33510 = CARTESIAN_POINT ( 'NONE',  ( 1.799999999999996048, 0.000000000000000000, 0.000000000000000000 ) ) ;
#33511 = EDGE_CURVE ( 'NONE', #27872, #12895, #27028, .T. ) ;
#33512 = CARTESIAN_POINT ( 'NONE',  ( -36.23083527818512550, -116.0245472910329880, 4.784774454178448266 ) ) ;
#33513 = ORIENTED_EDGE ( 'NONE', *, *, #23772, .F. ) ;
#33514 = CARTESIAN_POINT ( 'NONE',  ( 3.413765605486549060, -14.29811891091956078, -1.200000000000006617 ) ) ;
#33515 = ORIENTED_EDGE ( 'NONE', *, *, #30824, .T. ) ;
#33516 = CARTESIAN_POINT ( 'NONE',  ( -21.15833593587365513, -28.69486372867102375, 88.29903810567654432 ) ) ;
#33517 = AXIS2_PLACEMENT_3D ( 'NONE', #2810, #24754, #21319 ) ;
#33518 = CARTESIAN_POINT ( 'NONE',  ( -35.50000000000000711, -112.4434344552011282, 1.705278471174987986 ) ) ;
#33519 = AXIS2_PLACEMENT_3D ( 'NONE', #31150, #35120, #26830 ) ;
#33520 = ORIENTED_EDGE ( 'NONE', *, *, #10550, .T. ) ;
#33521 = EDGE_LOOP ( 'NONE', ( #3737, #16231, #35042, #9530 ) ) ;
#33522 = EDGE_CURVE ( 'NONE', #10666, #19094, #26900, .T. ) ;
#33523 = DIRECTION ( 'NONE',  ( -1.000000000000000000, -1.836970198721029934E-16, -0.000000000000000000 ) ) ;
#33524 = EDGE_CURVE ( 'NONE', #22087, #18383, #11159, .T. ) ;
#33525 =( NAMED_UNIT ( * ) PLANE_ANGLE_UNIT ( ) SI_UNIT ( $, .RADIAN. ) );
#33526 = DIRECTION ( 'NONE',  ( 0.000000000000000000, 0.9980267284282712259, 0.06279051952931682945 ) ) ;
#33527 = EDGE_LOOP ( 'NONE', ( #5259, #22218 ) ) ;
#33528 = ORIENTED_EDGE ( 'NONE', *, *, #26894, .T. ) ;
#33529 = CARTESIAN_POINT ( 'NONE',  ( -34.50000000000000000, -115.0140978167139707, -0.6091573525984161908 ) ) ;
#33530 = DIRECTION ( 'NONE',  ( -1.000000000000000000, -0.000000000000000000, -0.000000000000000000 ) ) ;
#33531 = VERTEX_POINT ( 'NONE', #21590 ) ;
#33532 = ORIENTED_EDGE ( 'NONE', *, *, #26844, .F. ) ;
#33533 = LINE ( 'NONE', #33709, #528 ) ;
#33534 = VECTOR ( 'NONE', #18876, 1000.000000000000000 ) ;
#33535 = CARTESIAN_POINT ( 'NONE',  ( -35.50000000000000000, -113.9929510916434339, 10.50625754673587409 ) ) ;
#33536 = DIRECTION ( 'NONE',  ( 0.000000000000000000, 0.8660254037844428154, -0.4999999999999929501 ) ) ;
#33537 = CARTESIAN_POINT ( 'NONE',  ( -55.00000000000000000, -25.98076211353320275, 78.99999999999992895 ) ) ;
#33538 = CARTESIAN_POINT ( 'NONE',  ( -34.50000000000000000, -111.0687598768285369, 1.355111303971038073 ) ) ;
#33539 = CARTESIAN_POINT ( 'NONE',  ( -35.50000000000000000, -114.7000328234681206, 8.631511418192262752 ) ) ;
#33540 = DIRECTION ( 'NONE',  ( 0.000000000000000000, -0.8090169943749534465, 0.5877852522924649215 ) ) ;
#33542 = CIRCLE ( 'NONE', #5947, 4.000000000000000000 ) ;
#33541 = DIRECTION ( 'NONE',  ( -1.174092375852890260E-15, 4.222049128630259891E-16, 1.000000000000000000 ) ) ;
#33543 = VECTOR ( 'NONE', #28237, 1000.000000000000000 ) ;
#33544 = VECTOR ( 'NONE', #18056, 1000.000000000000000 ) ;
#33545 = CARTESIAN_POINT ( 'NONE',  ( 7.999999999999992895, 0.000000000000000000, 0.000000000000000000 ) ) ;
#33546 = DIRECTION ( 'NONE',  ( -1.000000000000000000, -0.000000000000000000, -0.000000000000000000 ) ) ;
#33547 = DIRECTION ( 'NONE',  ( -1.000000000000000000, 0.000000000000000000, 0.000000000000000000 ) ) ;
#33548 = ADVANCED_FACE ( 'NONE', ( #12671 ), #5416, .T. ) ;
#33549 = VERTEX_POINT ( 'NONE', #16363 ) ;
#33550 = DIRECTION ( 'NONE',  ( -1.000000000000000000, 0.000000000000000000, 0.000000000000000000 ) ) ;
#33551 = DIRECTION ( 'NONE',  ( 0.000000000000000000, -0.2486898871648415832, -0.9685831611286344067 ) ) ;
#33552 = ADVANCED_FACE ( 'NONE', ( #13691 ), #24671, .T. ) ;
#33553 = DIRECTION ( 'NONE',  ( -1.000000000000000000, 0.000000000000000000, 0.000000000000000000 ) ) ;
#33554 = CARTESIAN_POINT ( 'NONE',  ( 115.0000000000000000, 81.48267994499606459, 30.15054357219658954 ) ) ;
#33555 = CONTEXT_DEPENDENT_SHAPE_REPRESENTATION ( #13144, #34843 ) ;
#33556 = DIRECTION ( 'NONE',  ( -1.000000000000000000, -1.734723475976807094E-16, -0.000000000000000000 ) ) ;
#33557 = CARTESIAN_POINT ( 'NONE',  ( -34.49999999999998579, -4.633167542791596816, 143.9590043477703887 ) ) ;
#33558 = ORIENTED_EDGE ( 'NONE', *, *, #34346, .T. ) ;
#33559 = DIRECTION ( 'NONE',  ( 0.000000000000000000, 0.000000000000000000, -1.000000000000000000 ) ) ;
#33560 = CARTESIAN_POINT ( 'NONE',  ( 0.000000000000000000, 17.06000345190438949, 10.43821259704026794 ) ) ;
#33561 = DIRECTION ( 'NONE',  ( -1.000000000000000000, 0.000000000000000000, 0.000000000000000000 ) ) ;
#33562 = ORIENTED_EDGE ( 'NONE', *, *, #8110, .F. ) ;
#33563 = CARTESIAN_POINT ( 'NONE',  ( -35.99999999999999289, -113.9407375970686758, 5.496475545821551734 ) ) ;
#33564 = ORIENTED_EDGE ( 'NONE', *, *, #29239, .F. ) ;
#33565 = ORIENTED_EDGE ( 'NONE', *, *, #10734, .F. ) ;
#33566 = ORIENTED_EDGE ( 'NONE', *, *, #29, .T. ) ;
#33567 = DIRECTION ( 'NONE',  ( -1.000000000000000000, 0.000000000000000000, 0.000000000000000000 ) ) ;
#33568 = CIRCLE ( 'NONE', #6527, 47.49900000000001654 ) ;
#33569 = VECTOR ( 'NONE', #23128, 1000.000000000000000 ) ;
#33570 = ADVANCED_FACE ( 'NONE', ( #9958 ), #8270, .T. ) ;
#33571 = CARTESIAN_POINT ( 'NONE',  ( -35.50000000000000711, -116.0140978167138712, -0.3747823525984422255 ) ) ;
#33572 = DIRECTION ( 'NONE',  ( -1.000000000000000000, 0.000000000000000000, 0.000000000000000000 ) ) ;
#33573 = PLANE ( 'NONE',  #18408 ) ;
#33574 = LINE ( 'NONE', #8905, #30475 ) ;
#33575 = FACE_OUTER_BOUND ( 'NONE', #21292, .T. ) ;
#33576 = CARTESIAN_POINT ( 'NONE',  ( 0.000000000000000000, -21.80633394113448276, -2.912696353506054159 ) ) ;
#33577 = DIRECTION ( 'NONE',  ( -1.000000000000000000, 0.000000000000000000, 0.000000000000000000 ) ) ;
#33578 = DIRECTION ( 'NONE',  ( 8.708451184622495809E-17, -6.938893903907203726E-17, -1.000000000000000000 ) ) ;
#33579 = CARTESIAN_POINT ( 'NONE',  ( -35.50000000000000000, -114.3793648455349654, 8.543708532059524074 ) ) ;
#33580 = CARTESIAN_POINT ( 'NONE',  ( -35.50000000000000711, -112.8356783780338759, 1.859636627348750348 ) ) ;
#33581 = DIRECTION ( 'NONE',  ( -1.000000000000000000, -1.836970198721029934E-16, -0.000000000000000000 ) ) ;
#33582 = CARTESIAN_POINT ( 'NONE',  ( 46.00000000000000000, -25.98076211353320275, 95.99999999999991473 ) ) ;
#33583 = DIRECTION ( 'NONE',  ( -1.000000000000000000, -0.000000000000000000, -0.000000000000000000 ) ) ;
#33584 = LINE ( 'NONE', #25147, #3182 ) ;
#33585 = CIRCLE ( 'NONE', #1975, 5.000000000000004441 ) ;
#33586 = EDGE_CURVE ( 'NONE', #10915, #21999, #12543, .T. ) ;
#33587 = AXIS2_PLACEMENT_3D ( 'NONE', #31522, #6845, #7558 ) ;
#33588 = CARTESIAN_POINT ( 'NONE',  ( 6.071532165918824830E-15, 1.000000000000000000, 30.00000000000000000 ) ) ;
#33589 = DIRECTION ( 'NONE',  ( -1.000000000000000000, 0.000000000000000000, 0.000000000000000000 ) ) ;
#33590 = ORIENTED_EDGE ( 'NONE', *, *, #17935, .F. ) ;
#33591 = CARTESIAN_POINT ( 'NONE',  ( -35.97545270896705460, -114.3549511594417680, 2.590225545821551734 ) ) ;
#33592 = DIRECTION ( 'NONE',  ( 0.000000000000000000, 0.000000000000000000, 1.000000000000000000 ) ) ;
#33593 = DIRECTION ( 'NONE',  ( 0.000000000000000000, 0.2538061376417690140, 0.9672551082808337197 ) ) ;
#33594 = CARTESIAN_POINT ( 'NONE',  ( 0.000000000000000000, -46.90537658765327933, -2.727856614654800005 ) ) ;
#33595 = CIRCLE ( 'NONE', #26153, 6.765000000000044977 ) ;
#33596 = ORIENTED_EDGE ( 'NONE', *, *, #8871, .F. ) ;
#33597 = ORIENTED_EDGE ( 'NONE', *, *, #3697, .F. ) ;
#33598 = DIRECTION ( 'NONE',  ( -1.000000000000000000, 0.000000000000000000, 0.000000000000000000 ) ) ;
#33599 = CARTESIAN_POINT ( 'NONE',  ( 0.000000000000000000, 3.840921266750509488, -47.34345070675166767 ) ) ;
#33600 = ORIENTED_EDGE ( 'NONE', *, *, #6603, .F. ) ;
#33601 = CARTESIAN_POINT ( 'NONE',  ( -39.99999999999999289, -113.9407375970686758, 8.253524454178448266 ) ) ;
#33602 = EDGE_CURVE ( 'NONE', #14042, #28842, #11678, .T. ) ;
#33603 = VERTEX_POINT ( 'NONE', #20123 ) ;
#33604 = CARTESIAN_POINT ( 'NONE',  ( 0.000000000000000000, 10.00000000000000888, -15.00000000000000178 ) ) ;
#33605 = CARTESIAN_POINT ( 'NONE',  ( 8.000000000000000000, -16.53603053422202862, -8.931325931664767737 ) ) ;
#33606 = PRODUCT_CONTEXT ( 'NONE', #1346, 'mechanical' ) ;
#33607 = CARTESIAN_POINT ( 'NONE',  ( 7.999999999999992895, 34.03046037009256963, 33.13733193845818903 ) ) ;
#33608 = ORIENTED_EDGE ( 'NONE', *, *, #15855, .F. ) ;
#33609 = ORIENTED_EDGE ( 'NONE', *, *, #20653, .F. ) ;
#33610 = AXIS2_PLACEMENT_3D ( 'NONE', #22791, #28921, #34507 ) ;
#33611 = AXIS2_PLACEMENT_3D ( 'NONE', #2319, #18666, #13289 ) ;
#33612 = DIRECTION ( 'NONE',  ( 0.000000000000000000, 0.000000000000000000, -1.000000000000000000 ) ) ;
#33613 = CARTESIAN_POINT ( 'NONE',  ( 7.999999999999992895, -15.49408907645203470, 44.90087086784588877 ) ) ;
#33614 = ORIENTED_EDGE ( 'NONE', *, *, #29807, .F. ) ;
#33615 = CARTESIAN_POINT ( 'NONE',  ( 7.999999999999992895, 0.000000000000000000, 0.000000000000000000 ) ) ;
#33616 = AXIS2_PLACEMENT_3D ( 'NONE', #15429, #26442, #21200 ) ;
#33617 = CARTESIAN_POINT ( 'NONE',  ( -34.50000000000000000, -114.0000000000000853, 2.000000000000001776 ) ) ;
#33618 = CARTESIAN_POINT ( 'NONE',  ( 0.000000000000000000, 43.55304910509448035, -28.41006711799937179 ) ) ;
#33619 = CARTESIAN_POINT ( 'NONE',  ( -34.50000000000000000, -116.0140978167138712, 0.3752176474015736507 ) ) ;
#33620 = CARTESIAN_POINT ( 'NONE',  ( -39.00000000000000711, -114.9929510916434339, 10.50625754673587231 ) ) ;
#33621 = CARTESIAN_POINT ( 'NONE',  ( 0.000000000000000000, -3.384281271887945586, 18.48663108841355651 ) ) ;
#33622 = CARTESIAN_POINT ( 'NONE',  ( 7.999999999999992895, 51.93417535146742381, -2.615612846549375536 ) ) ;
#33623 = CARTESIAN_POINT ( 'NONE',  ( -38.99518666717493431, -114.9929510916434339, 12.74107470552714716 ) ) ;
#33624 = DIRECTION ( 'NONE',  ( 0.000000000000000000, -0.5877852522924799095, 0.8090169943749424553 ) ) ;
#33625 = DIRECTION ( 'NONE',  ( -1.000000000000000000, 0.000000000000000000, 0.000000000000000000 ) ) ;
#33626 = CIRCLE ( 'NONE', #34809, 14.00000000000000000 ) ;
#33627 = CARTESIAN_POINT ( 'NONE',  ( 7.999999999999992895, 0.000000000000000000, 0.000000000000000000 ) ) ;
#33628 = CARTESIAN_POINT ( 'NONE',  ( 29.99999999999999289, 45.00000000000000711, 5.510910596163087978E-15 ) ) ;
#33629 = EDGE_CURVE ( 'NONE', #10783, #932, #25740, .T. ) ;
#33630 = ORIENTED_EDGE ( 'NONE', *, *, #25959, .T. ) ;
#33631 = ADVANCED_FACE ( 'NONE', ( #8793 ), #16892, .T. ) ;
#33632 = DIRECTION ( 'NONE',  ( -1.000000000000000000, -1.836970198721029934E-16, -0.000000000000000000 ) ) ;
#33633 = VERTEX_POINT ( 'NONE', #17250 ) ;
#33634 = CARTESIAN_POINT ( 'NONE',  ( -35.81662171581204746, -117.0245472910329738, 6.284774454178449155 ) ) ;
#33635 = CARTESIAN_POINT ( 'NONE',  ( 4.000000000000003553, 35.11945359308164427, -38.34871548465979174 ) ) ;
#33636 = CARTESIAN_POINT ( 'NONE',  ( -35.50000000000000711, -114.9307644833806137, -1.624782352598427959 ) ) ;
#33637 = EDGE_LOOP ( 'NONE', ( #20205, #25413, #1251, #28643 ) ) ;
#33638 = ORIENTED_EDGE ( 'NONE', *, *, #8229, .F. ) ;
#33639 = CLOSED_SHELL ( 'NONE', ( #21082, #25614, #29792, #27150, #28475, #26923, #32191, #34406, #25318, #33403, #6283, #18369, #29040, #12403, #12133, #34505, #9543, #5966, #11895, #1051, #23618, #15833, #30404, #27062, #17668, #33358, #9741, #25518, #506, #5455, #22933, #21977, #1995, #23848, #3135, #10285, #14594, #19787, #20446, #20498, #26256, #33254, #8527, #17670, #17442, #10398, #28685, #17773, #12678, #32602, #13748, #29458, #33659, #7759, #2420, #5171, #15614, #15416, #26716, #4689, #16538, #27444, #31240, #5541, #13853, #4705, #28250, #19588, #20867, #19830, #35294, #3205, #26687, #888, #21536, #18749, #22405, #4887, #29060, #32685, #1853, #22327, #27216, #9260, #11447, #15655, #18638, #2218, #5569, #28050, #10295, #25235, #12510, #11933, #17391, #31858, #22813, #35446, #5061, #31045, #3613, #2043, #24543, #9330, #417, #10121, #27104, #16223, #48, #30008, #7823, #25846, #24684, #21117, #17162, #13266, #21780, #34554, #28670, #2009, #21327, #8424, #479, #21646, #7781, #9706, #32998, #9309, #16959, #34659, #28083, #18938, #3206, #4237, #33570, #3249, #15575, #34635, #18367, #32673, #19645, #25027, #4394, #21586, #31411, #25149, #22605, #9291, #26541, #6602, #8868, #13214, #29796, #27720, #16035, #24302, #12129, #14727, #27760, #6120, #25130, #23818, #29499, #25347, #22871, #4662, #10074, #33241, #17033, #24300, #30670, #32805, #28888, #30273, #24911, #8751, #25569, #21936, #20241, #2327, #17004, #15709, #5922, #30480, #6221, #17077, #22466, #21834, #3345, #23153, #33240, #12145, #30677, #18705, #2567, #18161, #27313, #14887, #11713, #25399, #15192, #14243, #4899, #13187, #21807, #9345, #34109, #4495, #19366, #8334, #27535 ) ) ;
#33641 = CARTESIAN_POINT ( 'NONE',  ( 8.000000000000000000, -6.359167119270591861, 18.96209359615091827 ) ) ;
#33640 = PRODUCT_DEFINITION_SHAPE ( 'NONE', 'NONE',  #35633 ) ;
#33642 = CIRCLE ( 'NONE', #22713, 52.00000000000000711 ) ;
#33643 = DIRECTION ( 'NONE',  ( 0.000000000000000000, 0.000000000000000000, -1.000000000000000000 ) ) ;
#33644 = EDGE_CURVE ( 'NONE', #10690, #21576, #11510, .T. ) ;
#33645 = VERTEX_POINT ( 'NONE', #25020 ) ;
#33646 = CARTESIAN_POINT ( 'NONE',  ( 7.999999999999992895, -26.17370628620682638, 39.63700417846155233 ) ) ;
#33647 = ORIENTED_EDGE ( 'NONE', *, *, #18035, .T. ) ;
#33648 = VERTEX_POINT ( 'NONE', #30596 ) ;
#33649 = CARTESIAN_POINT ( 'NONE',  ( -35.00000000000000000, -113.9407375970686900, 3.996475545821551290 ) ) ;
#33650 = FILL_AREA_STYLE_COLOUR ( '', #13919 ) ;
#33651 = CARTESIAN_POINT ( 'NONE',  ( -39.49999999999999289, -14.17619866229204106, 94.12476896299857287 ) ) ;
#33653 = ORIENTED_EDGE ( 'NONE', *, *, #30688, .T. ) ;
#33652 = CIRCLE ( 'NONE', #32505, 52.00000000000000711 ) ;
#33654 = ORIENTED_EDGE ( 'NONE', *, *, #1547, .T. ) ;
#33655 = CARTESIAN_POINT ( 'NONE',  ( -35.50000000000000000, -111.0140978167138570, 0.7502176474015694874 ) ) ;
#33656 = DIRECTION ( 'NONE',  ( -1.000000000000000000, -0.000000000000000000, -0.000000000000000000 ) ) ;
#33657 = ORIENTED_EDGE ( 'NONE', *, *, #7055, .T. ) ;
#33658 = CARTESIAN_POINT ( 'NONE',  ( -37.46874999999996447, -114.9929510916434339, 13.11852480586264669 ) ) ;
#33659 = ADVANCED_FACE ( 'NONE', ( #28255 ), #33303, .T. ) ;
#33660 = CARTESIAN_POINT ( 'NONE',  ( -38.99984940073100148, -113.9929510916434339, 12.64306614848957544 ) ) ;
#33661 = AXIS2_PLACEMENT_3D ( 'NONE', #11759, #14628, #26163 ) ;
#33662 = DIRECTION ( 'NONE',  ( -0.000000000000000000, -0.000000000000000000, -1.000000000000000000 ) ) ;
#33663 = FACE_OUTER_BOUND ( 'NONE', #26136, .T. ) ;
#33664 = CARTESIAN_POINT ( 'NONE',  ( -36.03125000000003553, -113.9929510916434339, 14.11852480586265024 ) ) ;
#33665 = CARTESIAN_POINT ( 'NONE',  ( -44.00000000000000711, 44.99999999999999289, 5.510910596163087978E-15 ) ) ;
#33666 = AXIS2_PLACEMENT_3D ( 'NONE', #3669, #27970, #11581 ) ;
#33667 = VECTOR ( 'NONE', #6097, 1000.000000000000000 ) ;
#33668 = CARTESIAN_POINT ( 'NONE',  ( -35.50640865667918433, -114.9929510916434339, 12.69998175888958514 ) ) ;
#33669 = CARTESIAN_POINT ( 'NONE',  ( 0.000000000000000000, 5.400000000000013678, 5.082197683525802034E-18 ) ) ;
#33670 = CARTESIAN_POINT ( 'NONE',  ( 1.519999999999994245, 1.327174818595651622E-15, 6.983999999999990216 ) ) ;
#33671 = CARTESIAN_POINT ( 'NONE',  ( 8.000000000000000000, 9.508666619816938947, -19.83898331853677277 ) ) ;
#33672 = EDGE_CURVE ( 'NONE', #31978, #10012, #5079, .T. ) ;
#33673 = ORIENTED_EDGE ( 'NONE', *, *, #30419, .F. ) ;
#33674 = EDGE_CURVE ( 'NONE', #26725, #2211, #6456, .T. ) ;
#33675 = CARTESIAN_POINT ( 'NONE',  ( -35.50000000000000711, -114.5636144531578680, 9.676196722963288366 ) ) ;
#33676 = VERTEX_POINT ( 'NONE', #22647 ) ;
#33677 = EDGE_CURVE ( 'NONE', #16466, #22531, #19758, .T. ) ;
#33678 = DIRECTION ( 'NONE',  ( -1.000000000000000000, 0.000000000000000000, -0.000000000000000000 ) ) ;
#33679 = FACE_OUTER_BOUND ( 'NONE', #34050, .T. ) ;
#33680 = AXIS2_PLACEMENT_3D ( 'NONE', #28950, #10038, #18665 ) ;
#33681 = ORIENTED_EDGE ( 'NONE', *, *, #8226, .F. ) ;
#33682 = CARTESIAN_POINT ( 'NONE',  ( 8.000000000000007105, 0.000000000000000000, 9.499000000000000554 ) ) ;
#33683 = ORIENTED_EDGE ( 'NONE', *, *, #2120, .F. ) ;
#33684 = CARTESIAN_POINT ( 'NONE',  ( -35.50000000000000000, -115.0140978167138712, -0.4997823525984417259 ) ) ;
#33685 = CARTESIAN_POINT ( 'NONE',  ( 7.999999999999992895, 0.000000000000000000, 0.000000000000000000 ) ) ;
#33686 = CARTESIAN_POINT ( 'NONE',  ( -38.45611840935523418, -115.3723087153909432, 2.066024454178448710 ) ) ;
#33687 = EDGE_CURVE ( 'NONE', #18294, #26363, #873, .T. ) ;
#33688 = ORIENTED_EDGE ( 'NONE', *, *, #3733, .F. ) ;
#33689 = CARTESIAN_POINT ( 'NONE',  ( -34.97545270896703329, -113.2308352781851539, 7.409774454178451819 ) ) ;
#33690 = EDGE_CURVE ( 'NONE', #17785, #29087, #3070, .T. ) ;
#33691 = ORIENTED_EDGE ( 'NONE', *, *, #637, .F. ) ;
#33692 = DIRECTION ( 'NONE',  ( 0.000000000000000000, 0.000000000000000000, -1.000000000000000000 ) ) ;
#33693 = CIRCLE ( 'NONE', #30818, 8.000000000000008882 ) ;
#33694 = CARTESIAN_POINT ( 'NONE',  ( -35.50000000000000000, -114.9307644833806137, -2.624782352598442614 ) ) ;
#33695 = ORIENTED_EDGE ( 'NONE', *, *, #2660, .F. ) ;
#33696 = ORIENTED_EDGE ( 'NONE', *, *, #3812, .F. ) ;
#33697 = CARTESIAN_POINT ( 'NONE',  ( -37.76916472181487450, -111.9754527089670404, 4.034774454178449155 ) ) ;
#33698 = AXIS2_PLACEMENT_3D ( 'NONE', #15596, #21367, #34906 ) ;
#33699 =( LENGTH_UNIT ( ) NAMED_UNIT ( * ) SI_UNIT ( .MILLI., .METRE. ) );
#33700 = DIRECTION ( 'NONE',  ( 0.000000000000000000, -0.9822872507286865007, -0.1873813145857354812 ) ) ;
#33701 = ORIENTED_EDGE ( 'NONE', *, *, #33480, .T. ) ;
#33702 = ORIENTED_EDGE ( 'NONE', *, *, #24868, .F. ) ;
#33703 = CARTESIAN_POINT ( 'NONE',  ( -34.50000000000000000, -112.0140978167138712, -0.5622823525984296245 ) ) ;
#33704 = AXIS2_PLACEMENT_3D ( 'NONE', #12173, #34322, #1550 ) ;
#33705 = DIRECTION ( 'NONE',  ( 1.000000000000000000, 0.000000000000000000, 0.000000000000000000 ) ) ;
#33706 = ORIENTED_EDGE ( 'NONE', *, *, #14899, .F. ) ;
#33707 = VERTEX_POINT ( 'NONE', #33641 ) ;
#33708 = AXIS2_PLACEMENT_3D ( 'NONE', #20749, #22926, #23279 ) ;
#33709 = CARTESIAN_POINT ( 'NONE',  ( -49.99999999999998579, -60.00000000000000000, 120.0000000000000000 ) ) ;
#33710 = EDGE_CURVE ( 'NONE', #16181, #532, #27897, .T. ) ;
#33711 = AXIS2_PLACEMENT_3D ( 'NONE', #29135, #4488, #5005 ) ;
#33712 = CARTESIAN_POINT ( 'NONE',  ( -37.48437500000004263, -113.9929510916434339, 13.11852480586264846 ) ) ;
#33713 = ADVANCED_FACE ( 'NONE', ( #3243 ), #14206, .F. ) ;
#33714 = CARTESIAN_POINT ( 'NONE',  ( 50.00005079999999680, 5.399999999999999467, -1.000000000000003109 ) ) ;
#33715 = DIRECTION ( 'NONE',  ( 0.000000000000000000, 0.000000000000000000, -1.000000000000000000 ) ) ;
#33716 = EDGE_CURVE ( 'NONE', #24903, #33265, #7935, .T. ) ;
#33717 = CARTESIAN_POINT ( 'NONE',  ( -34.50000000000000000, -116.0140978167138712, -0.3747823525984422255 ) ) ;
#33718 = CARTESIAN_POINT ( 'NONE',  ( -35.50000000000000000, -114.8124184834118324, 8.677834500183694288 ) ) ;
#33719 = AXIS2_PLACEMENT_3D ( 'NONE', #8254, #18889, #13498 ) ;
#33720 = UNCERTAINTY_MEASURE_WITH_UNIT (LENGTH_MEASURE( 1.000000000000000082E-05 ), #21507, 'distance_accuracy_value', 'NONE');
#33721 = PLANE ( 'NONE',  #33666 ) ;
#33722 = DIRECTION ( 'NONE',  ( -1.000000000000000000, 0.000000000000000000, 0.000000000000000000 ) ) ;
#33723 = EDGE_CURVE ( 'NONE', #34390, #34778, #30948, .T. ) ;
#33724 = FACE_BOUND ( 'NONE', #18987, .T. ) ;
#33725 = CARTESIAN_POINT ( 'NONE',  ( 0.000000000000000000, -24.47917365149914559, -45.87777302070961127 ) ) ;
#33726 = EDGE_CURVE ( 'NONE', #11394, #9366, #22836, .T. ) ;
#33727 = DIRECTION ( 'NONE',  ( 1.000000000000000000, -1.110223024625156540E-16, 0.000000000000000000 ) ) ;
#33728 = CIRCLE ( 'NONE', #6713, 4.000000000000000000 ) ;
#33729 = ORIENTED_EDGE ( 'NONE', *, *, #11259, .F. ) ;
#33730 = VECTOR ( 'NONE', #24936, 1000.000000000000000 ) ;
#33731 = DIRECTION ( 'NONE',  ( -1.000000000000000000, 0.000000000000000000, 0.000000000000000000 ) ) ;
#33732 = FACE_BOUND ( 'NONE', #94, .T. ) ;
#33733 = CARTESIAN_POINT ( 'NONE',  ( -55.00000000000000000, 6.123233995736780087E-16, 5.000000000000011546 ) ) ;
#33734 = DIRECTION ( 'NONE',  ( 0.000000000000000000, 0.3420201433256695456, -0.9396926207859079838 ) ) ;
#33735 = AXIS2_PLACEMENT_3D ( 'NONE', #118, #7858, #11108 ) ;
#33736 = CIRCLE ( 'NONE', #22799, 6.765000000000044977 ) ;
#33737 = CYLINDRICAL_SURFACE ( 'NONE', #2631, 20.00000000000000711 ) ;
#33738 = FACE_OUTER_BOUND ( 'NONE', #10833, .T. ) ;
#33739 = EDGE_CURVE ( 'NONE', #15714, #2729, #3923, .T. ) ;
#33740 = VECTOR ( 'NONE', #8346, 1000.000000000000000 ) ;
#33741 = EDGE_LOOP ( 'NONE', ( #5077, #4165, #2534, #31509 ) ) ;
#33742 = SHAPE_REPRESENTATION ( 'shaft1', ( #21307 ), #32890 ) ;
#33743 = CARTESIAN_POINT ( 'NONE',  ( -9.999999999999994671, 0.000000000000000000, 0.000000000000000000 ) ) ;
#33744 = CYLINDRICAL_SURFACE ( 'NONE', #8474, 52.00000000000000711 ) ;
#33745 = CARTESIAN_POINT ( 'NONE',  ( 1.999999999999998224, 6.989963968728753772E-16, 4.200000000000014388 ) ) ;
#33746 = VERTEX_POINT ( 'NONE', #9338 ) ;
#33747 = ORIENTED_EDGE ( 'NONE', *, *, #22461, .T. ) ;
#33748 = CARTESIAN_POINT ( 'NONE',  ( -36.25098837183130485, -114.6652019342044184, 7.183975545821551734 ) ) ;
#33749 = EDGE_LOOP ( 'NONE', ( #13169, #20748, #35144, #12617 ) ) ;
#33750 = MANIFOLD_SOLID_BREP ( 'Cavity1', #3769 ) ;
#33751 = AXIS2_PLACEMENT_3D ( 'NONE', #26074, #6268, #15064 ) ;
#33752 = ORIENTED_EDGE ( 'NONE', *, *, #30275, .T. ) ;
#33753 = ORIENTED_EDGE ( 'NONE', *, *, #20078, .T. ) ;
#33754 = DIRECTION ( 'NONE',  ( 0.000000000000000000, 0.000000000000000000, -1.000000000000000000 ) ) ;
#33755 = VECTOR ( 'NONE', #2798, 1000.000000000000000 ) ;
#33756 = CARTESIAN_POINT ( 'NONE',  ( -35.50000000000000711, -113.3474311500483935, -1.624782352598427959 ) ) ;
#33757 = CIRCLE ( 'NONE', #21666, 15.49899999999998101 ) ;
#33758 = ADVANCED_FACE ( 'NONE', ( #1782 ), #6284, .T. ) ;
#33759 = DIRECTION ( 'NONE',  ( -1.000000000000000000, -1.836970198721029934E-16, -0.000000000000000000 ) ) ;
#33760 = CIRCLE ( 'NONE', #9029, 3.799999999999999822 ) ;
#33761 = EDGE_CURVE ( 'NONE', #16526, #24903, #26926, .T. ) ;
#33762 = CARTESIAN_POINT ( 'NONE',  ( -36.07812499999994316, -114.9929510916434339, 13.11852480586264669 ) ) ;
#33763 = CARTESIAN_POINT ( 'NONE',  ( -1.000000000000014655, -5.408326913195881325, -0.7999999999999951594 ) ) ;
#33764 = AXIS2_PLACEMENT_3D ( 'NONE', #32853, #8051, #2152 ) ;
#33765 = AXIS2_PLACEMENT_3D ( 'NONE', #31971, #31613, #28920 ) ;
#33766 = DIRECTION ( 'NONE',  ( 0.000000000000000000, 1.000000000000000000, 0.000000000000000000 ) ) ;
#33767 = AXIS2_PLACEMENT_3D ( 'NONE', #15660, #4553, #10290 ) ;
#33768 = CARTESIAN_POINT ( 'NONE',  ( -34.50000000000000000, -114.8211182053456838, 9.932864235516914775 ) ) ;
#33769 = CARTESIAN_POINT ( 'NONE',  ( -39.49999999999999289, 7.019851009788996343, 105.5074730863398003 ) ) ;
#33770 = EDGE_CURVE ( 'NONE', #20492, #17645, #14817, .T. ) ;
#33771 = CYLINDRICAL_SURFACE ( 'NONE', #22628, 47.49900000000001654 ) ;
#33772 = ORIENTED_EDGE ( 'NONE', *, *, #31967, .T. ) ;
#33773 = CARTESIAN_POINT ( 'NONE',  ( -35.50000000000000000, -114.3496480102005251, 8.538090462223289379 ) ) ;
#33774 = CARTESIAN_POINT ( 'NONE',  ( -35.50000000000000711, -112.0140978167138712, 0.3752176474015640473 ) ) ;
#33775 = SURFACE_SIDE_STYLE ('',( #25862 ) ) ;
#33776 = EDGE_CURVE ( 'NONE', #17076, #34725, #4676, .T. ) ;
#33777 = LINE ( 'NONE', #25322, #7284 ) ;
#33778 = AXIS2_PLACEMENT_3D ( 'NONE', #35421, #29847, #27504 ) ;
#33779 = DIRECTION ( 'NONE',  ( -1.000000000000000000, -1.836970198721029934E-16, -0.000000000000000000 ) ) ;
#33780 = CARTESIAN_POINT ( 'NONE',  ( 7.999999999999992895, 27.43636312076321104, 38.14186064215159888 ) ) ;
#33781 = AXIS2_PLACEMENT_3D ( 'NONE', #10217, #4117, #17941 ) ;
#33782 = CARTESIAN_POINT ( 'NONE',  ( 0.9999999999999453770, -6.008326913195871199, 0.000000000000000000 ) ) ;
#33783 = DIRECTION ( 'NONE',  ( -1.000000000000000000, -0.000000000000000000, -0.000000000000000000 ) ) ;
#33784 = VERTEX_POINT ( 'NONE', #1418 ) ;
#33785 = AXIS2_PLACEMENT_3D ( 'NONE', #17272, #30457, #31149 ) ;
#33786 = CARTESIAN_POINT ( 'NONE',  ( -37.66520193420439711, -114.7490116281687023, 7.558975545821551734 ) ) ;
#33787 = CYLINDRICAL_SURFACE ( 'NONE', #16981, 8.000000000000001776 ) ;
#33788 = VECTOR ( 'NONE', #2209, 1000.000000000000000 ) ;
#33789 = FACE_OUTER_BOUND ( 'NONE', #1185, .T. ) ;
#33790 = EDGE_LOOP ( 'NONE', ( #27552, #16058, #29825, #14411 ) ) ;
#33791 = VERTEX_POINT ( 'NONE', #34915 ) ;
#33792 = CIRCLE ( 'NONE', #19955, 47.49900000000000944 ) ;
#33793 = DIRECTION ( 'NONE',  ( 1.000000000000000000, -5.339440136655842133E-16, -1.047965281155519420E-16 ) ) ;
#33794 = DIRECTION ( 'NONE',  ( 0.000000000000000000, 0.7705132427757904745, -0.6374239897486881912 ) ) ;
#33795 = VERTEX_POINT ( 'NONE', #28963 ) ;
#33796 = CARTESIAN_POINT ( 'NONE',  ( -34.92058450342249643, -111.8367748094582197, 3.808975545821551734 ) ) ;
#33797 = ORIENTED_EDGE ( 'NONE', *, *, #4954, .T. ) ;
#33798 = VECTOR ( 'NONE', #2991, 1000.000000000000000 ) ;
#33799 = CARTESIAN_POINT ( 'NONE',  ( 65.00000000000001421, -25.98076211353320986, 91.99999999999994316 ) ) ;
#33800 = CYLINDRICAL_SURFACE ( 'NONE', #21745, 4.980000000000017302 ) ;
#33801 = PRODUCT_CONTEXT ( 'NONE', #3670, 'mechanical' ) ;
#33802 = CYLINDRICAL_SURFACE ( 'NONE', #99, 22.00000000000000000 ) ;
#33803 = VECTOR ( 'NONE', #35, 1000.000000000000000 ) ;
#33804 = EDGE_LOOP ( 'NONE', ( #23075, #14180 ) ) ;
#33805 = ORIENTED_EDGE ( 'NONE', *, *, #25365, .F. ) ;
#33806 = EDGE_CURVE ( 'NONE', #13387, #4303, #9866, .T. ) ;
#33807 = FACE_OUTER_BOUND ( 'NONE', #30967, .T. ) ;
#33808 = DIRECTION ( 'NONE',  ( 0.000000000000000000, 0.000000000000000000, -1.000000000000000000 ) ) ;
#33809 = ORIENTED_EDGE ( 'NONE', *, *, #31215, .F. ) ;
#33810 = DIRECTION ( 'NONE',  ( -1.000000000000000000, 0.000000000000000000, -0.000000000000000000 ) ) ;
#33811 = AXIS2_PLACEMENT_3D ( 'NONE', #33133, #8276, #22137 ) ;
#33812 = CARTESIAN_POINT ( 'NONE',  ( -34.50000000000000000, -113.3557509229967764, 1.923098431109107054 ) ) ;
#33813 = CARTESIAN_POINT ( 'NONE',  ( -3.799999999999999822, 4.653657836759942730E-16, 60.90000000000001279 ) ) ;
#33814 = CARTESIAN_POINT ( 'NONE',  ( -2.000000000000001776, 0.000000000000000000, 0.000000000000000000 ) ) ;
#33815 = CARTESIAN_POINT ( 'NONE',  ( -34.50000000000000000, -115.9929510916434481, 10.53376102667243508 ) ) ;
#33816 = DIRECTION ( 'NONE',  ( 0.000000000000000000, -0.5877852522924796874, 0.8090169943749426773 ) ) ;
#33817 = CYLINDRICAL_SURFACE ( 'NONE', #10556, 4.800000000000000711 ) ;
#33818 = CARTESIAN_POINT ( 'NONE',  ( -34.50000000000000000, -114.2675000158779710, 8.525177020294046670 ) ) ;
#33819 = DIRECTION ( 'NONE',  ( 0.000000000000000000, -0.9048270524660146918, -0.4257792915650830956 ) ) ;
#33820 = AXIS2_PLACEMENT_3D ( 'NONE', #5374, #21542, #11121 ) ;
#33821 = LINE ( 'NONE', #28772, #17804 ) ;
#33822 = FACE_OUTER_BOUND ( 'NONE', #30997, .T. ) ;
#33823 = DIRECTION ( 'NONE',  ( 0.000000000000000000, 0.000000000000000000, -1.000000000000000000 ) ) ;
#33824 = VERTEX_POINT ( 'NONE', #23554 ) ;
#33825 = DIRECTION ( 'NONE',  ( -1.000000000000000000, 0.000000000000000000, 0.000000000000000000 ) ) ;
#33826 = VERTEX_POINT ( 'NONE', #28787 ) ;
#33827 = CARTESIAN_POINT ( 'NONE',  ( -39.97545270896702618, -115.3019030900506152, 7.652725545821552622 ) ) ;
#33828 = CARTESIAN_POINT ( 'NONE',  ( 7.999999999999992895, 20.99948489194422763, 42.60488980472790388 ) ) ;
#33829 = CARTESIAN_POINT ( 'NONE',  ( -35.50000000000000711, -112.0140978167138712, 0.0002176474015661141945 ) ) ;
#33830 = ORIENTED_EDGE ( 'NONE', *, *, #1423, .F. ) ;
#33831 = ORIENTED_EDGE ( 'NONE', *, *, #12631, .F. ) ;
#33832 = FILL_AREA_STYLE_COLOUR ( '', #26349 ) ;
#33833 = CARTESIAN_POINT ( 'NONE',  ( -1.387778780781445676E-14, 0.4273491293403097746, 0.000000000000000000 ) ) ;
#33834 = ORIENTED_EDGE ( 'NONE', *, *, #21648, .F. ) ;
#33835 = AXIS2_PLACEMENT_3D ( 'NONE', #13606, #19006, #16285 ) ;
#33836 = VERTEX_POINT ( 'NONE', #15254 ) ;
#33837 = AXIS2_PLACEMENT_3D ( 'NONE', #12729, #32657, #27443 ) ;
#33838 = LINE ( 'NONE', #20127, #6208 ) ;
#33839 = EDGE_LOOP ( 'NONE', ( #32052, #22380, #7462, #3708 ) ) ;
#33840 = VERTEX_POINT ( 'NONE', #15075 ) ;
#33841 = CARTESIAN_POINT ( 'NONE',  ( -36.94073759706868287, -115.9999999999999858, 7.371475545821551734 ) ) ;
#33842 = CARTESIAN_POINT ( 'NONE',  ( 0.000000000000000000, 0.000000000000000000, 0.000000000000000000 ) ) ;
#33843 = DIRECTION ( 'NONE',  ( 0.000000000000000000, -6.982962677686266711E-15, 1.000000000000000000 ) ) ;
#33844 = ORIENTED_EDGE ( 'NONE', *, *, #8594, .F. ) ;
#33845 = ORIENTED_EDGE ( 'NONE', *, *, #5962, .T. ) ;
#33846 = CARTESIAN_POINT ( 'NONE',  ( -35.50000000000000000, -116.9501796819249222, -1.143161139954000260 ) ) ;
#33847 = EDGE_CURVE ( 'NONE', #19260, #2874, #35560, .T. ) ;
#33848 = FACE_OUTER_BOUND ( 'NONE', #5708, .T. ) ;
#33849 = VERTEX_POINT ( 'NONE', #20828 ) ;
#33850 = CARTESIAN_POINT ( 'NONE',  ( -38.00000000000000711, -114.9929510916434339, 11.21034663311206181 ) ) ;
#33851 = CARTESIAN_POINT ( 'NONE',  ( -39.00000000000000000, -113.9929510916434339, 12.60752341388803721 ) ) ;
#33852 = DIRECTION ( 'NONE',  ( -1.000000000000000000, 0.000000000000000000, 0.000000000000000000 ) ) ;
#33853 = CIRCLE ( 'NONE', #13186, 20.00000000000000711 ) ;
#33854 = CARTESIAN_POINT ( 'NONE',  ( 0.000000000000000000, 13.42368113696687537, -3.975523202427861058 ) ) ;
#33855 = EDGE_CURVE ( 'NONE', #869, #15169, #25790, .T. ) ;
#33856 = CARTESIAN_POINT ( 'NONE',  ( -37.98325232167028531, -113.9929510916434339, 14.04194344061727584 ) ) ;
#33857 = DIRECTION ( 'NONE',  ( 0.000000000000000000, 0.000000000000000000, 1.000000000000000000 ) ) ;
#33858 = CIRCLE ( 'NONE', #21211, 4.000000000000000000 ) ;
#33859 = CARTESIAN_POINT ( 'NONE',  ( -35.97955704204053262, -114.9929510916434339, 13.11812344617474579 ) ) ;
#33860 = CARTESIAN_POINT ( 'NONE',  ( -46.00000000000000000, 0.000000000000000000, 0.000000000000000000 ) ) ;
#33861 = VERTEX_POINT ( 'NONE', #26447 ) ;
#33862 = AXIS2_PLACEMENT_3D ( 'NONE', #22939, #33232, #33938 ) ;
#33863 = DIRECTION ( 'NONE',  ( 0.000000000000000000, 0.000000000000000000, 1.000000000000000000 ) ) ;
#33864 = CARTESIAN_POINT ( 'NONE',  ( 5.400000000000085620, -1.000000000000049516, -52.50000000000000000 ) ) ;
#33865 = ORIENTED_EDGE ( 'NONE', *, *, #3578, .T. ) ;
#33866 = CARTESIAN_POINT ( 'NONE',  ( -35.50000000000000711, -114.9929510916434339, 12.59102132592610523 ) ) ;
#33867 = VERTEX_POINT ( 'NONE', #12222 ) ;
#33868 = CARTESIAN_POINT ( 'NONE',  ( 3.872983346207489852, 0.9999999999999522604, 55.00000000000000711 ) ) ;
#33869 = CARTESIAN_POINT ( 'NONE',  ( -38.37230871539094323, -112.5438815906447729, 3.941024454178448710 ) ) ;
#33870 = ORIENTED_EDGE ( 'NONE', *, *, #22487, .T. ) ;
#33871 = CYLINDRICAL_SURFACE ( 'NONE', #18763, 4.000000000000000000 ) ;
#33872 = ORIENTED_EDGE ( 'NONE', *, *, #20697, .T. ) ;
#33873 = CARTESIAN_POINT ( 'NONE',  ( -35.50000000000000000, -115.0140978167138712, 0.6252176474015650465 ) ) ;
#33874 = CARTESIAN_POINT ( 'NONE',  ( 8.000000000000000000, -0.5097555531871945655, -19.99350267651956159 ) ) ;
#33875 = CARTESIAN_POINT ( 'NONE',  ( -35.02454729103298803, -114.8876895276775087, 3.097274454178448710 ) ) ;
#33876 = ORIENTED_EDGE ( 'NONE', *, *, #29, .F. ) ;
#33877 = CARTESIAN_POINT ( 'NONE',  ( -35.02454729103298803, -114.8876895276775087, 3.097274454178448710 ) ) ;
#33878 = EDGE_CURVE ( 'NONE', #2676, #25030, #15605, .T. ) ;
#33879 = FACE_BOUND ( 'NONE', #23556, .T. ) ;
#33880 = CARTESIAN_POINT ( 'NONE',  ( -35.50000000000000711, -115.9630435732166518, -0.9469505670456015434 ) ) ;
#33881 = ORIENTED_EDGE ( 'NONE', *, *, #5135, .F. ) ;
#33882 = EDGE_LOOP ( 'NONE', ( #12050, #8086, #34068, #3456 ) ) ;
#33883 = LINE ( 'NONE', #9212, #25161 ) ;
#33884 = CARTESIAN_POINT ( 'NONE',  ( 8.000000000000000000, 0.000000000000000000, 0.000000000000000000 ) ) ;
#33885 = VERTEX_POINT ( 'NONE', #23197 ) ;
#33886 = ORIENTED_EDGE ( 'NONE', *, *, #925, .T. ) ;
#33887 = AXIS2_PLACEMENT_3D ( 'NONE', #7231, #1480, #23629 ) ;
#33888 = CARTESIAN_POINT ( 'NONE',  ( -34.50000000000000000, -115.6286452741999113, -1.424448457485488095 ) ) ;
#33889 = CARTESIAN_POINT ( 'NONE',  ( -35.50000000000000711, -113.1256619669233885, 1.895633585076891947 ) ) ;
#33890 = EDGE_CURVE ( 'NONE', #33746, #26146, #22293, .T. ) ;
#33891 = EDGE_CURVE ( 'NONE', #23346, #19686, #1961, .T. ) ;
#33892 = EDGE_CURVE ( 'NONE', #17467, #30036, #6777, .T. ) ;
#33893 = VECTOR ( 'NONE', #21005, 1000.000000000000000 ) ;
#33894 = VERTEX_POINT ( 'NONE', #20475 ) ;
#33895 = ORIENTED_EDGE ( 'NONE', *, *, #1708, .T. ) ;
#33896 = FACE_OUTER_BOUND ( 'NONE', #23569, .T. ) ;
#33897 = CARTESIAN_POINT ( 'NONE',  ( -37.53269373325071712, -113.9929510916434339, 13.11752178341324360 ) ) ;
#33898 = CYLINDRICAL_SURFACE ( 'NONE', #4092, 13.99999999999999822 ) ;
#33899 = CARTESIAN_POINT ( 'NONE',  ( -55.00000000000000000, -25.98076211353320275, 90.99999999999994316 ) ) ;
#33900 = ADVANCED_FACE ( 'NONE', ( #3962 ), #26089, .F. ) ;
#33901 = CARTESIAN_POINT ( 'NONE',  ( -35.50160444427493189, -113.9929510916434339, 12.65937477241749853 ) ) ;
#33902 = EDGE_CURVE ( 'NONE', #3119, #18391, #24625, .T. ) ;
#33903 = CARTESIAN_POINT ( 'NONE',  ( -35.50000000000000000, -115.9929510916434481, 10.52000928670414126 ) ) ;
#33904 = FACE_OUTER_BOUND ( 'NONE', #19857, .T. ) ;
#33905 = CARTESIAN_POINT ( 'NONE',  ( 7.999999999999992895, -46.87740477351715640, -3.172455868805712509 ) ) ;
#33906 = FACE_OUTER_BOUND ( 'NONE', #28865, .T. ) ;
#33907 = CARTESIAN_POINT ( 'NONE',  ( 0.000000000000000000, 3.268936481846368203, -13.61301047812914256 ) ) ;
#33908 = CYLINDRICAL_SURFACE ( 'NONE', #19120, 4.000000000000003553 ) ;
#33909 = ORIENTED_EDGE ( 'NONE', *, *, #22830, .T. ) ;
#33910 = CIRCLE ( 'NONE', #17781, 7.199999999999995737 ) ;
#33911 = DIRECTION ( 'NONE',  ( -0.000000000000000000, 0.000000000000000000, -1.000000000000000000 ) ) ;
#33912 = CARTESIAN_POINT ( 'NONE',  ( 7.999999999999992895, 51.85248208264518865, 3.914090171286368935 ) ) ;
#33913 = DIRECTION ( 'NONE',  ( -1.000000000000000000, -0.000000000000000000, 0.000000000000000000 ) ) ;
#33914 = CARTESIAN_POINT ( 'NONE',  ( -46.00000000000000000, 0.000000000000000000, 11.00000000000000000 ) ) ;
#33915 = ITEM_DEFINED_TRANSFORMATION ( 'NONE', 'NONE', #16060,  #21307 ) ;
#33916 = VECTOR ( 'NONE', #33077, 1000.000000000000000 ) ;
#33917 = PRODUCT_DEFINITION_FORMATION_WITH_SPECIFIED_SOURCE ( 'ANY', '', #17537, .NOT_KNOWN. ) ;
#33918 = VECTOR ( 'NONE', #145, 1000.000000000000000 ) ;
#33919 = DIRECTION ( 'NONE',  ( 1.000000000000000000, 1.387778780781445922E-16, 0.000000000000000000 ) ) ;
#33920 = DIRECTION ( 'NONE',  ( 0.000000000000000000, 0.9822872507286893873, -0.1873813145857213258 ) ) ;
#33921 = EDGE_CURVE ( 'NONE', #24853, #24623, #29233, .T. ) ;
#33922 = EDGE_LOOP ( 'NONE', ( #2061, #19947 ) ) ;
#33923 = CARTESIAN_POINT ( 'NONE',  ( -6.938893903907228378E-15, 0.7408941433508786645, 0.000000000000000000 ) ) ;
#33924 = FACE_OUTER_BOUND ( 'NONE', #29678, .T. ) ;
#33925 = PRODUCT_DEFINITION ( 'UNKNOWN', '', #21264, #11217 ) ;
#33926 = DIRECTION ( 'NONE',  ( -1.000000000000000000, -1.734723475976807094E-16, -0.000000000000000000 ) ) ;
#33927 = ORIENTED_EDGE ( 'NONE', *, *, #16250, .T. ) ;
#33928 = EDGE_LOOP ( 'NONE', ( #14828, #32810, #4226, #31976 ) ) ;
#33929 = CARTESIAN_POINT ( 'NONE',  ( -37.05926240293133134, -115.0000000000000000, 1.878524454178448710 ) ) ;
#33930 = ORIENTED_EDGE ( 'NONE', *, *, #450, .F. ) ;
#33931 = MANIFOLD_SOLID_BREP ( 'Fillet3', #6044 ) ;
#33932 = VERTEX_POINT ( 'NONE', #22090 ) ;
#33933 = EDGE_LOOP ( 'NONE', ( #29141, #35258, #28419, #15259 ) ) ;
#33934 = FACE_OUTER_BOUND ( 'NONE', #4765, .T. ) ;
#33935 = EDGE_CURVE ( 'NONE', #11561, #22225, #20589, .T. ) ;
#33936 = EDGE_CURVE ( 'NONE', #20350, #18294, #481, .T. ) ;
#33937 = EDGE_CURVE ( 'NONE', #6623, #27197, #2857, .T. ) ;
#33938 = DIRECTION ( 'NONE',  ( 0.000000000000000000, 0.000000000000000000, 1.000000000000000000 ) ) ;
#33939 = DIRECTION ( 'NONE',  ( -1.000000000000000000, 0.000000000000000000, 0.000000000000000000 ) ) ;
#33940 = CARTESIAN_POINT ( 'NONE',  ( -35.50000000000000711, -114.9929510916434339, 10.85830208992344303 ) ) ;
#33941 = DIRECTION ( 'NONE',  ( -1.000000000000000000, -0.000000000000000000, 0.000000000000000000 ) ) ;
#33942 = CIRCLE ( 'NONE', #31647, 20.00000000000000711 ) ;
#33943 = AXIS2_PLACEMENT_3D ( 'NONE', #9832, #23333, #29108 ) ;
#33944 = CARTESIAN_POINT ( 'NONE',  ( 8.000000000000000000, 18.48663108841359559, -3.384281271887881637 ) ) ;
#33945 = EDGE_CURVE ( 'NONE', #12138, #17844, #2678, .T. ) ;
#33946 = CARTESIAN_POINT ( 'NONE',  ( -34.50000000000000000, -114.9928438774171582, 10.49113435197128652 ) ) ;
#33947 = CARTESIAN_POINT ( 'NONE',  ( 7.999999999999992895, -17.08890430202718491, -43.76671000081963570 ) ) ;
#33948 = PRODUCT_DEFINITION_SHAPE ( 'NONE', 'NONE',  #35630 ) ;
#33949 = LINE ( 'NONE', #9276, #32424 ) ;
#33950 = ORIENTED_EDGE ( 'NONE', *, *, #1665, .F. ) ;
#33951 = CARTESIAN_POINT ( 'NONE',  ( -35.50000000000000000, -115.9929510916434481, 10.55026311463432087 ) ) ;
#33952 = CARTESIAN_POINT ( 'NONE',  ( -39.49999999999999289, -12.31102132296306451, 91.73752798680880005 ) ) ;
#33953 = CARTESIAN_POINT ( 'NONE',  ( 8.000000000000000000, 0.000000000000000000, 0.000000000000000000 ) ) ;
#33954 = DIRECTION ( 'NONE',  ( 0.000000000000000000, 0.000000000000000000, 1.000000000000000000 ) ) ;
#33955 = DIRECTION ( 'NONE',  ( -1.000000000000000000, 0.000000000000000000, 0.000000000000000000 ) ) ;
#33956 = DIRECTION ( 'NONE',  ( 0.000000000000000000, 0.000000000000000000, -1.000000000000000000 ) ) ;
#33957 = CARTESIAN_POINT ( 'NONE',  ( 3.160591952521676795, -3.281206521718066149, 0.000000000000000000 ) ) ;
#33958 = SHAPE_REPRESENTATION ( 'Heavy-Duty Locking Pawl', ( #21307 ), #6954 ) ;
#33959 = DIRECTION ( 'NONE',  ( -1.000000000000000000, 0.000000000000000000, 0.000000000000000000 ) ) ;
#33960 = FACE_OUTER_BOUND ( 'NONE', #20129, .T. ) ;
#33961 = EDGE_LOOP ( 'NONE', ( #15987, #24215, #19997, #9116 ) ) ;
#33962 = CIRCLE ( 'NONE', #18427, 52.00000000000000711 ) ;
#33963 = CARTESIAN_POINT ( 'NONE',  ( -35.99999999999999289, -113.9407375970686758, 5.496475545821551734 ) ) ;
#33964 = CARTESIAN_POINT ( 'NONE',  ( -21.15833593587365513, -41.45319397786874305, 92.20096189432315725 ) ) ;
#33965 = CARTESIAN_POINT ( 'NONE',  ( 3.872983346207489852, 0.9999999999999522604, 65.00000000000000000 ) ) ;
#33966 = EDGE_CURVE ( 'NONE', #27370, #10671, #13645, .T. ) ;
#33967 = ORIENTED_EDGE ( 'NONE', *, *, #12761, .T. ) ;
#33968 = AXIS2_PLACEMENT_3D ( 'NONE', #29660, #32003, #32183 ) ;
#33969 = VERTEX_POINT ( 'NONE', #31622 ) ;
#33970 = EDGE_CURVE ( 'NONE', #35265, #17430, #34997, .T. ) ;
#33971 = DIRECTION ( 'NONE',  ( -1.000000000000000000, -1.836970198721029934E-16, -0.000000000000000000 ) ) ;
#33972 = ADVANCED_FACE ( 'NONE', ( #24808 ), #18676, .T. ) ;
#33973 = CARTESIAN_POINT ( 'NONE',  ( 55.00000000000000000, 0.000000000000000000, 70.00000000000000000 ) ) ;
#33974 = ORIENTED_EDGE ( 'NONE', *, *, #7091, .F. ) ;
#33975 = CARTESIAN_POINT ( 'NONE',  ( -33.97545270896702618, -112.8166217158120475, 5.909774454178450931 ) ) ;
#33976 = EDGE_LOOP ( 'NONE', ( #14430, #11132, #10021, #449 ) ) ;
#33977 = CIRCLE ( 'NONE', #12723, 47.49900000000001654 ) ;
#33978 = AXIS2_PLACEMENT_3D ( 'NONE', #24685, #30087, #32782 ) ;
#33979 = AXIS2_PLACEMENT_3D ( 'NONE', #18870, #29868, #16152 ) ;
#33980 = CARTESIAN_POINT ( 'NONE',  ( 0.000000000000000000, -2.710505431213761085E-17, -20.99999999999999645 ) ) ;
#33981 = CYLINDRICAL_SURFACE ( 'NONE', #34392, 10.50000000000000178 ) ;
#33982 = ADVANCED_FACE ( 'NONE', ( #4842 ), #7527, .T. ) ;
#33983 = EDGE_CURVE ( 'NONE', #32383, #18097, #6799, .T. ) ;
#33984 = PRODUCT_CONTEXT ( 'NONE', #25960, 'mechanical' ) ;
#33985 = CARTESIAN_POINT ( 'NONE',  ( -35.50000000000000711, -114.0000000000003411, 9.500000000000035527 ) ) ;
#33986 = EDGE_LOOP ( 'NONE', ( #11359, #16438, #27153, #6832 ) ) ;
#33987 = VERTEX_POINT ( 'NONE', #16145 ) ;
#33988 = CARTESIAN_POINT ( 'NONE',  ( 70.00001200000002655, -26.50436088913151167, 88.99999999999992895 ) ) ;
#33989 = CARTESIAN_POINT ( 'NONE',  ( 8.000000000000000000, 19.35373470438997856, -10.46102064772319729 ) ) ;
#33990 = ORIENTED_EDGE ( 'NONE', *, *, #4525, .T. ) ;
#33991 = DIRECTION ( 'NONE',  ( 0.000000000000000000, 0.000000000000000000, -1.000000000000000000 ) ) ;
#33992 = CARTESIAN_POINT ( 'NONE',  ( -34.50000000000000000, -112.7765286249690035, 1.847058736912741583 ) ) ;
#33993 = CARTESIAN_POINT ( 'NONE',  ( 0.000000000000000000, 0.000000000000000000, 0.000000000000000000 ) ) ;
#33994 = DIRECTION ( 'NONE',  ( -1.000000000000000000, 5.339440136655842133E-16, -1.047965281155515476E-16 ) ) ;
#33995 = CARTESIAN_POINT ( 'NONE',  ( -39.00000000000000711, -114.9929510916434339, 12.17846912687782179 ) ) ;
#33996 = LINE ( 'NONE', #9322, #28396 ) ;
#33997 = CARTESIAN_POINT ( 'NONE',  ( 46.00000000000000000, 1.347111479062088405E-15, 11.00000000000000000 ) ) ;
#33998 = CIRCLE ( 'NONE', #18465, 52.00000000000000711 ) ;
#33999 = MECHANICAL_DESIGN_GEOMETRIC_PRESENTATION_REPRESENTATION (  '', ( #20759 ), #25391 ) ;
#34000 = CARTESIAN_POINT ( 'NONE',  ( -38.99999693208653895, -114.9929510916434339, 12.62875129555797749 ) ) ;
#34002 = DIRECTION ( 'NONE',  ( -1.836970198721029934E-16, 1.000000000000000000, 0.000000000000000000 ) ) ;
#34001 = AXIS2_PLACEMENT_3D ( 'NONE', #29517, #26996, #26459 ) ;
#34003 = CARTESIAN_POINT ( 'NONE',  ( -44.00199999999999534, 14.29999999999999893, -3.000000000000002665 ) ) ;
#34004 = CARTESIAN_POINT ( 'NONE',  ( 0.000000000000000000, -15.49408907645203470, 44.90087086784588877 ) ) ;
#34005 = LINE ( 'NONE', #23363, #30187 ) ;
#34006 = ORIENTED_EDGE ( 'NONE', *, *, #14126, .T. ) ;
#34007 = DIRECTION ( 'NONE',  ( -1.000000000000000000, 0.000000000000000000, 0.000000000000000000 ) ) ;
#34008 = EDGE_LOOP ( 'NONE', ( #8980, #25653, #32555, #4592 ) ) ;
#34009 = CARTESIAN_POINT ( 'NONE',  ( -34.92058450342249643, -111.8367748094582197, 6.808975545821551734 ) ) ;
#34010 = DIRECTION ( 'NONE',  ( -1.000000000000000000, 0.000000000000000000, 0.000000000000000000 ) ) ;
#34011 = CARTESIAN_POINT ( 'NONE',  ( -35.50000000000000000, -113.0140978167138712, 0.3752176474015639918 ) ) ;
#34012 = EDGE_CURVE ( 'NONE', #18147, #26998, #32611, .T. ) ;
#34013 = EDGE_LOOP ( 'NONE', ( #34431, #825, #7712, #5330, #29217 ) ) ;
#34014 = VERTEX_POINT ( 'NONE', #14499 ) ;
#34015 = EDGE_CURVE ( 'NONE', #35000, #12018, #17716, .T. ) ;
#34016 = DIRECTION ( 'NONE',  ( 0.000000000000000000, 0.000000000000000000, 1.000000000000000000 ) ) ;
#34017 = CYLINDRICAL_SURFACE ( 'NONE', #16896, 20.00000000000000711 ) ;
#34018 = ORIENTED_EDGE ( 'NONE', *, *, #27246, .F. ) ;
#34019 = ORIENTED_EDGE ( 'NONE', *, *, #18033, .F. ) ;
#34020 = DIRECTION ( 'NONE',  ( -1.000000000000000000, -1.734723475976807094E-16, -0.000000000000000000 ) ) ;
#34021 = ORIENTED_EDGE ( 'NONE', *, *, #14395, .T. ) ;
#34022 = CARTESIAN_POINT ( 'NONE',  ( -37.05926240293131713, -112.0000000000000142, 3.621475545821551290 ) ) ;
#34023 = AXIS2_PLACEMENT_3D ( 'NONE', #9132, #27223, #18919 ) ;
#34024 = AXIS2_PLACEMENT_3D ( 'NONE', #14509, #23339, #17932 ) ;
#34025 = CARTESIAN_POINT ( 'NONE',  ( 30.00000000000000000, 1.359357947053562196E-14, 0.000000000000000000 ) ) ;
#34026 = LINE ( 'NONE', #31842, #10997 ) ;
#34027 = EDGE_LOOP ( 'NONE', ( #20004, #6828 ) ) ;
#34028 = VERTEX_POINT ( 'NONE', #25511 ) ;
#34029 = CARTESIAN_POINT ( 'NONE',  ( -35.50000000000000000, -117.0108842342086888, -0.7556348869410856040 ) ) ;
#34030 = LINE ( 'NONE', #6650, #17789 ) ;
#34031 = EDGE_LOOP ( 'NONE', ( #33831, #29952, #18297, #6817 ) ) ;
#34032 = CARTESIAN_POINT ( 'NONE',  ( -37.99974912065192711, -114.9929510916434339, 12.63488142334838571 ) ) ;
#34033 = CARTESIAN_POINT ( 'NONE',  ( -34.50000000000000000, -114.0743172650041686, 9.508870970061893857 ) ) ;
#34034 = CARTESIAN_POINT ( 'NONE',  ( 0.000000000000000000, 9.604183132802424083, -5.908880290975567995 ) ) ;
#34035 = DIRECTION ( 'NONE',  ( 0.000000000000000000, -0.9980267284282708928, -0.06279051952932446223 ) ) ;
#34036 = CARTESIAN_POINT ( 'NONE',  ( -38.69949915733018742, -113.9929510916434339, 13.54034599209165890 ) ) ;
#34037 = CARTESIAN_POINT ( 'NONE',  ( 4.000000000000003553, -47.32430374665947426, 21.55018039121510398 ) ) ;
#34038 = CARTESIAN_POINT ( 'NONE',  ( -36.03125000000004263, -114.9929510916434339, 13.11852480586264669 ) ) ;
#34039 = DIRECTION ( 'NONE',  ( 1.000000000000000000, 0.000000000000000000, 0.000000000000000000 ) ) ;
#34040 = ORIENTED_EDGE ( 'NONE', *, *, #2370, .F. ) ;
#34041 = CARTESIAN_POINT ( 'NONE',  ( 0.000000000000000000, 0.000000000000000000, 0.000000000000000000 ) ) ;
#34042 = CARTESIAN_POINT ( 'NONE',  ( -34.49999999999998579, -21.98076211353320630, 86.49999999999995737 ) ) ;
#34043 = EDGE_LOOP ( 'NONE', ( #1422, #34217, #33886, #34678, #3649, #32195, #27106, #28529 ) ) ;
#34044 = CARTESIAN_POINT ( 'NONE',  ( -35.50000000000000711, -114.8211182053456838, 9.932864235516914775 ) ) ;
#34045 = EDGE_LOOP ( 'NONE', ( #8419, #10944, #5648, #8497 ) ) ;
#34046 = AXIS2_PLACEMENT_3D ( 'NONE', #13103, #4818, #32514 ) ;
#34047 = CARTESIAN_POINT ( 'NONE',  ( -34.97545270896703329, -113.2308352781851539, 2.909774454178448710 ) ) ;
#34048 = ORIENTED_EDGE ( 'NONE', *, *, #1246, .T. ) ;
#34049 = DIRECTION ( 'NONE',  ( 0.000000000000000000, 0.000000000000000000, -1.000000000000000000 ) ) ;
#34050 = EDGE_LOOP ( 'NONE', ( #15844, #18782, #35494, #35127 ) ) ;
#34051 =( REPRESENTATION_RELATIONSHIP ('NONE','NONE', #26607, #2005 ) REPRESENTATION_RELATIONSHIP_WITH_TRANSFORMATION ( #33915 )SHAPE_REPRESENTATION_RELATIONSHIP( ) );
#34052 = EDGE_CURVE ( 'NONE', #17665, #32586, #22318, .T. ) ;
#34053 = CARTESIAN_POINT ( 'NONE',  ( -35.50000000000000000, -113.0140978167137717, -0.6411448143358797758 ) ) ;
#34054 = DIRECTION ( 'NONE',  ( 0.000000000000000000, 0.4817536741017164337, -0.8763066800438629178 ) ) ;
#34055 = DIRECTION ( 'NONE',  ( 1.000000000000000000, -0.000000000000000000, 0.000000000000000000 ) ) ;
#34056 = EDGE_LOOP ( 'NONE', ( #31004, #1242, #22473, #35482 ) ) ;
#34057 = CARTESIAN_POINT ( 'NONE',  ( -34.97545270896703329, -113.2308352781851539, 2.909774454178448710 ) ) ;
#34058 = STYLED_ITEM ( 'NONE', ( #11066 ), #22718 ) ;
#34059 = FACE_OUTER_BOUND ( 'NONE', #611, .T. ) ;
#34060 = CARTESIAN_POINT ( 'NONE',  ( -35.50000000000000711, -115.2732872103912030, -1.592823285204062911 ) ) ;
#34061 = EDGE_LOOP ( 'NONE', ( #29057, #15568, #4738, #7979 ) ) ;
#34062 = ORIENTED_EDGE ( 'NONE', *, *, #5609, .T. ) ;
#34063 = DIRECTION ( 'NONE',  ( -1.000000000000000000, -0.000000000000000000, 0.000000000000000000 ) ) ;
#34064 = EDGE_CURVE ( 'NONE', #34789, #7837, #7958, .T. ) ;
#34065 =( NAMED_UNIT ( * ) PLANE_ANGLE_UNIT ( ) SI_UNIT ( $, .RADIAN. ) );
#34066 = CARTESIAN_POINT ( 'NONE',  ( 7.999999999999992895, 0.000000000000000000, 0.000000000000000000 ) ) ;
#34067 = ORIENTED_EDGE ( 'NONE', *, *, #16324, .F. ) ;
#34068 = ORIENTED_EDGE ( 'NONE', *, *, #9733, .T. ) ;
#34069 = CARTESIAN_POINT ( 'NONE',  ( -34.50000000000000000, -116.0140978167138712, -0.3122823525984417259 ) ) ;
#34070 = FACE_OUTER_BOUND ( 'NONE', #27193, .T. ) ;
#34071 = VECTOR ( 'NONE', #19270, 1000.000000000000000 ) ;
#34072 = ORIENTED_EDGE ( 'NONE', *, *, #5554, .F. ) ;
#34073 = AXIS2_PLACEMENT_3D ( 'NONE', #29256, #4601, #29430 ) ;
#34074 = ORIENTED_EDGE ( 'NONE', *, *, #19082, .F. ) ;
#34075 = CARTESIAN_POINT ( 'NONE',  ( 7.999999999999992895, 0.000000000000000000, 0.000000000000000000 ) ) ;
#34076 = CARTESIAN_POINT ( 'NONE',  ( -35.74814306589956203, -113.9929510916434339, 13.05539834812772781 ) ) ;
#34077 = DIRECTION ( 'NONE',  ( 0.000000000000000000, -0.4387576694191720472, 0.8986054237126862576 ) ) ;
#34078 = LINE ( 'NONE', #12468, #27198 ) ;
#34079 = CARTESIAN_POINT ( 'NONE',  ( -35.98364338251434447, -113.9929510916434339, 13.11827392651456314 ) ) ;
#34080 = CARTESIAN_POINT ( 'NONE',  ( -35.50000000000000000, -115.9929510916434481, 12.44250253426871033 ) ) ;
#34081 = UNCERTAINTY_MEASURE_WITH_UNIT (LENGTH_MEASURE( 1.000000000000000082E-05 ), #32650, 'distance_accuracy_value', 'NONE');
#34082 = CYLINDRICAL_SURFACE ( 'NONE', #20437, 20.00000000000000711 ) ;
#34083 = CIRCLE ( 'NONE', #22573, 52.00000000000000711 ) ;
#34084 = AXIS2_PLACEMENT_3D ( 'NONE', #33947, #11613, #3706 ) ;
#34085 = CARTESIAN_POINT ( 'NONE',  ( 8.000000000000007105, -11.27190672109260028, 4.484851126495120077 ) ) ;
#34086 = VECTOR ( 'NONE', #2313, 1000.000000000000000 ) ;
#34087 = DIRECTION ( 'NONE',  ( 0.000000000000000000, -1.000000000000000000, 1.067522139062650474E-15 ) ) ;
#34088 = CARTESIAN_POINT ( 'NONE',  ( -1.599999999999989653, -4.871103520542888323E-16, -7.020000000000045759 ) ) ;
#34089 = CARTESIAN_POINT ( 'NONE',  ( 4.000000000000000000, 17.06000345190438949, 10.43821259704026794 ) ) ;
#34090 = ORIENTED_EDGE ( 'NONE', *, *, #1169, .T. ) ;
#34091 = DIRECTION ( 'NONE',  ( 1.000000000000000000, -4.528031003192420052E-15, -1.179290629824070178E-15 ) ) ;
#34092 = CIRCLE ( 'NONE', #2500, 20.00000000000000711 ) ;
#34093 = EDGE_CURVE ( 'NONE', #5736, #12434, #24077, .T. ) ;
#34094 = CARTESIAN_POINT ( 'NONE',  ( -21.15833593587365513, -24.48076211353314591, 80.99999999999991473 ) ) ;
#34095 = CARTESIAN_POINT ( 'NONE',  ( 7.999999999999992895, -17.08890430202718491, -43.76671000081963570 ) ) ;
#34096 = EDGE_CURVE ( 'NONE', #30700, #14767, #33262, .T. ) ;
#34097 = VECTOR ( 'NONE', #33926, 1000.000000000000000 ) ;
#34098 = DIRECTION ( 'NONE',  ( 0.000000000000000000, 0.000000000000000000, 1.000000000000000000 ) ) ;
#34099 = DIRECTION ( 'NONE',  ( 0.1305261922200497138, 0.9914448613738107152, -1.707538432756455455E-31 ) ) ;
#34100 = VERTEX_POINT ( 'NONE', #33086 ) ;
#34101 = CARTESIAN_POINT ( 'NONE',  ( 8.000000000000000000, 6.336799421340039373, -16.31134495048478428 ) ) ;
#34102 = CARTESIAN_POINT ( 'NONE',  ( -34.50000000000000000, -117.0108842342086888, -0.7556348869410856040 ) ) ;
#34103 = DIRECTION ( 'NONE',  ( -1.000000000000000000, 0.000000000000000000, 0.000000000000000000 ) ) ;
#34104 = ORIENTED_EDGE ( 'NONE', *, *, #26085, .F. ) ;
#34105 = ORIENTED_EDGE ( 'NONE', *, *, #19154, .T. ) ;
#34106 = CARTESIAN_POINT ( 'NONE',  ( -36.52652403469556930, -113.0245472910329880, 2.722274454178449155 ) ) ;
#34107 = ADVANCED_FACE ( 'NONE', ( #20077 ), #33426, .T. ) ;
#34108 = EDGE_LOOP ( 'NONE', ( #16414, #3967, #26724, #29922 ) ) ;
#34109 = ADVANCED_FACE ( 'NONE', ( #30731 ), #6414, .T. ) ;
#34111 = ORIENTED_EDGE ( 'NONE', *, *, #2267, .T. ) ;
#34110 = AXIS2_PLACEMENT_3D ( 'NONE', #26820, #34204, #4151 ) ;
#34112 = VERTEX_POINT ( 'NONE', #14159 ) ;
#34113 = CARTESIAN_POINT ( 'NONE',  ( -35.50000000000000000, -115.0140978167138712, -0.6247823525984418369 ) ) ;
#34114 = VECTOR ( 'NONE', #17326, 1000.000000000000000 ) ;
#34115 = DIRECTION ( 'NONE',  ( 0.000000000000000000, 0.000000000000000000, -1.000000000000000000 ) ) ;
#34116 = DIRECTION ( 'NONE',  ( 1.000000000000000000, 1.734723475976807094E-16, 0.000000000000000000 ) ) ;
#34117 = CARTESIAN_POINT ( 'NONE',  ( -35.50000000000000711, -114.9929510916434339, 10.53376102667243508 ) ) ;
#34118 = CIRCLE ( 'NONE', #4244, 20.00000000000000711 ) ;
#34119 = DIRECTION ( 'NONE',  ( 0.000000000000000000, 0.000000000000000000, 1.000000000000000000 ) ) ;
#34120 = VECTOR ( 'NONE', #7442, 1000.000000000000000 ) ;
#34121 = CARTESIAN_POINT ( 'NONE',  ( -1.799999999999996048, 0.000000000000000000, 0.000000000000000000 ) ) ;
#34122 = EDGE_CURVE ( 'NONE', #28798, #4346, #17382, .T. ) ;
#34123 = CARTESIAN_POINT ( 'NONE',  ( -35.90191880024783444, -114.9929510916434339, 14.11551573851448893 ) ) ;
#34124 = CARTESIAN_POINT ( 'NONE',  ( -1.387778780781445676E-14, 0.4273491293403097746, 0.000000000000000000 ) ) ;
#34125 = CARTESIAN_POINT ( 'NONE',  ( 7.999999999999992895, 46.21320724403665281, -10.97699764141904488 ) ) ;
#34126 = ORIENTED_EDGE ( 'NONE', *, *, #14308, .F. ) ;
#34127 = CARTESIAN_POINT ( 'NONE',  ( -35.50000000000000000, -115.9929510916434481, 10.56126450660895699 ) ) ;
#34128 = CARTESIAN_POINT ( 'NONE',  ( -35.50000000000000711, -112.0140978167138712, -0.3122823525984337878 ) ) ;
#34129 = DIRECTION ( 'NONE',  ( 0.000000000000000000, -1.000000000000000000, -1.047252562447196865E-14 ) ) ;
#34130 = CARTESIAN_POINT ( 'NONE',  ( -21.15833593587365513, -23.26666049839539951, 81.70096189432331357 ) ) ;
#34131 = CARTESIAN_POINT ( 'NONE',  ( -34.49999999999998579, -30.19486372867100954, 85.70096189432321410 ) ) ;
#34132 = VECTOR ( 'NONE', #20456, 1000.000000000000000 ) ;
#34133 = CARTESIAN_POINT ( 'NONE',  ( 0.000000000000000000, -19.35373470438990395, 10.46102064772334295 ) ) ;
#34134 = DIRECTION ( 'NONE',  ( -1.000000000000000000, 0.000000000000000000, 0.000000000000000000 ) ) ;
#34135 = EDGE_CURVE ( 'NONE', #4193, #12141, #17068, .T. ) ;
#34136 = DIRECTION ( 'NONE',  ( 0.000000000000000000, 0.000000000000000000, 1.000000000000000000 ) ) ;
#34137 = FACE_BOUND ( 'NONE', #26751, .T. ) ;
#34138 = ORIENTED_EDGE ( 'NONE', *, *, #16107, .F. ) ;
#34139 = EDGE_CURVE ( 'NONE', #19094, #12307, #34425, .T. ) ;
#34140 = EDGE_CURVE ( 'NONE', #10539, #1825, #28041, .T. ) ;
#34141 = CARTESIAN_POINT ( 'NONE',  ( -38.02454729103295961, -113.6450488405582462, 4.840225545821551734 ) ) ;
#34142 = PLANE ( 'NONE',  #10089 ) ;
#34143 = CARTESIAN_POINT ( 'NONE',  ( -42.49999999999999289, -30.19486372867100954, 85.70096189432321410 ) ) ;
#34144 = ORIENTED_EDGE ( 'NONE', *, *, #6134, .T. ) ;
#34145 = EDGE_LOOP ( 'NONE', ( #15645, #2744, #8193, #30259 ) ) ;
#34146 = VECTOR ( 'NONE', #20156, 1000.000000000000000 ) ;
#34147 = CARTESIAN_POINT ( 'NONE',  ( -44.00000000000000000, 3.999999999999993339, 4.898587196589404940E-16 ) ) ;
#34148 = AXIS2_PLACEMENT_3D ( 'NONE', #26195, #9807, #26564 ) ;
#34149 = CYLINDRICAL_SURFACE ( 'NONE', #33610, 4.000000000000000000 ) ;
#34150 = ORIENTED_EDGE ( 'NONE', *, *, #3532, .T. ) ;
#34151 = CARTESIAN_POINT ( 'NONE',  ( -39.16322519054178741, -111.9205845034225177, 6.433975545821551734 ) ) ;
#34152 = EDGE_CURVE ( 'NONE', #24725, #5418, #5024, .T. ) ;
#34153 = ORIENTED_EDGE ( 'NONE', *, *, #13450, .F. ) ;
#34154 = EDGE_CURVE ( 'NONE', #28784, #30634, #9118, .T. ) ;
#34155 = DIRECTION ( 'NONE',  ( -1.000000000000000000, 0.000000000000000000, 0.000000000000000000 ) ) ;
#34156 = DIRECTION ( 'NONE',  ( 0.000000000000000000, 0.000000000000000000, -1.000000000000000000 ) ) ;
#34157 = FACE_OUTER_BOUND ( 'NONE', #9554, .T. ) ;
#34158 = SHAPE_DEFINITION_REPRESENTATION ( #18440, #15534 ) ;
#34159 = DIRECTION ( 'NONE',  ( 0.000000000000000000, 0.000000000000000000, 1.000000000000000000 ) ) ;
#34160 = ORIENTED_EDGE ( 'NONE', *, *, #12316, .T. ) ;
#34161 = ORIENTED_EDGE ( 'NONE', *, *, #23614, .F. ) ;
#34162 = AXIS2_PLACEMENT_3D ( 'NONE', #22198, #33200, #3494 ) ;
#34163 = CARTESIAN_POINT ( 'NONE',  ( 0.000000000000000000, 43.55304910509406824, 28.41006711800001128 ) ) ;
#34164 = CARTESIAN_POINT ( 'NONE',  ( 0.000000000000000000, 17.56975900509174693, 9.555290079479316745 ) ) ;
#34165 = VERTEX_POINT ( 'NONE', #653 ) ;
#34166 = DIRECTION ( 'NONE',  ( 1.000000000000000000, -5.339440136655840161E-16, 0.000000000000000000 ) ) ;
#34167 = EDGE_CURVE ( 'NONE', #8141, #4040, #18802, .T. ) ;
#34168 = CARTESIAN_POINT ( 'NONE',  ( -34.50000000000000000, -115.0140978167137860, -0.6247823525984403936 ) ) ;
#34169 = DIRECTION ( 'NONE',  ( 0.000000000000000000, 0.8660254037844363761, 0.5000000000000037748 ) ) ;
#34170 = CARTESIAN_POINT ( 'NONE',  ( 0.000000000000000000, 22.43957647427220081, -41.27978878573601662 ) ) ;
#34171 = VECTOR ( 'NONE', #8623, 1000.000000000000000 ) ;
#34172 = CARTESIAN_POINT ( 'NONE',  ( -34.50000000000000000, -114.2067765580549832, 8.517583185305328541 ) ) ;
#34173 = EDGE_CURVE ( 'NONE', #532, #27859, #27857, .T. ) ;
#34174 = CARTESIAN_POINT ( 'NONE',  ( 2.000000000000001776, 4.200000000000065015, -2.775557561562891351E-14 ) ) ;
#34175 = CARTESIAN_POINT ( 'NONE',  ( 0.000000000000000000, -2.123073309835510791, 47.45152853935334747 ) ) ;
#34176 = EDGE_CURVE ( 'NONE', #17487, #15308, #15988, .T. ) ;
#34177 = CARTESIAN_POINT ( 'NONE',  ( -38.99699093265173389, -114.9929510916434339, 12.71660600561481402 ) ) ;
#34178 = CYLINDRICAL_SURFACE ( 'NONE', #15898, 20.00000000000000355 ) ;
#34179 = DIRECTION ( 'NONE',  ( 1.000000000000000000, -5.339440136655842133E-16, -1.047965281155519420E-16 ) ) ;
#34180 = CARTESIAN_POINT ( 'NONE',  ( 4.000000000000003553, -18.53613841426757958, -48.58406706613921244 ) ) ;
#34181 = CARTESIAN_POINT ( 'NONE',  ( -44.00000000000000000, -10.99999999999999289, 0.000000000000000000 ) ) ;
#34182 = CARTESIAN_POINT ( 'NONE',  ( 3.983177536951269193, -13.66651769228263724, 0.000000000000000000 ) ) ;
#34183 = VERTEX_POINT ( 'NONE', #6243 ) ;
#34184 = EDGE_CURVE ( 'NONE', #19677, #31595, #17204, .T. ) ;
#34185 = CARTESIAN_POINT ( 'NONE',  ( -35.69809690994941320, -116.9754527089670546, 5.777725545821551734 ) ) ;
#34186 = EDGE_CURVE ( 'NONE', #26304, #12651, #828, .T. ) ;
#34187 = DIRECTION ( 'NONE',  ( 0.000000000000000000, 0.000000000000000000, -1.000000000000000000 ) ) ;
#34188 = CARTESIAN_POINT ( 'NONE',  ( -35.50000000000000711, -116.0140978167138712, -0.1247823525984439463 ) ) ;
#34189 = ORIENTED_EDGE ( 'NONE', *, *, #20623, .T. ) ;
#34190 = ORIENTED_EDGE ( 'NONE', *, *, #27495, .F. ) ;
#34191 = DIRECTION ( 'NONE',  ( -1.000000000000000000, 0.000000000000000000, 0.000000000000000000 ) ) ;
#34192 = ORIENTED_EDGE ( 'NONE', *, *, #32103, .T. ) ;
#34193 = ORIENTED_EDGE ( 'NONE', *, *, #18522, .T. ) ;
#34194 = VECTOR ( 'NONE', #26217, 1000.000000000000000 ) ;
#34195 = DIRECTION ( 'NONE',  ( -1.783119874454246424E-31, -1.187911941725854497E-31, 1.000000000000000000 ) ) ;
#34196 = VECTOR ( 'NONE', #21193, 1000.000000000000000 ) ;
#34197 = CARTESIAN_POINT ( 'NONE',  ( -37.88768952767750875, -112.0245472910329880, 6.527725545821550845 ) ) ;
#34198 =( NAMED_UNIT ( * ) PLANE_ANGLE_UNIT ( ) SI_UNIT ( $, .RADIAN. ) );
#34199 = VECTOR ( 'NONE', #168, 1000.000000000000000 ) ;
#34200 = CYLINDRICAL_SURFACE ( 'NONE', #3523, 13.99999999999999822 ) ;
#34201 = EDGE_LOOP ( 'NONE', ( #15492, #25699, #15662, #29277 ) ) ;
#34202 = VERTEX_POINT ( 'NONE', #4269 ) ;
#34203 = CARTESIAN_POINT ( 'NONE',  ( -35.50000000000000000, -113.0765974847181781, -2.624803185604914102 ) ) ;
#34204 = DIRECTION ( 'NONE',  ( 0.000000000000000000, 0.000000000000000000, 1.000000000000000000 ) ) ;
#34205 = DIRECTION ( 'NONE',  ( 1.000000000000000000, -0.000000000000000000, -0.000000000000000000 ) ) ;
#34206 = ORIENTED_EDGE ( 'NONE', *, *, #17614, .F. ) ;
#34207 = CARTESIAN_POINT ( 'NONE',  ( -37.80727372874345349, -114.9929510916434339, 13.01835785830664527 ) ) ;
#34208 = EDGE_CURVE ( 'NONE', #14643, #19601, #9684, .T. ) ;
#34209 = AXIS2_PLACEMENT_3D ( 'NONE', #27594, #8295, #21806 ) ;
#34210 = EDGE_CURVE ( 'NONE', #18156, #2615, #3917, .T. ) ;
#34211 = CARTESIAN_POINT ( 'NONE',  ( -37.98325232167028531, -113.9929510916434339, 14.04194344061727584 ) ) ;
#34212 = DIRECTION ( 'NONE',  ( -1.000000000000000000, 0.000000000000000000, 0.000000000000000000 ) ) ;
#34213 = LINE ( 'NONE', #3797, #26053 ) ;
#34214 = CARTESIAN_POINT ( 'NONE',  ( -38.99999693208653895, -113.9929510916434339, 12.62875129555797749 ) ) ;
#34215 = DIRECTION ( 'NONE',  ( -1.000000000000000000, 0.000000000000000000, 0.000000000000000000 ) ) ;
#34216 = CARTESIAN_POINT ( 'NONE',  ( -37.43749999999998579, -114.9929510916434339, 13.11852480586264669 ) ) ;
#34217 = ORIENTED_EDGE ( 'NONE', *, *, #17189, .T. ) ;
#34219 = CLOSED_SHELL ( 'NONE', ( #10395, #21163, #33758, #18779, #33972, #6306, #28042, #5618, #9087, #35607, #29972, #13933, #11175, #13229, #6925, #5815, #11281, #14154, #24855, #19193, #30803, #31498, #22209, #35509, #11102, #15736, #5482, #17576 ) ) ;
#34218 = DIRECTION ( 'NONE',  ( -1.000000000000000000, 0.000000000000000000, -0.000000000000000000 ) ) ;
#34220 = DIRECTION ( 'NONE',  ( 0.000000000000000000, 0.000000000000000000, -1.000000000000000000 ) ) ;
#34221 = CIRCLE ( 'NONE', #33093, 3.800000000000018918 ) ;
#34222 = ORIENTED_EDGE ( 'NONE', *, *, #3903, .T. ) ;
#34223 = CARTESIAN_POINT ( 'NONE',  ( -35.50000000000000711, -114.9929510916434339, 12.44250253426871033 ) ) ;
#34224 = ORIENTED_EDGE ( 'NONE', *, *, #8563, .T. ) ;
#34225 = LINE ( 'NONE', #26490, #16853 ) ;
#34226 = MANIFOLD_SOLID_BREP ( 'Boss-Extrude2', #27337 ) ;
#34227 = ORIENTED_EDGE ( 'NONE', *, *, #23845, .T. ) ;
#34228 = CARTESIAN_POINT ( 'NONE',  ( 7.999999999999992895, 37.91532898920963390, -28.61088654061597225 ) ) ;
#34229 = ORIENTED_EDGE ( 'NONE', *, *, #22013, .F. ) ;
#34230 = AXIS2_PLACEMENT_3D ( 'NONE', #18781, #21652, #13564 ) ;
#34231 = CARTESIAN_POINT ( 'NONE',  ( -34.50000000000000000, -113.0140978167137717, 0.8752176474015607166 ) ) ;
#34232 = CARTESIAN_POINT ( 'NONE',  ( 4.000000000000003553, 21.80633394113452539, 2.912696353505896063 ) ) ;
#34233 = CARTESIAN_POINT ( 'NONE',  ( 8.000000000000007105, 0.000000000000000000, 0.000000000000000000 ) ) ;
#34234 = VERTEX_POINT ( 'NONE', #20789 ) ;
#34235 = CARTESIAN_POINT ( 'NONE',  ( -38.45611840935523418, -115.3723087153909432, 5.066024454178449155 ) ) ;
#34236 = AXIS2_PLACEMENT_3D ( 'NONE', #7195, #18362, #5056 ) ;
#34237 = CARTESIAN_POINT ( 'NONE',  ( 4.000000000000003553, 13.61301047812919052, -3.268936481846215880 ) ) ;
#34238 = CARTESIAN_POINT ( 'NONE',  ( -35.50000000000000711, -112.0141059978162019, -0.6575071456984691309 ) ) ;
#34239 = ORIENTED_EDGE ( 'NONE', *, *, #24788, .F. ) ;
#34240 = VERTEX_POINT ( 'NONE', #34506 ) ;
#34241 = CARTESIAN_POINT ( 'NONE',  ( 0.000000000000000000, -2.710505431213761085E-17, -45.00000000000000000 ) ) ;
#34242 =( LENGTH_UNIT ( ) NAMED_UNIT ( * ) SI_UNIT ( .MILLI., .METRE. ) );
#34243 = DIRECTION ( 'NONE',  ( 1.000000000000000000, -0.000000000000000000, -0.000000000000000000 ) ) ;
#34244 = ORIENTED_EDGE ( 'NONE', *, *, #12053, .T. ) ;
#34245 = VERTEX_POINT ( 'NONE', #17744 ) ;
#34246 = CARTESIAN_POINT ( 'NONE',  ( -34.50000000000000000, -114.5974311500472425, -1.624782352598427959 ) ) ;
#34247 = CARTESIAN_POINT ( 'NONE',  ( -35.50000000000000711, -112.9876085932806262, 1.879154677457530065 ) ) ;
#34248 = PRODUCT ( 'Toothed Ratchet Brake Disc', 'Toothed Ratchet Brake Disc', '', ( #28578 ) ) ;
#34249 = AXIS2_PLACEMENT_3D ( 'NONE', #24583, #14280, #27469 ) ;
#34250 = ORIENTED_EDGE ( 'NONE', *, *, #34440, .T. ) ;
#34251 = VERTEX_POINT ( 'NONE', #26045 ) ;
#34252 = DIRECTION ( 'NONE',  ( -1.000000000000000000, 0.000000000000000000, 0.000000000000000000 ) ) ;
#34253 = AXIS2_PLACEMENT_3D ( 'NONE', #5327, #16269, #5677 ) ;
#34254 = EDGE_CURVE ( 'NONE', #18020, #4806, #9470, .T. ) ;
#34255 = CARTESIAN_POINT ( 'NONE',  ( -36.07812499999994316, -113.9929510916434339, 13.11852480586264846 ) ) ;
#34256 = LINE ( 'NONE', #9589, #20829 ) ;
#34257 = CARTESIAN_POINT ( 'NONE',  ( -36.12500000000014211, -113.9929510916434339, 13.11852480586264846 ) ) ;
#34258 = CARTESIAN_POINT ( 'NONE',  ( -35.50000000000000000, -115.9382890315277308, 10.02636389016632812 ) ) ;
#34259 = AXIS2_PLACEMENT_3D ( 'NONE', #26616, #7344, #12571 ) ;
#34260 = DIRECTION ( 'NONE',  ( 0.000000000000000000, 0.000000000000000000, 1.000000000000000000 ) ) ;
#34261 = APPLICATION_CONTEXT ( 'automotive_design' ) ;
#34262 = CARTESIAN_POINT ( 'NONE',  ( -46.00000000000000000, 0.000000000000000000, 70.00000000000000000 ) ) ;
#34263 = EDGE_CURVE ( 'NONE', #28580, #35006, #15342, .T. ) ;
#34264 = DIRECTION ( 'NONE',  ( -1.000000000000000000, -0.000000000000000000, 0.000000000000000000 ) ) ;
#34265 = FACE_OUTER_BOUND ( 'NONE', #13897, .T. ) ;
#34266 = DIRECTION ( 'NONE',  ( 1.000000000000000000, 0.000000000000000000, 0.000000000000000000 ) ) ;
#34267 = EDGE_LOOP ( 'NONE', ( #31968, #8962, #27075, #9637 ) ) ;
#34268 = FACE_BOUND ( 'NONE', #9878, .T. ) ;
#34269 = AXIS2_PLACEMENT_3D ( 'NONE', #18046, #34632, #20916 ) ;
#34270 = CARTESIAN_POINT ( 'NONE',  ( -35.50000000000000711, -112.0460568841087223, -0.8839717462762063382 ) ) ;
#34271 = DIRECTION ( 'NONE',  ( 0.000000000000000000, 0.000000000000000000, -1.000000000000000000 ) ) ;
#34272 = CONTEXT_DEPENDENT_SHAPE_REPRESENTATION ( #8737, #16738 ) ;
#34273 = CARTESIAN_POINT ( 'NONE',  ( -35.50000000000000711, -114.1021862393805577, 9.512197583835053649 ) ) ;
#34274 = CARTESIAN_POINT ( 'NONE',  ( 7.999999999999992895, -44.25018368420724357, -27.31155879685229237 ) ) ;
#34275 = CIRCLE ( 'NONE', #18149, 20.00000000000000711 ) ;
#34276 = CIRCLE ( 'NONE', #6658, 17.49900000000000233 ) ;
#34277 = ORIENTED_EDGE ( 'NONE', *, *, #3094, .T. ) ;
#34278 = AXIS2_PLACEMENT_3D ( 'NONE', #20422, #9465, #12534 ) ;
#34279 = LINE ( 'NONE', #9610, #30834 ) ;
#34280 = CARTESIAN_POINT ( 'NONE',  ( -34.50000000000000000, -113.2224311500466030, -2.624782352598442614 ) ) ;
#34281 = FACE_OUTER_BOUND ( 'NONE', #28099, .T. ) ;
#34282 = VERTEX_POINT ( 'NONE', #14867 ) ;
#34283 = VERTEX_POINT ( 'NONE', #12538 ) ;
#34284 = CARTESIAN_POINT ( 'NONE',  ( -36.25098837183129774, -113.3347980657956242, 4.316024454178448266 ) ) ;
#34285 = ORIENTED_EDGE ( 'NONE', *, *, #24604, .F. ) ;
#34286 = AXIS2_PLACEMENT_3D ( 'NONE', #3339, #33559, #9074 ) ;
#34287 = MANIFOLD_SOLID_BREP ( 'Keyway', #18681 ) ;
#34288 = AXIS2_PLACEMENT_3D ( 'NONE', #11454, #22420, #17911 ) ;
#34289 = ORIENTED_EDGE ( 'NONE', *, *, #30631, .T. ) ;
#34290 = ORIENTED_EDGE ( 'NONE', *, *, #14120, .T. ) ;
#34291 = CARTESIAN_POINT ( 'NONE',  ( -35.50000000000000000, -113.2224311500466030, -0.6247823525984269599 ) ) ;
#34292 = DIRECTION ( 'NONE',  ( 0.000000000000000000, 0.2486898871648552389, -0.9685831611286310761 ) ) ;
#34293 = DIRECTION ( 'NONE',  ( 0.000000000000000000, 0.000000000000000000, 1.000000000000000000 ) ) ;
#34294 = AXIS2_PLACEMENT_3D ( 'NONE', #14756, #14570, #33857 ) ;
#34295 = EDGE_CURVE ( 'NONE', #34234, #26460, #34325, .T. ) ;
#34296 = AXIS2_PLACEMENT_3D ( 'NONE', #2584, #11195, #33165 ) ;
#34297 = CARTESIAN_POINT ( 'NONE',  ( -36.12500000000014211, -114.9929510916434339, 13.11852480586264669 ) ) ;
#34298 = CARTESIAN_POINT ( 'NONE',  ( 4.000000000000003553, -31.08872492059985859, 41.68322423723089543 ) ) ;
#34299 = EDGE_CURVE ( 'NONE', #34977, #6171, #6948, .T. ) ;
#34300 = CARTESIAN_POINT ( 'NONE',  ( 65.00000000000001421, -27.93100416606587899, 81.50764321173589622 ) ) ;
#34301 = VECTOR ( 'NONE', #33330, 1000.000000000000000 ) ;
#34302 = CIRCLE ( 'NONE', #19900, 20.00000000000000711 ) ;
#34303 = CARTESIAN_POINT ( 'NONE',  ( -34.50000000000000000, -114.9929510916434339, 12.59652202191340642 ) ) ;
#34304 = DIRECTION ( 'NONE',  ( 0.000000000000000000, 0.1253332335642974305, 0.9921147013144787641 ) ) ;
#34305 = AXIS2_PLACEMENT_3D ( 'NONE', #17875, #4224, #17701 ) ;
#34306 = FACE_OUTER_BOUND ( 'NONE', #10104, .T. ) ;
#34307 = ORIENTED_EDGE ( 'NONE', *, *, #23155, .T. ) ;
#34308 = EDGE_CURVE ( 'NONE', #25123, #9377, #14788, .T. ) ;
#34309 = CARTESIAN_POINT ( 'NONE',  ( -35.50000000000000000, -115.9929510916434481, 12.59652202191340464 ) ) ;
#34310 = CARTESIAN_POINT ( 'NONE',  ( -35.50000000000000711, -115.2732872103912030, -1.592823285204062911 ) ) ;
#34311 = CIRCLE ( 'NONE', #18778, 4.200000000000014388 ) ;
#34312 = DIRECTION ( 'NONE',  ( 0.000000000000000000, -0.5735764363510502672, 0.8191520442889889120 ) ) ;
#34313 = CARTESIAN_POINT ( 'NONE',  ( -42.49999999999999289, -41.45319397786874305, 92.20096189432315725 ) ) ;
#34314 = AXIS2_PLACEMENT_3D ( 'NONE', #11993, #3713, #33956 ) ;
#34315 = DIRECTION ( 'NONE',  ( 0.000000000000000000, 0.000000000000000000, 1.000000000000000000 ) ) ;
#34316 = CARTESIAN_POINT ( 'NONE',  ( -37.49999999999999289, -11.52052244843579309, 115.1848168619253698 ) ) ;
#34317 = DIRECTION ( 'NONE',  ( 0.000000000000000000, 0.000000000000000000, 1.000000000000000000 ) ) ;
#34318 = DIRECTION ( 'NONE',  ( 1.000000000000000000, -5.339440136655842133E-16, -1.047965281155519420E-16 ) ) ;
#34319 = EDGE_LOOP ( 'NONE', ( #24897, #25686, #7122, #20962 ) ) ;
#34320 = CARTESIAN_POINT ( 'NONE',  ( -35.99999999999999289, -113.9407375970686758, 8.496475545821549957 ) ) ;
#34321 = CYLINDRICAL_SURFACE ( 'NONE', #315, 17.49900000000000233 ) ;
#34322 = DIRECTION ( 'NONE',  ( 1.000000000000000000, 1.836970198721029934E-16, 0.000000000000000000 ) ) ;
#34323 = EDGE_LOOP ( 'NONE', ( #5200, #713, #18872, #12929 ) ) ;
#34324 = VERTEX_POINT ( 'NONE', #18460 ) ;
#34325 = LINE ( 'NONE', #31440, #9034 ) ;
#34326 = AXIS2_PLACEMENT_3D ( 'NONE', #33421, #8742, #3024 ) ;
#34327 = CARTESIAN_POINT ( 'NONE',  ( -42.49999999999999289, -22.68172400785658382, 87.71410161513770731 ) ) ;
#34328 = ORIENTED_EDGE ( 'NONE', *, *, #7385, .T. ) ;
#34329 = CARTESIAN_POINT ( 'NONE',  ( -39.97545270896702618, -115.3019030900506152, 7.652725545821552622 ) ) ;
#34330 = EDGE_LOOP ( 'NONE', ( #23476, #10586, #14724, #9448 ) ) ;
#34331 = EDGE_CURVE ( 'NONE', #2158, #19176, #34943, .T. ) ;
#34332 = AXIS2_PLACEMENT_3D ( 'NONE', #11995, #28027, #9459 ) ;
#34333 = DIRECTION ( 'NONE',  ( 1.000000000000000000, -0.000000000000000000, 0.000000000000000000 ) ) ;
#34334 = AXIS2_PLACEMENT_3D ( 'NONE', #15522, #29241, #29594 ) ;
#34335 = DIRECTION ( 'NONE',  ( -1.000000000000000000, 0.000000000000000000, 0.000000000000000000 ) ) ;
#34336 = VECTOR ( 'NONE', #18265, 1000.000000000000000 ) ;
#34337 = LINE ( 'NONE', #14338, #6793 ) ;
#34338 = AXIS2_PLACEMENT_3D ( 'NONE', #12088, #9206, #25608 ) ;
#34339 = CARTESIAN_POINT ( 'NONE',  ( 7.999999999999992895, -47.22458491092817212, -5.098390039074724100 ) ) ;
#34340 = ORIENTED_EDGE ( 'NONE', *, *, #32436, .F. ) ;
#34341 = ORIENTED_EDGE ( 'NONE', *, *, #26707, .F. ) ;
#34342 = EDGE_CURVE ( 'NONE', #31433, #35453, #2749, .T. ) ;
#34343 = CARTESIAN_POINT ( 'NONE',  ( 70.00001200000001234, -29.98076211353321341, 85.52359877559823076 ) ) ;
#34344 = DIRECTION ( 'NONE',  ( 0.000000000000000000, -6.938893903907203726E-17, -1.000000000000000000 ) ) ;
#34345 = ADVANCED_FACE ( 'NONE', ( #30165 ), #34868, .T. ) ;
#34346 = EDGE_CURVE ( 'NONE', #4839, #11168, #22829, .T. ) ;
#34347 = ORIENTED_EDGE ( 'NONE', *, *, #33395, .T. ) ;
#34348 = CYLINDRICAL_SURFACE ( 'NONE', #7314, 8.000000000000001776 ) ;
#34349 = CARTESIAN_POINT ( 'NONE',  ( 7.999999999999992895, -22.43957647427129842, -41.27978878573651400 ) ) ;
#34350 = DIRECTION ( 'NONE',  ( 0.000000000000000000, -0.5877852522924624790, -0.8090169943749551118 ) ) ;
#34351 = CARTESIAN_POINT ( 'NONE',  ( -37.18750000000004974, -115.9929510916434481, 14.11852480586265024 ) ) ;
#34352 = AXIS2_PLACEMENT_3D ( 'NONE', #10927, #35417, #35243 ) ;
#34353 = CARTESIAN_POINT ( 'NONE',  ( 50.00005079999999680, 0.000000000000000000, 0.000000000000000000 ) ) ;
#34354 = DIRECTION ( 'NONE',  ( -1.000000000000000000, 0.000000000000000000, 0.000000000000000000 ) ) ;
#34355 = ADVANCED_FACE ( 'NONE', ( #18639 ), #4975, .T. ) ;
#34356 = CARTESIAN_POINT ( 'NONE',  ( -37.56132887387857267, -114.9929510916434339, 14.11732072679899197 ) ) ;
#34357 = CARTESIAN_POINT ( 'NONE',  ( 0.000000000000000000, 26.17370628620655282, 39.63700417846173707 ) ) ;
#34358 = AXIS2_PLACEMENT_3D ( 'NONE', #21181, #18655, #24088 ) ;
#34359 = AXIS2_PLACEMENT_3D ( 'NONE', #34094, #22559, #30686 ) ;
#34360 = EDGE_CURVE ( 'NONE', #27914, #6627, #21104, .T. ) ;
#34361 = DIRECTION ( 'NONE',  ( 0.000000000000000000, 0.000000000000000000, 1.000000000000000000 ) ) ;
#34362 = VECTOR ( 'NONE', #30086, 1000.000000000000000 ) ;
#34363 = DIRECTION ( 'NONE',  ( -1.000000000000000000, 0.000000000000000000, 0.000000000000000000 ) ) ;
#34364 = CARTESIAN_POINT ( 'NONE',  ( 0.000000000000000000, 16.59870953437680896, 10.45300502024390354 ) ) ;
#34365 = AXIS2_PLACEMENT_3D ( 'NONE', #14675, #9653, #9295 ) ;
#34366 = CARTESIAN_POINT ( 'NONE',  ( 8.000000000000000000, 0.000000000000000000, 0.000000000000000000 ) ) ;
#34367 = ORIENTED_EDGE ( 'NONE', *, *, #13903, .F. ) ;
#34368 = CARTESIAN_POINT ( 'NONE',  ( -33.97545270896703329, -115.1833782841879810, 2.590225545821551734 ) ) ;
#34369 = AXIS2_PLACEMENT_3D ( 'NONE', #11082, #33044, #2109 ) ;
#34370 = DIRECTION ( 'NONE',  ( -1.783119874454246424E-31, -1.187911941725854497E-31, 1.000000000000000000 ) ) ;
#34371 = CARTESIAN_POINT ( 'NONE',  ( -35.50000000000000000, -113.0140978167136581, 0.8752176474015604946 ) ) ;
#34372 = ORIENTED_EDGE ( 'NONE', *, *, #30581, .F. ) ;
#34373 = VERTEX_POINT ( 'NONE', #15745 ) ;
#34374 = CARTESIAN_POINT ( 'NONE',  ( 7.999999999999992895, 30.93515269692163372, -36.04401931830219752 ) ) ;
#34375 = CARTESIAN_POINT ( 'NONE',  ( -34.49999999999998579, -31.68172400785665488, 97.87435565298206086 ) ) ;
#34376 = ORIENTED_EDGE ( 'NONE', *, *, #10515, .F. ) ;
#34377 = ORIENTED_EDGE ( 'NONE', *, *, #5122, .T. ) ;
#34378 = ORIENTED_EDGE ( 'NONE', *, *, #28206, .F. ) ;
#34379 = EDGE_CURVE ( 'NONE', #17966, #16592, #29178, .T. ) ;
#34380 = AXIS2_PLACEMENT_3D ( 'NONE', #20369, #15511, #31563 ) ;
#34381 = AXIS2_PLACEMENT_3D ( 'NONE', #16390, #34215, #3985 ) ;
#34382 = CARTESIAN_POINT ( 'NONE',  ( -55.00000000000000000, 0.000000000000000000, 0.000000000000000000 ) ) ;
#34383 = PRODUCT_DEFINITION ( 'UNKNOWN', '', #29921, #408 ) ;
#34384 = CARTESIAN_POINT ( 'NONE',  ( -35.00000000000000000, -113.9407375970686900, 6.996475545821551734 ) ) ;
#34385 = EDGE_CURVE ( 'NONE', #2111, #25342, #35053, .T. ) ;
#34386 = AXIS2_PLACEMENT_3D ( 'NONE', #23563, #17610, #28620 ) ;
#34387 = DIRECTION ( 'NONE',  ( -1.000000000000000000, 0.000000000000000000, 0.000000000000000000 ) ) ;
#34388 = FACE_OUTER_BOUND ( 'NONE', #25215, .T. ) ;
#34389 = ORIENTED_EDGE ( 'NONE', *, *, #35524, .T. ) ;
#34390 = VERTEX_POINT ( 'NONE', #21333 ) ;
#34391 = CARTESIAN_POINT ( 'NONE',  ( -35.50000000000000000, -117.0140978167138854, -0.1247823525984438492 ) ) ;
#34392 = AXIS2_PLACEMENT_3D ( 'NONE', #6071, #23162, #6250 ) ;
#34393 = DIRECTION ( 'NONE',  ( 0.000000000000000000, 0.4999999999999898415, 0.8660254037844444808 ) ) ;
#34394 = EDGE_CURVE ( 'NONE', #7117, #1847, #31994, .T. ) ;
#34395 = ADVANCED_FACE ( 'NONE', ( #32326 ), #21501, .T. ) ;
#34396 = LINE ( 'NONE', #14919, #4595 ) ;
#34397 = ORIENTED_EDGE ( 'NONE', *, *, #30229, .T. ) ;
#34398 = AXIS2_PLACEMENT_3D ( 'NONE', #5762, #23651, #20919 ) ;
#34399 = PLANE ( 'NONE',  #35093 ) ;
#34400 = CARTESIAN_POINT ( 'NONE',  ( -34.50000000000000000, -114.9929510916434339, 11.21034663311131929 ) ) ;
#34401 = FACE_OUTER_BOUND ( 'NONE', #16040, .T. ) ;
#34402 = CARTESIAN_POINT ( 'NONE',  ( -37.48437500000004263, -114.9929510916434339, 13.11852480586264669 ) ) ;
#34403 = DIRECTION ( 'NONE',  ( -1.000000000000000000, -0.000000000000000000, 0.000000000000000000 ) ) ;
#34404 = CARTESIAN_POINT ( 'NONE',  ( -34.80050084267116972, -113.9929510916434339, 13.54034599209289347 ) ) ;
#34405 = DIRECTION ( 'NONE',  ( -1.000000000000000000, 0.000000000000000000, 0.000000000000000000 ) ) ;
#34406 = ADVANCED_FACE ( 'NONE', ( #26763 ), #5503, .F. ) ;
#34407 = CARTESIAN_POINT ( 'NONE',  ( -37.48437500000004263, -114.9929510916434339, 13.11852480586264669 ) ) ;
#34408 = CARTESIAN_POINT ( 'NONE',  ( 63.00000000000001421, -28.31857036507964764, 80.03062855292515110 ) ) ;
#34409 = ORIENTED_EDGE ( 'NONE', *, *, #16356, .F. ) ;
#34410 = CARTESIAN_POINT ( 'NONE',  ( 8.000000000000000000, -21.80633394113447920, -2.912696353506051494 ) ) ;
#34411 = CARTESIAN_POINT ( 'NONE',  ( 0.000000000000000000, 0.000000000000000000, 35.10000000000000142 ) ) ;
#34412 = ORIENTED_EDGE ( 'NONE', *, *, #18348, .T. ) ;
#34413 = CARTESIAN_POINT ( 'NONE',  ( -35.50000000000000711, -114.9929510916434339, 10.68227981832981044 ) ) ;
#34414 = ORIENTED_EDGE ( 'NONE', *, *, #6123, .F. ) ;
#34415 = AXIS2_PLACEMENT_3D ( 'NONE', #4105, #34155, #32163 ) ;
#34416 = LINE ( 'NONE', #9732, #34146 ) ;
#34417 = EDGE_LOOP ( 'NONE', ( #6062, #22374, #34192, #6191 ) ) ;
#34418 = VECTOR ( 'NONE', #7983, 1000.000000000000000 ) ;
#34419 = CARTESIAN_POINT ( 'NONE',  ( -34.49999999999998579, -38.85511776651532756, 79.29903810567645905 ) ) ;
#34420 = ORIENTED_EDGE ( 'NONE', *, *, #17566, .F. ) ;
#34421 = CARTESIAN_POINT ( 'NONE',  ( -34.50000000000000000, -113.0140978167138712, 0.8752176474013583229 ) ) ;
#34422 = DIRECTION ( 'NONE',  ( -1.000000000000000000, -0.000000000000000000, 0.000000000000000000 ) ) ;
#34423 = CARTESIAN_POINT ( 'NONE',  ( 7.999999999999992895, -46.77034588191320807, 22.72740077717213936 ) ) ;
#34424 = VERTEX_POINT ( 'NONE', #5159 ) ;
#34425 = CIRCLE ( 'NONE', #20508, 20.00000000000000711 ) ;
#34426 = CARTESIAN_POINT ( 'NONE',  ( -38.45611840935523418, -115.3723087153909432, 2.066024454178448710 ) ) ;
#34427 = EDGE_CURVE ( 'NONE', #16647, #29296, #11861, .T. ) ;
#34428 = EDGE_CURVE ( 'NONE', #35591, #25299, #24408, .T. ) ;
#34429 = LINE ( 'NONE', #34237, #5585 ) ;
#34430 = CARTESIAN_POINT ( 'NONE',  ( -35.50000000000000711, -115.0468226098135744, -1.624774171496087716 ) ) ;
#34431 = ORIENTED_EDGE ( 'NONE', *, *, #4635, .F. ) ;
#34433 = EDGE_LOOP ( 'NONE', ( #9244, #23936 ) ) ;
#34432 = ADVANCED_FACE ( 'NONE', ( #21691, #7482 ), #16459, .F. ) ;
#34434 = CARTESIAN_POINT ( 'NONE',  ( 0.000000000000000000, 9.471478019455348729, -14.71414642875945056 ) ) ;
#34435 = DIRECTION ( 'NONE',  ( 0.000000000000000000, 0.9822872507286892763, -0.1873813145857214646 ) ) ;
#34436 = VERTEX_POINT ( 'NONE', #32692 ) ;
#34437 = VERTEX_POINT ( 'NONE', #2635 ) ;
#34438 = CARTESIAN_POINT ( 'NONE',  ( -34.50000000000000000, -116.0140978167138712, 0.8752176474015622709 ) ) ;
#34439 = CARTESIAN_POINT ( 'NONE',  ( -35.50000000000000711, -112.0577668799241309, 1.173706424699810569 ) ) ;
#34440 = EDGE_CURVE ( 'NONE', #6697, #21923, #4969, .T. ) ;
#34441 = AXIS2_PLACEMENT_3D ( 'NONE', #20797, #15754, #23518 ) ;
#34442 = CARTESIAN_POINT ( 'NONE',  ( 0.000000000000000000, 19.35373470438998211, -10.46102064772319729 ) ) ;
#34443 = VERTEX_POINT ( 'NONE', #8187 ) ;
#34444 = EDGE_LOOP ( 'NONE', ( #34689, #7313, #14, #11593 ) ) ;
#34445 = EDGE_CURVE ( 'NONE', #5380, #6627, #19166, .T. ) ;
#34446 = LINE ( 'NONE', #21080, #20057 ) ;
#34447 = AXIS2_PLACEMENT_3D ( 'NONE', #13048, #5471, #24202 ) ;
#34448 = CARTESIAN_POINT ( 'NONE',  ( -37.52044295795950291, -113.9929510916434339, 13.11812344617477422 ) ) ;
#34449 = CYLINDRICAL_SURFACE ( 'NONE', #7047, 17.49900000000000233 ) ;
#34450 = CARTESIAN_POINT ( 'NONE',  ( -35.83891589277641287, -113.9929510916434339, 13.09299768411358400 ) ) ;
#34451 = CARTESIAN_POINT ( 'NONE',  ( -35.69272627125608466, -115.9929510916434481, 13.01835785830562209 ) ) ;
#34452 = DIRECTION ( 'NONE',  ( -1.000000000000000000, 0.000000000000000000, 0.000000000000000000 ) ) ;
#34453 = DIRECTION ( 'NONE',  ( 0.000000000000000000, 0.000000000000000000, 1.000000000000000000 ) ) ;
#34454 = ORIENTED_EDGE ( 'NONE', *, *, #4761, .F. ) ;
#34455 = DIRECTION ( 'NONE',  ( 0.000000000000000000, 1.067522139062650474E-15, 1.000000000000000000 ) ) ;
#34456 = FACE_OUTER_BOUND ( 'NONE', #14364, .T. ) ;
#34457 = CYLINDRICAL_SURFACE ( 'NONE', #9929, 3.999999999999996447 ) ;
#34458 = ORIENTED_EDGE ( 'NONE', *, *, #33970, .F. ) ;
#34459 = CARTESIAN_POINT ( 'NONE',  ( 3.799999999999999822, 0.000000000000000000, -32.00000000000000000 ) ) ;
#34460 = CARTESIAN_POINT ( 'NONE',  ( -35.50000000000000711, -114.6807644833805000, -1.624782352598427959 ) ) ;
#34461 = CARTESIAN_POINT ( 'NONE',  ( 50.00005079999999680, 3.872983346207417021, 0.9999999999999985567 ) ) ;
#34462 = CONTEXT_DEPENDENT_SHAPE_REPRESENTATION ( #2107, #25916 ) ;
#34463 = CARTESIAN_POINT ( 'NONE',  ( 8.000000000000000000, 0.000000000000000000, 0.000000000000000000 ) ) ;
#34464 = CARTESIAN_POINT ( 'NONE',  ( 0.000000000000000000, -29.60891106212813995, 37.14118181634756866 ) ) ;
#34465 = ORIENTED_EDGE ( 'NONE', *, *, #35085, .F. ) ;
#34466 = AXIS2_PLACEMENT_3D ( 'NONE', #1852, #31554, #1132 ) ;
#34467 = EDGE_CURVE ( 'NONE', #1935, #20040, #15859, .T. ) ;
#34468 = CARTESIAN_POINT ( 'NONE',  ( 0.000000000000000000, -3.840921266749480534, -47.34345070675175293 ) ) ;
#34469 = CARTESIAN_POINT ( 'NONE',  ( -34.50000000000000000, -117.0140978167138854, 0.6252176474015650465 ) ) ;
#34470 = CARTESIAN_POINT ( 'NONE',  ( -35.00000000000000000, -114.0000000000000853, 2.000000000000001776 ) ) ;
#34471 = ORIENTED_EDGE ( 'NONE', *, *, #30160, .F. ) ;
#34472 = ORIENTED_EDGE ( 'NONE', *, *, #26305, .T. ) ;
#34473 = CARTESIAN_POINT ( 'NONE',  ( -37.74901162816869515, -114.6652019342044042, 3.566024454178448710 ) ) ;
#34474 =( LENGTH_UNIT ( ) NAMED_UNIT ( * ) SI_UNIT ( .MILLI., .METRE. ) );
#34475 = ORIENTED_EDGE ( 'NONE', *, *, #6771, .F. ) ;
#34476 = EDGE_LOOP ( 'NONE', ( #33566, #29810, #23493, #28694 ) ) ;
#34477 = CARTESIAN_POINT ( 'NONE',  ( -35.50000000000000000, -114.6807644833805000, -0.6247823525984269599 ) ) ;
#34478 = LINE ( 'NONE', #21127, #31556 ) ;
#34479 = CARTESIAN_POINT ( 'NONE',  ( 0.000000000000000000, -47.22458491092817212, -5.098390039074724100 ) ) ;
#34480 = APPLICATION_CONTEXT ( 'automotive_design' ) ;
#34481 = CARTESIAN_POINT ( 'NONE',  ( -37.18750000000006395, -114.9929510916434339, 13.11852480586264669 ) ) ;
#34482 = DIRECTION ( 'NONE',  ( -1.000000000000000000, 0.000000000000000000, 0.000000000000000000 ) ) ;
#34483 = VECTOR ( 'NONE', #10742, 1000.000000000000000 ) ;
#34484 = CARTESIAN_POINT ( 'NONE',  ( -37.48437500000004263, -114.9929510916434339, 14.11852480586264846 ) ) ;
#34485 = DIRECTION ( 'NONE',  ( 0.000000000000000000, 0.6427876096865403621, -0.7660444431189772363 ) ) ;
#34486 = CIRCLE ( 'NONE', #31592, 4.499999999999990230 ) ;
#34487 = CARTESIAN_POINT ( 'NONE',  ( -44.00000000000000000, 0.000000000000000000, 0.000000000000000000 ) ) ;
#34488 = ORIENTED_EDGE ( 'NONE', *, *, #959, .T. ) ;
#34489 = PRODUCT_DEFINITION_FORMATION_WITH_SPECIFIED_SOURCE ( 'ANY', '', #34248, .NOT_KNOWN. ) ;
#34490 = CARTESIAN_POINT ( 'NONE',  ( -35.50640865667917723, -115.9929510916434481, 12.69998175888958691 ) ) ;
#34491 = CARTESIAN_POINT ( 'NONE',  ( -35.50000000000000711, -113.4307644833805000, -1.624782352598427959 ) ) ;
#34492 = CIRCLE ( 'NONE', #23560, 20.00000000000000711 ) ;
#34493 = DIRECTION ( 'NONE',  ( -1.000000000000000000, -0.000000000000000000, 0.000000000000000000 ) ) ;
#34494 = CARTESIAN_POINT ( 'NONE',  ( 8.000000000000000000, -3.384281271887945586, 18.48663108841355651 ) ) ;
#34495 = DIRECTION ( 'NONE',  ( -1.000000000000000000, -0.000000000000000000, -0.000000000000000000 ) ) ;
#34496 = LINE ( 'NONE', #17548, #8911 ) ;
#34497 = CARTESIAN_POINT ( 'NONE',  ( -55.00000000000000000, -2.775557561562891351E-14, 110.0000000000000000 ) ) ;
#34498 = DIRECTION ( 'NONE',  ( 0.000000000000000000, 0.8660254037844379305, 0.5000000000000011102 ) ) ;
#34499 = ORIENTED_EDGE ( 'NONE', *, *, #17210, .F. ) ;
#34500 = CARTESIAN_POINT ( 'NONE',  ( -35.97545270896702618, -113.6450488405582604, 7.409774454178449155 ) ) ;
#34501 = DIRECTION ( 'NONE',  ( -1.000000000000000000, 0.000000000000000000, -0.000000000000000000 ) ) ;
#34502 = CARTESIAN_POINT ( 'NONE',  ( 8.000000000000000000, 8.605879768205412006, -12.89022243466699535 ) ) ;
#34503 = ORIENTED_EDGE ( 'NONE', *, *, #34295, .T. ) ;
#34504 = ORIENTED_EDGE ( 'NONE', *, *, #16943, .T. ) ;
#34505 = ADVANCED_FACE ( 'NONE', ( #25469 ), #14113, .T. ) ;
#34506 = CARTESIAN_POINT ( 'NONE',  ( 1.599999999999990763, -4.792677538558942720E-14, 4.980000000000000426 ) ) ;
#34507 = DIRECTION ( 'NONE',  ( -1.000000000000000000, 0.000000000000000000, 0.000000000000000000 ) ) ;
#34508 = ORIENTED_EDGE ( 'NONE', *, *, #21274, .T. ) ;
#34509 = CARTESIAN_POINT ( 'NONE',  ( -34.02454729103297382, -112.6980969099494132, 5.402725545821552622 ) ) ;
#34510 = VERTEX_POINT ( 'NONE', #30865 ) ;
#34511 = FILL_AREA_STYLE ('',( #10013 ) ) ;
#34512 = VERTEX_POINT ( 'NONE', #17336 ) ;
#34513 = AXIS2_PLACEMENT_3D ( 'NONE', #8031, #5349, #19014 ) ;
#34514 = DIRECTION ( 'NONE',  ( 0.000000000000000000, 0.000000000000000000, 1.000000000000000000 ) ) ;
#34515 = CYLINDRICAL_SURFACE ( 'NONE', #13143, 20.00000000000000711 ) ;
#34516 = ADVANCED_FACE ( 'NONE', ( #6201, #2823 ), #441, .F. ) ;
#34517 = AXIS2_PLACEMENT_3D ( 'NONE', #17550, #14860, #1367 ) ;
#34518 = PRODUCT_DEFINITION_FORMATION_WITH_SPECIFIED_SOURCE ( 'ANY', '', #4077, .NOT_KNOWN. ) ;
#34519 = DIRECTION ( 'NONE',  ( -1.000000000000000000, 0.000000000000000000, 0.000000000000000000 ) ) ;
#34520 = ORIENTED_EDGE ( 'NONE', *, *, #16068, .T. ) ;
#34521 = ORIENTED_EDGE ( 'NONE', *, *, #21065, .F. ) ;
#34522 = DIRECTION ( 'NONE',  ( -1.000000000000000000, -1.734723475976807094E-16, -0.000000000000000000 ) ) ;
#34523 = FACE_OUTER_BOUND ( 'NONE', #11523, .T. ) ;
#34524 = VERTEX_POINT ( 'NONE', #14291 ) ;
#34525 = CYLINDRICAL_SURFACE ( 'NONE', #4041, 52.00000000000000711 ) ;
#34526 = MANIFOLD_SOLID_BREP ( 'Cavity1', #5493 ) ;
#34527 = CARTESIAN_POINT ( 'NONE',  ( 7.999999999999992895, 44.47301969247469344, -16.68249143361863318 ) ) ;
#34528 = DIRECTION ( 'NONE',  ( 0.000000000000000000, -6.938893903907203726E-17, -1.000000000000000000 ) ) ;
#34529 = CARTESIAN_POINT ( 'NONE',  ( -34.50000000000000000, -115.9929510916434481, 11.38636890470581164 ) ) ;
#34530 = VECTOR ( 'NONE', #7989, 1000.000000000000000 ) ;
#34531 = DIRECTION ( 'NONE',  ( -1.000000000000000000, 0.000000000000000000, 0.000000000000000000 ) ) ;
#34532 = CARTESIAN_POINT ( 'NONE',  ( 8.000000000000007105, 5.363026430117226795, 9.919332006307262972 ) ) ;
#34533 = CARTESIAN_POINT ( 'NONE',  ( -34.50000000000000000, -115.9929510916434481, 10.56126450660895699 ) ) ;
#34534 = CARTESIAN_POINT ( 'NONE',  ( 0.000000000000000000, 0.000000000000000000, 0.000000000000000000 ) ) ;
#34535 = DIRECTION ( 'NONE',  ( 0.000000000000000000, 0.8660254037844381525, 0.5000000000000007772 ) ) ;
#34536 = CIRCLE ( 'NONE', #27660, 12.55910585664918422 ) ;
#34537 = CYLINDRICAL_SURFACE ( 'NONE', #29661, 52.00000000000000711 ) ;
#34538 = DIRECTION ( 'NONE',  ( -1.000000000000000000, 0.000000000000000000, 0.000000000000000000 ) ) ;
#34539 = CYLINDRICAL_SURFACE ( 'NONE', #35468, 10.99999999999999645 ) ;
#34540 = DIRECTION ( 'NONE',  ( -1.000000000000000000, -0.000000000000000000, -0.000000000000000000 ) ) ;
#34541 = EDGE_LOOP ( 'NONE', ( #30874, #10103, #26708, #9819 ) ) ;
#34542 = AXIS2_PLACEMENT_3D ( 'NONE', #12709, #10366, #7298 ) ;
#34543 = CARTESIAN_POINT ( 'NONE',  ( -33.97545270896703329, -115.1833782841879810, 7.090225545821551734 ) ) ;
#34544 = AXIS2_PLACEMENT_3D ( 'NONE', #29387, #29566, #8984 ) ;
#34545 = DIRECTION ( 'NONE',  ( -1.000000000000000000, 0.000000000000000000, -0.000000000000000000 ) ) ;
#34546 = CARTESIAN_POINT ( 'NONE',  ( -35.50000000000000711, -116.0140978167138712, 0.0002176474015577116276 ) ) ;
#34547 = VERTEX_POINT ( 'NONE', #33219 ) ;
#34548 = ORIENTED_EDGE ( 'NONE', *, *, #27556, .F. ) ;
#34549 = EDGE_CURVE ( 'NONE', #22962, #27214, #5682, .T. ) ;
#34551 = CARTESIAN_POINT ( 'NONE',  ( 8.000000000000007105, 11.27190672109280811, -0.3151488735047974776 ) ) ;
#34550 = PRODUCT ( 'spur gear_iso_ISO - Spur gear 2M 20T 20PA 8FW ---S20A75H50L8.0S1', 'spur gear_iso_ISO - Spur gear 2M 20T 20PA 8FW ---S20A75H50L8.0S1', '', ( #33606 ) ) ;
#34552 = DIRECTION ( 'NONE',  ( 1.000000000000000000, -5.339440136655842133E-16, -1.047965281155519420E-16 ) ) ;
#34553 = ORIENTED_EDGE ( 'NONE', *, *, #23305, .F. ) ;
#34554 = ADVANCED_FACE ( 'NONE', ( #27822 ), #11594, .T. ) ;
#34555 = EDGE_LOOP ( 'NONE', ( #31920, #32235, #8856, #25565 ) ) ;
#34556 = ORIENTED_EDGE ( 'NONE', *, *, #12991, .F. ) ;
#34557 = CARTESIAN_POINT ( 'NONE',  ( -10.00000000000000000, 0.000000000000000000, 0.000000000000000000 ) ) ;
#34558 = CARTESIAN_POINT ( 'NONE',  ( -35.00000000000000000, -113.9407375970686900, 8.496475545821551734 ) ) ;
#34559 = EDGE_CURVE ( 'NONE', #453, #35403, #26812, .T. ) ;
#34560 = SURFACE_STYLE_FILL_AREA ( #31313 ) ;
#34561 = EDGE_CURVE ( 'NONE', #15465, #20170, #13013, .T. ) ;
#34562 = DIRECTION ( 'NONE',  ( -1.000000000000000000, 0.000000000000000000, -0.000000000000000000 ) ) ;
#34563 = EDGE_LOOP ( 'NONE', ( #23417, #14780, #1575, #29118 ) ) ;
#34564 = VERTEX_POINT ( 'NONE', #8542 ) ;
#34565 = CARTESIAN_POINT ( 'NONE',  ( -35.50000000000000000, -111.2666036476567655, -1.632210088999287212 ) ) ;
#34566 = DIRECTION ( 'NONE',  ( 1.000000000000000000, 0.000000000000000000, -1.691777834109591283E-31 ) ) ;
#34567 = CARTESIAN_POINT ( 'NONE',  ( -37.49999999999999289, -11.52052244843579309, 115.1848168619253698 ) ) ;
#34568 = AXIS2_PLACEMENT_3D ( 'NONE', #16222, #32638, #24889 ) ;
#34569 = ORIENTED_EDGE ( 'NONE', *, *, #21435, .F. ) ;
#34570 = VECTOR ( 'NONE', #19258, 1000.000000000000000 ) ;
#34571 = DIRECTION ( 'NONE',  ( -1.000000000000000000, 0.000000000000000000, 0.000000000000000000 ) ) ;
#34572 = CARTESIAN_POINT ( 'NONE',  ( -34.50000000000000000, -114.9929510916434339, 10.52826033068511435 ) ) ;
#34573 = LINE ( 'NONE', #9888, #10819 ) ;
#34574 = CARTESIAN_POINT ( 'NONE',  ( -36.03125000000004263, -114.9929510916434339, 13.11852480586264669 ) ) ;
#34575 = DIRECTION ( 'NONE',  ( -1.000000000000000000, -0.000000000000000000, -0.000000000000000000 ) ) ;
#34576 = CARTESIAN_POINT ( 'NONE',  ( -34.50000000000000000, -114.0000000000003411, 9.500000000000035527 ) ) ;
#34577 = LINE ( 'NONE', #15997, #1608 ) ;
#34578 = EDGE_CURVE ( 'NONE', #31888, #23379, #14143, .T. ) ;
#34579 = CARTESIAN_POINT ( 'NONE',  ( -37.53269373325071712, -114.9929510916434339, 13.11752178341324360 ) ) ;
#34580 = DIRECTION ( 'NONE',  ( 0.000000000000000000, 0.000000000000000000, 1.000000000000000000 ) ) ;
#34581 = VERTEX_POINT ( 'NONE', #19678 ) ;
#34582 = FACE_OUTER_BOUND ( 'NONE', #20139, .T. ) ;
#34583 = DIRECTION ( 'NONE',  ( -1.000000000000000000, -0.000000000000000000, -0.000000000000000000 ) ) ;
#34584 = VERTEX_POINT ( 'NONE', #16984 ) ;
#34585 = CARTESIAN_POINT ( 'NONE',  ( -35.50000000000000711, -114.9929510916434339, 10.72628538622835670 ) ) ;
#34586 = ORIENTED_EDGE ( 'NONE', *, *, #7647, .F. ) ;
#34587 = CARTESIAN_POINT ( 'NONE',  ( -36.23083527818512550, -116.0245472910329880, 3.284774454178449155 ) ) ;
#34588 = CARTESIAN_POINT ( 'NONE',  ( -49.99999999999998579, -60.00000000000000000, -25.00000000000000000 ) ) ;
#34589 = ORIENTED_EDGE ( 'NONE', *, *, #8721, .T. ) ;
#34590 = CARTESIAN_POINT ( 'NONE',  ( -34.49999999999998579, -13.17619866229203396, 90.66066734786082293 ) ) ;
#34591 = ORIENTED_EDGE ( 'NONE', *, *, #34, .F. ) ;
#34592 = EDGE_CURVE ( 'NONE', #11649, #19295, #33131, .T. ) ;
#34593 = CARTESIAN_POINT ( 'NONE',  ( -34.50000000000000000, -113.0140978167143260, -0.6247823525984285142 ) ) ;
#34594 = LINE ( 'NONE', #34232, #33417 ) ;
#34595 = CARTESIAN_POINT ( 'NONE',  ( -36.23083527818512550, -116.0245472910329880, 7.784774454178451819 ) ) ;
#34596 = EDGE_CURVE ( 'NONE', #28129, #4109, #8386, .T. ) ;
#34597 = ADVANCED_FACE ( 'NONE', ( #23473 ), #12131, .T. ) ;
#34598 = VECTOR ( 'NONE', #12202, 1000.000000000000000 ) ;
#34599 = VERTEX_POINT ( 'NONE', #23655 ) ;
#34600 = AXIS2_PLACEMENT_3D ( 'NONE', #6998, #34562, #31501 ) ;
#34601 = CARTESIAN_POINT ( 'NONE',  ( -39.97545270896702618, -112.6980969099493990, 3.847274454178448710 ) ) ;
#34602 = CARTESIAN_POINT ( 'NONE',  ( 0.9999999999999870104, -5.408326913195881325, -0.7999999999999951594 ) ) ;
#34603 = CARTESIAN_POINT ( 'NONE',  ( -35.50000000000000711, -115.1446187476384040, -1.616767172155725740 ) ) ;
#34604 = ORIENTED_EDGE ( 'NONE', *, *, #25112, .T. ) ;
#34605 = ORIENTED_EDGE ( 'NONE', *, *, #17197, .F. ) ;
#34606 = LINE ( 'NONE', #11918, #18829 ) ;
#34607 = SURFACE_SIDE_STYLE ('',( #23068 ) ) ;
#34608 = EDGE_CURVE ( 'NONE', #485, #27576, #32551, .T. ) ;
#34609 = LINE ( 'NONE', #1292, #7491 ) ;
#34610 = EDGE_LOOP ( 'NONE', ( #33683, #23233, #2598, #10140 ) ) ;
#34611 = ORIENTED_EDGE ( 'NONE', *, *, #16312, .T. ) ;
#34612 = CARTESIAN_POINT ( 'NONE',  ( -34.50000000000000000, -114.3474311500471430, -1.624782352598427959 ) ) ;
#34613 = CARTESIAN_POINT ( 'NONE',  ( 0.000000000000000000, -2.710505431213761085E-17, -54.99999999999999289 ) ) ;
#34614 = VERTEX_POINT ( 'NONE', #12308 ) ;
#34615 = ORIENTED_EDGE ( 'NONE', *, *, #34621, .F. ) ;
#34616 = LINE ( 'NONE', #12106, #18361 ) ;
#34617 = CARTESIAN_POINT ( 'NONE',  ( -34.50000000000000000, -113.9929510916434197, 10.50625754673586876 ) ) ;
#34618 = DIRECTION ( 'NONE',  ( 0.000000000000000000, -6.866613759074851423E-15, 1.000000000000000000 ) ) ;
#34619 = AXIS2_PLACEMENT_3D ( 'NONE', #4108, #3928, #20092 ) ;
#34620 = CARTESIAN_POINT ( 'NONE',  ( -35.51597953369717686, -113.9929510916434339, 12.74811950270164473 ) ) ;
#34621 = EDGE_CURVE ( 'NONE', #12235, #25221, #31400, .T. ) ;
#34622 = CARTESIAN_POINT ( 'NONE',  ( -38.00000000000000711, -115.9929510916434481, 12.56351784598954779 ) ) ;
#34623 = CARTESIAN_POINT ( 'NONE',  ( 7.999999999999992895, 5.400000000000098943, 1.000000000000000888 ) ) ;
#34624 = CARTESIAN_POINT ( 'NONE',  ( 7.999999999999992895, 0.000000000000000000, 0.000000000000000000 ) ) ;
#34625 = EDGE_CURVE ( 'NONE', #34512, #7954, #24525, .T. ) ;
#34626 = VERTEX_POINT ( 'NONE', #14636 ) ;
#34627 = DIRECTION ( 'NONE',  ( 0.000000000000000000, 0.000000000000000000, 1.000000000000000000 ) ) ;
#34628 = CARTESIAN_POINT ( 'NONE',  ( 7.999999999999992895, -42.03146605346771025, -22.12489237027362421 ) ) ;
#34629 = DIRECTION ( 'NONE',  ( 0.000000000000000000, 0.000000000000000000, 1.000000000000000000 ) ) ;
#34630 = ORIENTED_EDGE ( 'NONE', *, *, #30642, .F. ) ;
#34631 =( GEOMETRIC_REPRESENTATION_CONTEXT ( 3 ) GLOBAL_UNCERTAINTY_ASSIGNED_CONTEXT ( ( #33407 ) ) GLOBAL_UNIT_ASSIGNED_CONTEXT ( ( #4430, #35038, #29443 ) ) REPRESENTATION_CONTEXT ( 'NONE', 'WORKASPACE' ) );
#34632 = DIRECTION ( 'NONE',  ( -1.000000000000000000, -0.000000000000000000, -0.000000000000000000 ) ) ;
#34633 = CARTESIAN_POINT ( 'NONE',  ( -35.50000000000000711, -112.0140978167138712, -0.3122823525984337878 ) ) ;
#34634 = CARTESIAN_POINT ( 'NONE',  ( 0.000000000000000000, 0.000000000000000000, -44.50000000000000000 ) ) ;
#34635 = ADVANCED_FACE ( 'NONE', ( #26359 ), #17878, .T. ) ;
#34636 = DIRECTION ( 'NONE',  ( -1.000000000000000000, 0.000000000000000000, 0.000000000000000000 ) ) ;
#34637 = EDGE_CURVE ( 'NONE', #15571, #32324, #1515, .T. ) ;
#34638 = FACE_OUTER_BOUND ( 'NONE', #25167, .T. ) ;
#34639 = LINE ( 'NONE', #18594, #12483 ) ;
#34640 = EDGE_LOOP ( 'NONE', ( #33597, #20625 ) ) ;
#34641 = CYLINDRICAL_SURFACE ( 'NONE', #6109, 0.7500000000000041078 ) ;
#34642 = CARTESIAN_POINT ( 'NONE',  ( -34.50000000000000000, -113.0974311500471714, -2.624782352598442614 ) ) ;
#34643 = AXIS2_PLACEMENT_3D ( 'NONE', #26879, #24523, #7947 ) ;
#34644 = FACE_OUTER_BOUND ( 'NONE', #34883, .T. ) ;
#34645 = ORIENTED_EDGE ( 'NONE', *, *, #27146, .T. ) ;
#34646 = ORIENTED_EDGE ( 'NONE', *, *, #20054, .T. ) ;
#34647 = CARTESIAN_POINT ( 'NONE',  ( -37.35495115944176092, -112.9754527089670688, 2.534774454178448710 ) ) ;
#34648 = AXIS2_PLACEMENT_3D ( 'NONE', #29651, #13614, #10392 ) ;
#34649 = AXIS2_PLACEMENT_3D ( 'NONE', #25483, #28353, #28890 ) ;
#34650 =( NAMED_UNIT ( * ) SI_UNIT ( $, .STERADIAN. ) SOLID_ANGLE_UNIT ( ) );
#34651 = ORIENTED_EDGE ( 'NONE', *, *, #16752, .T. ) ;
#34652 = VERTEX_POINT ( 'NONE', #26173 ) ;
#34653 = CARTESIAN_POINT ( 'NONE',  ( -34.50000000000000000, -113.7503824761461004, 0.9631051547057219997 ) ) ;
#34654 = DIRECTION ( 'NONE',  ( 0.000000000000000000, 1.000000000000000000, 0.000000000000000000 ) ) ;
#34655 = CARTESIAN_POINT ( 'NONE',  ( 2.000000000000001776, 0.000000000000000000, 0.000000000000000000 ) ) ;
#34656 = CIRCLE ( 'NONE', #19112, 14.00000000000000000 ) ;
#34657 = CARTESIAN_POINT ( 'NONE',  ( -35.50000000000000000, -113.8814751941377352, 10.49295109164313722 ) ) ;
#34658 = DIRECTION ( 'NONE',  ( -1.000000000000000000, 0.000000000000000000, 0.000000000000000000 ) ) ;
#34659 = ADVANCED_FACE ( 'NONE', ( #1693 ), #31921, .T. ) ;
#34660 = CARTESIAN_POINT ( 'NONE',  ( -36.00976557831293690, -114.9929510916434339, 14.11852773550420359 ) ) ;
#34661 = CARTESIAN_POINT ( 'NONE',  ( 0.000000000000000000, -1.000000000000001554, -22.00000000000000000 ) ) ;
#34662 = EDGE_CURVE ( 'NONE', #10377, #14262, #23348, .T. ) ;
#34663 = CIRCLE ( 'NONE', #26052, 15.49899999999998279 ) ;
#34664 = AXIS2_PLACEMENT_3D ( 'NONE', #1986, #13495, #10267 ) ;
#34665 = FACE_OUTER_BOUND ( 'NONE', #28581, .T. ) ;
#34666 = ORIENTED_EDGE ( 'NONE', *, *, #28274, .T. ) ;
#34667 = VECTOR ( 'NONE', #18998, 1000.000000000000227 ) ;
#34668 = CARTESIAN_POINT ( 'NONE',  ( -35.50040135968784938, -115.9929510916434481, 12.63896776382214071 ) ) ;
#34669 = CARTESIAN_POINT ( 'NONE',  ( 8.000000000000000000, -14.71414642875963708, 9.471478019455089381 ) ) ;
#34670 = FACE_OUTER_BOUND ( 'NONE', #31931, .T. ) ;
#34671 = CARTESIAN_POINT ( 'NONE',  ( 4.000000000000000000, 19.77827456857338007, 2.969824084036535528 ) ) ;
#34672 = FACE_OUTER_BOUND ( 'NONE', #26499, .T. ) ;
#34673 = ORIENTED_EDGE ( 'NONE', *, *, #11910, .T. ) ;
#34674 = DIRECTION ( 'NONE',  ( -1.783119874454246424E-31, -1.187911941725854497E-31, 1.000000000000000000 ) ) ;
#34675 = CARTESIAN_POINT ( 'NONE',  ( -21.15833593587365513, -11.98076211353319742, 83.49999999999992895 ) ) ;
#34676 = DIRECTION ( 'NONE',  ( -1.000000000000000000, 0.000000000000000000, 0.000000000000000000 ) ) ;
#34677 = LINE ( 'NONE', #7116, #22978 ) ;
#34678 = ORIENTED_EDGE ( 'NONE', *, *, #5652, .F. ) ;
#34679 = CARTESIAN_POINT ( 'NONE',  ( -37.74901162816869515, -114.6652019342044042, 6.566024454178448266 ) ) ;
#34680 = CARTESIAN_POINT ( 'NONE',  ( 8.000000000000007105, -13.61301047812905907, -3.268936481846313136 ) ) ;
#34681 = CARTESIAN_POINT ( 'NONE',  ( 0.000000000000000000, 0.000000000000000000, 0.000000000000000000 ) ) ;
#34682 = ORIENTED_EDGE ( 'NONE', *, *, #4265, .T. ) ;
#34683 = AXIS2_PLACEMENT_3D ( 'NONE', #7002, #17978, #1433 ) ;
#34684 = ORIENTED_EDGE ( 'NONE', *, *, #1380, .F. ) ;
#34685 = FILL_AREA_STYLE_COLOUR ( '', #11335 ) ;
#34686 = CARTESIAN_POINT ( 'NONE',  ( 7.999999999999992895, 37.91532898920923600, 28.61088654061652647 ) ) ;
#34687 = ORIENTED_EDGE ( 'NONE', *, *, #19558, .T. ) ;
#34688 = CARTESIAN_POINT ( 'NONE',  ( -37.05926240293131713, -111.0000000000000284, 8.121475545821549957 ) ) ;
#34689 = ORIENTED_EDGE ( 'NONE', *, *, #9303, .T. ) ;
#34690 = CARTESIAN_POINT ( 'NONE',  ( 0.000000000000000000, 0.000000000000000000, -49.10000000000000142 ) ) ;
#34691 = ORIENTED_EDGE ( 'NONE', *, *, #5498, .F. ) ;
#34692 = VERTEX_POINT ( 'NONE', #34101 ) ;
#34693 = CARTESIAN_POINT ( 'NONE',  ( 0.000000000000000000, -2.710505431213761085E-17, -20.99999999999999645 ) ) ;
#34694 = AXIS2_PLACEMENT_3D ( 'NONE', #20332, #23418, #18181 ) ;
#34695 = CIRCLE ( 'NONE', #34664, 19.99999999999998579 ) ;
#34696 = LINE ( 'NONE', #2425, #18307 ) ;
#34697 = CARTESIAN_POINT ( 'NONE',  ( 26.99999999999999645, 1.304248841091931221E-14, 0.000000000000000000 ) ) ;
#34698 = ORIENTED_EDGE ( 'NONE', *, *, #26628, .F. ) ;
#34699 = ORIENTED_EDGE ( 'NONE', *, *, #3170, .T. ) ;
#34700 = DIRECTION ( 'NONE',  ( 1.000000000000000000, 0.000000000000000000, 0.000000000000000000 ) ) ;
#34701 = DIRECTION ( 'NONE',  ( -1.174092375852890260E-15, 4.222049128630259891E-16, 1.000000000000000000 ) ) ;
#34702 = ORIENTED_EDGE ( 'NONE', *, *, #1333, .F. ) ;
#34703 = CARTESIAN_POINT ( 'NONE',  ( 0.000000000000000000, 0.000000000000000000, -32.00000000000000000 ) ) ;
#34704 = AXIS2_PLACEMENT_3D ( 'NONE', #319, #11311, #33276 ) ;
#34705 = FACE_OUTER_BOUND ( 'NONE', #13275, .T. ) ;
#34706 = CARTESIAN_POINT ( 'NONE',  ( -55.00000000000000000, 0.000000000000000000, 0.000000000000000000 ) ) ;
#34707 = ADVANCED_FACE ( 'NONE', ( #20206 ), #34641, .T. ) ;
#34708 = CARTESIAN_POINT ( 'NONE',  ( -34.50000000000000000, -115.9929510916434481, 12.26648026267477398 ) ) ;
#34709 = DIRECTION ( 'NONE',  ( 1.112002228190253556E-16, -6.938893903907203726E-17, -1.000000000000000000 ) ) ;
#34710 = CARTESIAN_POINT ( 'NONE',  ( -37.88768952767750164, -115.9754527089670262, 3.472274454178448266 ) ) ;
#34711 = CARTESIAN_POINT ( 'NONE',  ( -34.50000000000000000, -115.9895221797699065, 10.38535157366622563 ) ) ;
#34712 = CARTESIAN_POINT ( 'NONE',  ( 0.000000000000000000, -16.31134495048480559, -6.336799421339987859 ) ) ;
#34713 = CARTESIAN_POINT ( 'NONE',  ( 8.000000000000007105, -9.637487275700962641, -10.15474465512060398 ) ) ;
#34714 = DIRECTION ( 'NONE',  ( 0.000000000000000000, 0.000000000000000000, 1.000000000000000000 ) ) ;
#34715 = CARTESIAN_POINT ( 'NONE',  ( 8.000000000000000000, 0.000000000000000000, 0.000000000000000000 ) ) ;
#34716 = AXIS2_PLACEMENT_3D ( 'NONE', #2, #5069, #29724 ) ;
#34717 = VECTOR ( 'NONE', #11145, 1000.000000000000000 ) ;
#34718 = CARTESIAN_POINT ( 'NONE',  ( -49.99999999999999289, -25.98076211353320275, 90.99999999999994316 ) ) ;
#34719 = CARTESIAN_POINT ( 'NONE',  ( -34.50000000000001421, -41.45319397786874305, 92.20096189432315725 ) ) ;
#34720 = ORIENTED_EDGE ( 'NONE', *, *, #26022, .T. ) ;
#34721 = EDGE_CURVE ( 'NONE', #16923, #10424, #7257, .T. ) ;
#34722 = CARTESIAN_POINT ( 'NONE',  ( -33.97545270896703329, -115.1833782841879810, 8.590225545821549957 ) ) ;
#34723 = CARTESIAN_POINT ( 'NONE',  ( -34.49999999999998579, -25.98076211353320986, 84.99999999999994316 ) ) ;
#34724 = CARTESIAN_POINT ( 'NONE',  ( -35.50000000000000000, -113.0140978167138712, 0.7189676474015717078 ) ) ;
#34725 = VERTEX_POINT ( 'NONE', #28520 ) ;
#34726 = ORIENTED_EDGE ( 'NONE', *, *, #3781, .T. ) ;
#34727 = SURFACE_STYLE_USAGE ( .BOTH. , #23921 ) ;
#34728 = CARTESIAN_POINT ( 'NONE',  ( 7.999999999999992895, 39.78933988720149273, -24.98727647984960853 ) ) ;
#34729 = VERTEX_POINT ( 'NONE', #3870 ) ;
#34730 = EDGE_LOOP ( 'NONE', ( #500, #18621, #16972, #15447 ) ) ;
#34731 = ORIENTED_EDGE ( 'NONE', *, *, #10850, .F. ) ;
#34732 = AXIS2_PLACEMENT_3D ( 'NONE', #2973, #24920, #8696 ) ;
#34733 = CIRCLE ( 'NONE', #8375, 0.6000000000000028644 ) ;
#34734 = CARTESIAN_POINT ( 'NONE',  ( 0.000000000000000000, 11.46872990052381880, 45.56340405422447049 ) ) ;
#34735 = CARTESIAN_POINT ( 'NONE',  ( -39.02454729103295961, -113.2308352781851397, 9.340225545821551734 ) ) ;
#34736 = DIRECTION ( 'NONE',  ( 1.000000000000000000, 1.387778780781445922E-16, 0.000000000000000000 ) ) ;
#34737 = CARTESIAN_POINT ( 'NONE',  ( 7.999999999999992895, -9.744342220503712682, 46.48873837489796301 ) ) ;
#34738 = ORIENTED_EDGE ( 'NONE', *, *, #32543, .T. ) ;
#34739 = VERTEX_POINT ( 'NONE', #23100 ) ;
#34740 = CARTESIAN_POINT ( 'NONE',  ( -35.50000000000000711, -112.8356783780338759, 1.859636627348750348 ) ) ;
#34741 = CIRCLE ( 'NONE', #12320, 47.49900000000000944 ) ;
#34742 = CARTESIAN_POINT ( 'NONE',  ( 1.520000000000017559, 9.404460481120056357E-16, 5.016000000000010672 ) ) ;
#34743 = CARTESIAN_POINT ( 'NONE',  ( 8.000000000000000000, 9.508666619816654730, 19.83898331853691488 ) ) ;
#34744 = EDGE_LOOP ( 'NONE', ( #9164, #17925, #21347, #26006, #14646 ) ) ;
#34745 = DIRECTION ( 'NONE',  ( 0.000000000000000000, 0.000000000000000000, -1.000000000000000000 ) ) ;
#34746 = CYLINDRICAL_SURFACE ( 'NONE', #17285, 52.00000000000000711 ) ;
#34747 = ADVANCED_FACE ( 'NONE', ( #6727 ), #14829, .T. ) ;
#34748 = CARTESIAN_POINT ( 'NONE',  ( -34.50000000000000000, -114.9656200615856818, 10.26631071845107179 ) ) ;
#34749 = EDGE_CURVE ( 'NONE', #13787, #14743, #34279, .T. ) ;
#34750 = DIRECTION ( 'NONE',  ( -1.047965281155515106E-16, 6.938893903907203726E-17, 1.000000000000000000 ) ) ;
#34751 = CARTESIAN_POINT ( 'NONE',  ( -35.50640865667918433, -114.9929510916434339, 12.69998175888958514 ) ) ;
#34752 = DIRECTION ( 'NONE',  ( -1.000000000000000000, 0.000000000000000000, 0.000000000000000000 ) ) ;
#34753 = CARTESIAN_POINT ( 'NONE',  ( -34.50000000000000000, -114.0928965812550757, 9.511088712577292270 ) ) ;
#34754 = DIRECTION ( 'NONE',  ( 1.000000000000000000, 0.000000000000000000, 0.000000000000000000 ) ) ;
#34755 = CARTESIAN_POINT ( 'NONE',  ( -38.00000000000000711, -114.9929510916434339, 12.17846912687782179 ) ) ;
#34756 = DIRECTION ( 'NONE',  ( -1.000000000000000000, 0.000000000000000000, 0.000000000000000000 ) ) ;
#34757 = ORIENTED_EDGE ( 'NONE', *, *, #5293, .F. ) ;
#34758 = CARTESIAN_POINT ( 'NONE',  ( 7.999999999999992895, -5.871425383721172508, -51.66745943012291065 ) ) ;
#34759 = CARTESIAN_POINT ( 'NONE',  ( 0.000000000000000000, -12.96676809804157848, 13.60411018104313641 ) ) ;
#34760 = ORIENTED_EDGE ( 'NONE', *, *, #29153, .F. ) ;
#34761 = CARTESIAN_POINT ( 'NONE',  ( -37.62959469683911351, -114.9929510916434339, 13.10254527216511633 ) ) ;
#34762 = ORIENTED_EDGE ( 'NONE', *, *, #11219, .F. ) ;
#34763 = EDGE_CURVE ( 'NONE', #13129, #32244, #19880, .T. ) ;
#34764 = CARTESIAN_POINT ( 'NONE',  ( -35.54388159064475872, -112.6276912846090568, 4.316024454178448266 ) ) ;
#34765 = DIRECTION ( 'NONE',  ( 0.000000000000000000, 0.000000000000000000, 1.000000000000000000 ) ) ;
#34766 = VERTEX_POINT ( 'NONE', #1509 ) ;
#34767 = VERTEX_POINT ( 'NONE', #12491 ) ;
#34768 = CIRCLE ( 'NONE', #10052, 15.49899999999998279 ) ;
#34769 = AXIS2_PLACEMENT_3D ( 'NONE', #4167, #23591, #31157 ) ;
#34770 = CARTESIAN_POINT ( 'NONE',  ( -34.50000000000000000, -113.0140978167138712, 0.7502176474015694874 ) ) ;
#34771 = CARTESIAN_POINT ( 'NONE',  ( -34.97545270896703329, -113.2308352781851539, 8.909774454178450043 ) ) ;
#34772 = ORIENTED_EDGE ( 'NONE', *, *, #2185, .T. ) ;
#34773 = CARTESIAN_POINT ( 'NONE',  ( -39.97545270896702618, -112.6980969099493990, 2.347274454178448710 ) ) ;
#34774 = CIRCLE ( 'NONE', #6030, 4.000000000000000000 ) ;
#34775 = CARTESIAN_POINT ( 'NONE',  ( 46.00000000000000000, 0.000000000000000000, 0.000000000000000000 ) ) ;
#34776 = DIRECTION ( 'NONE',  ( 0.000000000000000000, 0.000000000000000000, 1.000000000000000000 ) ) ;
#34777 = ORIENTED_EDGE ( 'NONE', *, *, #7750, .T. ) ;
#34778 = VERTEX_POINT ( 'NONE', #34468 ) ;
#34779 = CARTESIAN_POINT ( 'NONE',  ( 70.00001200000002655, -22.08487140685993921, 86.04699153743705153 ) ) ;
#34780 = EDGE_CURVE ( 'NONE', #26182, #15733, #31424, .T. ) ;
#34781 =( NAMED_UNIT ( * ) SI_UNIT ( $, .STERADIAN. ) SOLID_ANGLE_UNIT ( ) );
#34782 = DIRECTION ( 'NONE',  ( 1.000000000000000000, 1.734723475976807094E-16, -0.000000000000000000 ) ) ;
#34783 = EDGE_LOOP ( 'NONE', ( #12012, #21960, #9352, #24462 ) ) ;
#34784 = ORIENTED_EDGE ( 'NONE', *, *, #15910, .T. ) ;
#34785 = CARTESIAN_POINT ( 'NONE',  ( -34.50000000000000000, -112.3697613878167658, -2.522673865603075605 ) ) ;
#34786 = EDGE_CURVE ( 'NONE', #17651, #1850, #29051, .T. ) ;
#34787 = FACE_OUTER_BOUND ( 'NONE', #34108, .T. ) ;
#34788 = ORIENTED_EDGE ( 'NONE', *, *, #25596, .F. ) ;
#34789 = VERTEX_POINT ( 'NONE', #5288 ) ;
#34790 = FACE_OUTER_BOUND ( 'NONE', #15174, .T. ) ;
#34791 = EDGE_CURVE ( 'NONE', #31889, #24508, #8415, .T. ) ;
#34792 = CARTESIAN_POINT ( 'NONE',  ( -34.50000000000000000, -113.9883062625807071, 10.50570311110699961 ) ) ;
#34793 = CIRCLE ( 'NONE', #15197, 7.199999999999993960 ) ;
#34794 = ADVANCED_FACE ( 'NONE', ( #29776 ), #24022, .F. ) ;
#34795 = FACE_OUTER_BOUND ( 'NONE', #14536, .T. ) ;
#34796 = EDGE_CURVE ( 'NONE', #3677, #8987, #21054, .T. ) ;
#34797 = CARTESIAN_POINT ( 'NONE',  ( -37.48437500000004263, -113.9929510916434339, 13.11852480586264846 ) ) ;
#34798 = VECTOR ( 'NONE', #20824, 1000.000000000000000 ) ;
#34799 = CARTESIAN_POINT ( 'NONE',  ( -37.50613590685470911, -115.9929510916434481, 13.11852378322482515 ) ) ;
#34800 = DIRECTION ( 'NONE',  ( 0.000000000000000000, -0.9048270524660235736, 0.4257792915650641663 ) ) ;
#34801 = AXIS2_PLACEMENT_3D ( 'NONE', #8235, #19212, #27861 ) ;
#34802 = FACE_OUTER_BOUND ( 'NONE', #15802, .T. ) ;
#34803 = ORIENTED_EDGE ( 'NONE', *, *, #29066, .F. ) ;
#34804 = EDGE_CURVE ( 'NONE', #6961, #11554, #13383, .T. ) ;
#34805 = FACE_OUTER_BOUND ( 'NONE', #14608, .T. ) ;
#34806 = DIRECTION ( 'NONE',  ( -1.000000000000000000, 0.000000000000000000, 0.000000000000000000 ) ) ;
#34807 = DIRECTION ( 'NONE',  ( 0.000000000000000000, 0.000000000000000000, 1.000000000000000000 ) ) ;
#34808 = ADVANCED_FACE ( 'NONE', ( #18238 ), #15883, .F. ) ;
#34809 = AXIS2_PLACEMENT_3D ( 'NONE', #2928, #24877, #13887 ) ;
#34810 = EDGE_LOOP ( 'NONE', ( #5606, #13558, #7325, #884 ) ) ;
#34811 = CARTESIAN_POINT ( 'NONE',  ( 7.999999999999992895, 0.000000000000000000, 0.000000000000000000 ) ) ;
#34812 = CARTESIAN_POINT ( 'NONE',  ( -35.50000000000000711, -112.0651520602111191, -0.9469505670458575608 ) ) ;
#34813 = CARTESIAN_POINT ( 'NONE',  ( 0.000000000000000000, 0.000000000000000000, 0.000000000000000000 ) ) ;
#34814 = CARTESIAN_POINT ( 'NONE',  ( 0.000000000000000000, 4.460989585141205360, -16.92083251265322730 ) ) ;
#34815 = DIRECTION ( 'NONE',  ( -1.000000000000000000, 0.000000000000000000, 0.000000000000000000 ) ) ;
#34816 = ORIENTED_EDGE ( 'NONE', *, *, #6815, .T. ) ;
#34817 = CIRCLE ( 'NONE', #25019, 22.00000000000000000 ) ;
#34818 = DIRECTION ( 'NONE',  ( -1.000000000000000000, -1.836970198721029934E-16, -0.000000000000000000 ) ) ;
#34819 = VECTOR ( 'NONE', #3018, 1000.000000000000000 ) ;
#34820 = CARTESIAN_POINT ( 'NONE',  ( -35.50000000000000000, -111.0140978167138570, -0.5622823525984297355 ) ) ;
#34821 = DIRECTION ( 'NONE',  ( 0.000000000000000000, 0.000000000000000000, 1.000000000000000000 ) ) ;
#34822 = ORIENTED_EDGE ( 'NONE', *, *, #31134, .T. ) ;
#34823 = VERTEX_POINT ( 'NONE', #16055 ) ;
#34824 = CARTESIAN_POINT ( 'NONE',  ( -36.25098837183129774, -113.3347980657956242, 8.816024454178446490 ) ) ;
#34825 = EDGE_CURVE ( 'NONE', #16586, #25119, #33736, .T. ) ;
#34826 = VECTOR ( 'NONE', #18632, 1000.000000000000000 ) ;
#34827 = DIRECTION ( 'NONE',  ( -1.000000000000000000, 0.000000000000000000, 0.000000000000000000 ) ) ;
#34828 = VERTEX_POINT ( 'NONE', #35183 ) ;
#34829 = ORIENTED_EDGE ( 'NONE', *, *, #14610, .T. ) ;
#34830 = CARTESIAN_POINT ( 'NONE',  ( -35.50000000000000000, -115.0304602784513293, -0.6247823525985405357 ) ) ;
#34831 = EDGE_CURVE ( 'NONE', #26771, #20546, #21642, .T. ) ;
#34832 = EDGE_CURVE ( 'NONE', #10144, #24757, #9003, .T. ) ;
#34833 = LINE ( 'NONE', #1893, #24092 ) ;
#34834 = DIRECTION ( 'NONE',  ( 1.000000000000000000, 0.000000000000000000, 0.000000000000000000 ) ) ;
#34835 = AXIS2_PLACEMENT_3D ( 'NONE', #2361, #3230, #19581 ) ;
#34836 = CARTESIAN_POINT ( 'NONE',  ( -37.56526046546250086, -114.9929510916434339, 13.11451721564129258 ) ) ;
#34837 = DIRECTION ( 'NONE',  ( -1.000000000000000000, 0.000000000000000000, 0.000000000000000000 ) ) ;
#34838 = EDGE_CURVE ( 'NONE', #28168, #5282, #32583, .T. ) ;
#34839 = EDGE_CURVE ( 'NONE', #17814, #4619, #9585, .T. ) ;
#34840 = CARTESIAN_POINT ( 'NONE',  ( -34.50000000000000000, -114.6807644833805000, -1.624782352598427959 ) ) ;
#34841 = CARTESIAN_POINT ( 'NONE',  ( -37.42187499999997158, -114.9929510916434339, 14.11852480586264846 ) ) ;
#34842 = DIRECTION ( 'NONE',  ( 0.000000000000000000, 0.000000000000000000, 1.000000000000000000 ) ) ;
#34843 = PRODUCT_DEFINITION_SHAPE ( 'NONE', 'NONE',  #35624 ) ;
#34844 = CIRCLE ( 'NONE', #19844, 4.000000000000000000 ) ;
#34845 = CARTESIAN_POINT ( 'NONE',  ( 0.000000000000000000, -2.710505431213761085E-17, 54.99999999999999289 ) ) ;
#34846 = ORIENTED_EDGE ( 'NONE', *, *, #4728, .T. ) ;
#34847 = CARTESIAN_POINT ( 'NONE',  ( -36.87500000000098765, -115.9929510916434481, 13.11852480586264846 ) ) ;
#34848 = CARTESIAN_POINT ( 'NONE',  ( -35.50000000000000711, -112.7549084230351752, -1.592823285203595285 ) ) ;
#34849 = LINE ( 'NONE', #10174, #14497 ) ;
#34850 = CARTESIAN_POINT ( 'NONE',  ( 0.000000000000000000, 0.000000000000000000, 0.000000000000000000 ) ) ;
#34851 = AXIS2_PLACEMENT_3D ( 'NONE', #15068, #17240, #17592 ) ;
#34852 = DIRECTION ( 'NONE',  ( 1.000000000000000000, -0.000000000000000000, 0.000000000000000000 ) ) ;
#34853 = EDGE_CURVE ( 'NONE', #16992, #31088, #20480, .T. ) ;
#34854 = ORIENTED_EDGE ( 'NONE', *, *, #32457, .F. ) ;
#34855 = CARTESIAN_POINT ( 'NONE',  ( 7.999999999999992895, 0.000000000000000000, 0.000000000000000000 ) ) ;
#34856 = CARTESIAN_POINT ( 'NONE',  ( 8.000000000000007105, 0.3151488735048668666, 11.27190672109269798 ) ) ;
#34857 = AXIS2_PLACEMENT_3D ( 'NONE', #6277, #19936, #28607 ) ;
#34858 = CARTESIAN_POINT ( 'NONE',  ( 0.000000000000000000, 27.43636312076375461, -38.14186064215119387 ) ) ;
#34859 = LINE ( 'NONE', #35048, #23616 ) ;
#34860 = ORIENTED_EDGE ( 'NONE', *, *, #4540, .T. ) ;
#34861 = CARTESIAN_POINT ( 'NONE',  ( -38.02454729103296671, -114.3549511594417396, 6.659774454178448266 ) ) ;
#34862 = AXIS2_PLACEMENT_3D ( 'NONE', #15929, #32865, #29822 ) ;
#34863 = CARTESIAN_POINT ( 'NONE',  ( -34.49999999999998579, -12.06135120645816272, 83.49999999999992895 ) ) ;
#34864 = DIRECTION ( 'NONE',  ( 1.000000000000000000, 0.000000000000000000, -0.000000000000000000 ) ) ;
#34865 = ORIENTED_EDGE ( 'NONE', *, *, #14158, .T. ) ;
#34866 = CIRCLE ( 'NONE', #31401, 20.00000000000000711 ) ;
#34867 = VERTEX_POINT ( 'NONE', #2591 ) ;
#34868 = CYLINDRICAL_SURFACE ( 'NONE', #3888, 4.800000000000000711 ) ;
#34869 = DIRECTION ( 'NONE',  ( 0.000000000000000000, 0.000000000000000000, 1.000000000000000000 ) ) ;
#34870 = VERTEX_POINT ( 'NONE', #21826 ) ;
#34871 = CARTESIAN_POINT ( 'NONE',  ( -37.88768952767750875, -112.0245472910329880, 3.527725545821551290 ) ) ;
#34872 = ORIENTED_EDGE ( 'NONE', *, *, #26507, .T. ) ;
#34873 = EDGE_CURVE ( 'NONE', #3282, #35360, #26904, .T. ) ;
#34874 = ITEM_DEFINED_TRANSFORMATION ( 'NONE', 'NONE', #13299,  #21307 ) ;
#34875 = ORIENTED_EDGE ( 'NONE', *, *, #21552, .T. ) ;
#34876 = ORIENTED_EDGE ( 'NONE', *, *, #30965, .T. ) ;
#34877 = FACE_OUTER_BOUND ( 'NONE', #9170, .T. ) ;
#34878 = ADVANCED_FACE ( 'NONE', ( #7785 ), #21649, .T. ) ;
#34879 = AXIS2_PLACEMENT_3D ( 'NONE', #16218, #18940, #24357 ) ;
#34880 = AXIS2_PLACEMENT_3D ( 'NONE', #2761, #10312, #35338 ) ;
#34881 = CIRCLE ( 'NONE', #24542, 8.000000000000000000 ) ;
#34882 = DIRECTION ( 'NONE',  ( 0.000000000000000000, 0.000000000000000000, -1.000000000000000000 ) ) ;
#34883 = EDGE_LOOP ( 'NONE', ( #2820, #9251, #23967, #27928 ) ) ;
#34884 = ORIENTED_EDGE ( 'NONE', *, *, #8111, .T. ) ;
#34885 = VECTOR ( 'NONE', #16456, 1000.000000000000000 ) ;
#34886 = FACE_OUTER_BOUND ( 'NONE', #4170, .T. ) ;
#34887 = CARTESIAN_POINT ( 'NONE',  ( -50.00000000000000000, -2.775557561562891351E-14, 110.0000000000000000 ) ) ;
#34888 = EDGE_CURVE ( 'NONE', #32375, #2787, #34311, .T. ) ;
#34889 = EDGE_LOOP ( 'NONE', ( #17257, #8744 ) ) ;
#34890 = CARTESIAN_POINT ( 'NONE',  ( -2.600000000000004530, -12.74999999999999822, -1.200000000000006617 ) ) ;
#34891 = ADVANCED_FACE ( 'NONE', ( #35007, #27250 ), #24365, .T. ) ;
#34892 = AXIS2_PLACEMENT_3D ( 'NONE', #20577, #28874, #15165 ) ;
#34893 = VECTOR ( 'NONE', #35424, 1000.000000000000000 ) ;
#34894 = CYLINDRICAL_SURFACE ( 'NONE', #33781, 17.49900000000000233 ) ;
#34895 = DIRECTION ( 'NONE',  ( 0.000000000000000000, 0.000000000000000000, -1.000000000000000000 ) ) ;
#34896 = CARTESIAN_POINT ( 'NONE',  ( -34.50000000000000000, -115.9929510916434481, 12.57451923796416260 ) ) ;
#34897 = DIRECTION ( 'NONE',  ( 0.000000000000000000, -0.8660254037844350439, -0.5000000000000061062 ) ) ;
#34898 = CARTESIAN_POINT ( 'NONE',  ( -37.76916472181487450, -111.9754527089670404, 8.534774454178448266 ) ) ;
#34899 = CARTESIAN_POINT ( 'NONE',  ( -34.50000000000000000, -115.9929510916434481, 10.51175824272318415 ) ) ;
#34900 = DIRECTION ( 'NONE',  ( 1.000000000000000000, -0.000000000000000000, -0.000000000000000000 ) ) ;
#34901 = FACE_OUTER_BOUND ( 'NONE', #6981, .T. ) ;
#34902 = VECTOR ( 'NONE', #20460, 1000.000000000000000 ) ;
#34903 = CARTESIAN_POINT ( 'NONE',  ( 8.000000000000000000, 16.92083251265334098, -4.460989585140788805 ) ) ;
#34904 = CARTESIAN_POINT ( 'NONE',  ( 7.999999999999992895, 6.109652351742432153, -46.58570277113502556 ) ) ;
#34905 = AXIS2_PLACEMENT_3D ( 'NONE', #12802, #15477, #10584 ) ;
#34906 = DIRECTION ( 'NONE',  ( 0.000000000000000000, 0.000000000000000000, 1.000000000000000000 ) ) ;
#34907 = DIRECTION ( 'NONE',  ( 0.000000000000000000, 0.000000000000000000, 1.000000000000000000 ) ) ;
#34908 = ORIENTED_EDGE ( 'NONE', *, *, #12730, .T. ) ;
#34909 = CARTESIAN_POINT ( 'NONE',  ( -36.11231047232249125, -115.9754527089670262, 5.777725545821551734 ) ) ;
#34910 = CARTESIAN_POINT ( 'NONE',  ( 8.000000000000000000, 0.000000000000000000, 0.000000000000000000 ) ) ;
#34911 = CIRCLE ( 'NONE', #2710, 7.199999999999991296 ) ;
#34912 = FACE_OUTER_BOUND ( 'NONE', #7318, .T. ) ;
#34913 = ORIENTED_EDGE ( 'NONE', *, *, #5358, .F. ) ;
#34914 = ORIENTED_EDGE ( 'NONE', *, *, #5262, .F. ) ;
#34915 = CARTESIAN_POINT ( 'NONE',  ( -34.49999999999998579, 9.432411113711806294, 117.4309090467819772 ) ) ;
#34916 = CARTESIAN_POINT ( 'NONE',  ( 0.000000000000000000, 36.06787431788677623, 37.45808914225502662 ) ) ;
#34917 = VERTEX_POINT ( 'NONE', #15524 ) ;
#34918 = AXIS2_PLACEMENT_3D ( 'NONE', #28022, #33411, #3712 ) ;
#34919 = ORIENTED_EDGE ( 'NONE', *, *, #4281, .T. ) ;
#34921 = EDGE_LOOP ( 'NONE', ( #7356, #22322, #13162, #19583 ) ) ;
#34920 = AXIS2_PLACEMENT_3D ( 'NONE', #31706, #4184, #19990 ) ;
#34922 = EDGE_CURVE ( 'NONE', #9746, #8132, #26544, .T. ) ;
#34923 = DIRECTION ( 'NONE',  ( 1.000000000000000000, 0.000000000000000000, 0.000000000000000000 ) ) ;
#34924 =( BOUNDED_CURVE ( )  B_SPLINE_CURVE ( 2, ( #9323, #6971, #28411, #854, #11836, #22817, #9142, #20280, #31635, #1227, #23180, #17945, #1585, #12564, #23537, #30934, #12742, #26973, #18486, #2481, #23718, #34710, #35078, #21523, #31815, #20812, #10569, #2314, #26430, #32000, #10401, #29845, #7336, #7854, #21357, #7676, #32522, #29129, #2136, #32352, #9847, #5186, #13283, #16125, #18660, #26786, #18311, #13113, #27141, #10034, #13451, #24259, #20997, #35247, #29657, #24431, #15419, #4999, #15955, #18844, #24094, #7151, #4480, #18125, #1761, #21187, #29310, #4658, #15588, #26610, #29487, #1945, #12920, #23905, #32179, #34898, #10221, #7506, #4826, #15767, #30539 ),
 .UNSPECIFIED., .F., .T. ) 
 B_SPLINE_CURVE_WITH_KNOTS ( ( 3, 2, 2, 2, 2, 2, 2, 2, 2, 2, 2, 2, 2, 2, 2, 2, 2, 2, 2, 2, 2, 2, 2, 2, 2, 2, 2, 2, 2, 2, 2, 2, 2, 2, 2, 2, 2, 2, 2, 2, 3 ),
 ( 0.000000000000000000, 0.02500000000000000139, 0.05000000000000000278, 0.07499999999999999722, 0.1000000000000000056, 0.1250000000000000000, 0.1499999999999999944, 0.1749999999999999889, 0.2000000000000000111, 0.2250000000000000056, 0.2500000000000000000, 0.2750000000000000222, 0.2999999999999999889, 0.3250000000000000111, 0.3499999999999999778, 0.3750000000000000000, 0.4000000000000000222, 0.4249999999999999889, 0.4500000000000000111, 0.4749999999999999778, 0.5000000000000000000, 0.5250000000000000222, 0.5500000000000000444, 0.5749999999999999556, 0.5999999999999999778, 0.6250000000000000000, 0.6500000000000000222, 0.6750000000000000444, 0.6999999999999999556, 0.7249999999999999778, 0.7500000000000000000, 0.7750000000000000222, 0.8000000000000000444, 0.8249999999999999556, 0.8499999999999999778, 0.8750000000000000000, 0.9000000000000000222, 0.9250000000000000444, 0.9499999999999999556, 0.9749999999999999778, 1.000000000000000000 ),
 .UNSPECIFIED. ) 
 CURVE ( )  GEOMETRIC_REPRESENTATION_ITEM ( )  RATIONAL_B_SPLINE_CURVE ( ( 1.000000000000000000, 0.9238795325112867385, 1.000000000000000000, 0.9238795325112867385, 1.000000000000000000, 0.9238795325112867385, 1.000000000000000000, 0.9238795325112867385, 1.000000000000000000, 0.9238795325112867385, 1.000000000000000000, 0.9238795325112867385, 1.000000000000000000, 0.9238795325112867385, 1.000000000000000000, 0.9238795325112867385, 1.000000000000000000, 0.9238795325112867385, 1.000000000000000000, 0.9238795325112867385, 1.000000000000000000, 0.9238795325112867385, 1.000000000000000000, 0.9238795325112867385, 1.000000000000000000, 0.9238795325112867385, 1.000000000000000000, 0.9238795325112867385, 1.000000000000000000, 0.9238795325112867385, 1.000000000000000000, 0.9238795325112867385, 1.000000000000000000, 0.9238795325112867385, 1.000000000000000000, 0.9238795325112867385, 1.000000000000000000, 0.9238795325112867385, 1.000000000000000000, 0.9238795325112867385, 1.000000000000000000, 0.9238795325112867385, 1.000000000000000000, 0.9238795325112867385, 1.000000000000000000, 0.9238795325112867385, 1.000000000000000000, 0.9238795325112867385, 1.000000000000000000, 0.9238795325112867385, 1.000000000000000000, 0.9238795325112867385, 1.000000000000000000, 0.9238795325112867385, 1.000000000000000000, 0.9238795325112867385, 1.000000000000000000, 0.9238795325112867385, 1.000000000000000000, 0.9238795325112867385, 1.000000000000000000, 0.9238795325112867385, 1.000000000000000000, 0.9238795325112867385, 1.000000000000000000, 0.9238795325112867385, 1.000000000000000000, 0.9238795325112867385, 1.000000000000000000, 0.9238795325112867385, 1.000000000000000000, 0.9238795325112867385, 1.000000000000000000, 0.9238795325112867385, 1.000000000000000000, 0.9238795325112867385, 1.000000000000000000, 0.9238795325112867385, 1.000000000000000000, 0.9238795325112867385, 1.000000000000000000 ) ) 
 REPRESENTATION_ITEM ( '' )  );
#34925 = CARTESIAN_POINT ( 'NONE',  ( -38.37230871539094323, -115.4561184093552413, 9.058975545821551734 ) ) ;
#34926 = CARTESIAN_POINT ( 'NONE',  ( -47.99999999999997868, -1.517883041479706208E-15, 70.00000000000000000 ) ) ;
#34927 = DIRECTION ( 'NONE',  ( -1.000000000000000000, -0.000000000000000000, -0.000000000000000000 ) ) ;
#34928 = VECTOR ( 'NONE', #6798, 1000.000000000000000 ) ;
#34929 = ORIENTED_EDGE ( 'NONE', *, *, #19666, .T. ) ;
#34930 = ORIENTED_EDGE ( 'NONE', *, *, #29694, .F. ) ;
#34931 = CARTESIAN_POINT ( 'NONE',  ( -35.50000000000000711, -112.4434344552011282, 1.705278471174987986 ) ) ;
#34932 = CIRCLE ( 'NONE', #6738, 22.00000000000000000 ) ;
#34933 = PLANE ( 'NONE',  #15658 ) ;
#34934 = DIRECTION ( 'NONE',  ( 0.000000000000000000, 0.000000000000000000, 1.000000000000000000 ) ) ;
#34935 = ORIENTED_EDGE ( 'NONE', *, *, #1867, .F. ) ;
#34936 = DIRECTION ( 'NONE',  ( 0.000000000000000000, 0.000000000000000000, 1.000000000000000000 ) ) ;
#34937 = AXIS2_PLACEMENT_3D ( 'NONE', #25102, #31385, #20374 ) ;
#34938 = CARTESIAN_POINT ( 'NONE',  ( -34.50000000000000000, -112.3465879560236687, 1.629585756119413364 ) ) ;
#34939 = AXIS2_PLACEMENT_3D ( 'NONE', #18561, #35146, #29563 ) ;
#34940 = CARTESIAN_POINT ( 'NONE',  ( -34.50000000000000000, -114.9929510916434339, 12.26648026267477221 ) ) ;
#34941 = CIRCLE ( 'NONE', #3887, 8.000000000000007105 ) ;
#34942 = CARTESIAN_POINT ( 'NONE',  ( 4.747884751462025044, -5.143694235356003119, -0.7999999999999951594 ) ) ;
#34943 = CIRCLE ( 'NONE', #11917, 14.00000000000000000 ) ;
#34944 = CARTESIAN_POINT ( 'NONE',  ( -37.54084996655477369, -114.9929510916434339, 13.11692036158760466 ) ) ;
#34945 = CARTESIAN_POINT ( 'NONE',  ( -90.00000000000002842, 0.000000000000000000, 6.938893903907228378E-15 ) ) ;
#34946 = CARTESIAN_POINT ( 'NONE',  ( -34.50000000000000000, -114.9902084924877954, 10.43071793783961176 ) ) ;
#34947 = CYLINDRICAL_SURFACE ( 'NONE', #27418, 8.000000000000003553 ) ;
#34948 = CIRCLE ( 'NONE', #27490, 20.00000000000000711 ) ;
#34949 = CARTESIAN_POINT ( 'NONE',  ( -38.00000068757622529, -114.9929510916434339, 12.61439929482944855 ) ) ;
#34950 = FACE_OUTER_BOUND ( 'NONE', #5689, .T. ) ;
#34951 = ORIENTED_EDGE ( 'NONE', *, *, #15018, .F. ) ;
#34952 = CARTESIAN_POINT ( 'NONE',  ( 0.000000000000000000, -13.55483219355736324, 11.06713717293235710 ) ) ;
#34953 = CARTESIAN_POINT ( 'NONE',  ( 0.000000000000000000, 0.000000000000000000, -44.50000000000000000 ) ) ;
#34954 = EDGE_LOOP ( 'NONE', ( #9570, #7128, #23893, #17067 ) ) ;
#34955 = CARTESIAN_POINT ( 'NONE',  ( -37.51635661748575501, -114.9929510916434339, 13.11827392651459157 ) ) ;
#34956 = ORIENTED_EDGE ( 'NONE', *, *, #28365, .T. ) ;
#34957 = CARTESIAN_POINT ( 'NONE',  ( -37.88768952767750164, -115.9754527089670262, 7.972274454178450043 ) ) ;
#34958 = MANIFOLD_SOLID_BREP ( 'Body', #10081 ) ;
#34959 = DIRECTION ( 'NONE',  ( -1.000000000000000000, 0.000000000000000000, 0.000000000000000000 ) ) ;
#34960 = VECTOR ( 'NONE', #13767, 1000.000000000000000 ) ;
#34961 = ORIENTED_EDGE ( 'NONE', *, *, #31271, .T. ) ;
#34962 = ORIENTED_EDGE ( 'NONE', *, *, #8556, .T. ) ;
#34963 = DIRECTION ( 'NONE',  ( -1.000000000000000000, 0.000000000000000000, 0.000000000000000000 ) ) ;
#34964 = EDGE_LOOP ( 'NONE', ( #13093, #31012 ) ) ;
#34965 = CARTESIAN_POINT ( 'NONE',  ( -34.92058450342251064, -116.1632251905417945, 1.691024454178448932 ) ) ;
#34966 = AXIS2_PLACEMENT_3D ( 'NONE', #25028, #16560, #27568 ) ;
#34967 = CIRCLE ( 'NONE', #3916, 7.199999999999994849 ) ;
#34968 = CARTESIAN_POINT ( 'NONE',  ( 7.999999999999992895, -30.93515269692089120, -36.04401931830286543 ) ) ;
#34969 = ADVANCED_FACE ( 'NONE', ( #11391 ), #5459, .F. ) ;
#34970 = CARTESIAN_POINT ( 'NONE',  ( -35.50000000000000711, -116.0140978167138712, 0.0002176474015577116276 ) ) ;
#34971 = EDGE_LOOP ( 'NONE', ( #3894, #336, #35501, #22445, #35572, #32777, #33392, #10464, #31420, #17640, #11173, #11119, #33001, #32825, #12550, #30698, #20977, #22119, #18564, #9262, #25385, #1160, #6374, #32435, #34556, #25176, #9967, #22298, #29779, #16462, #1039, #10806, #34854, #14219, #34289, #19993, #22311, #31182, #5814, #17247, #16905, #31653, #11334, #22058, #6448, #29024, #27485, #24025 ) ) ;
#34972 = ORIENTED_EDGE ( 'NONE', *, *, #23648, .T. ) ;
#34973 = DIRECTION ( 'NONE',  ( 0.000000000000000000, 0.000000000000000000, 1.000000000000000000 ) ) ;
#34974 = AXIS2_PLACEMENT_3D ( 'NONE', #21013, #12581, #12396 ) ;
#34975 = FACE_OUTER_BOUND ( 'NONE', #24488, .T. ) ;
#34976 = ORIENTED_EDGE ( 'NONE', *, *, #19406, .T. ) ;
#34977 = VERTEX_POINT ( 'NONE', #19479 ) ;
#34978 = CARTESIAN_POINT ( 'NONE',  ( -34.50000000000000000, -113.4307644833805142, -2.624782352598442614 ) ) ;
#34979 = EDGE_CURVE ( 'NONE', #30005, #10010, #50, .T. ) ;
#34980 = DIRECTION ( 'NONE',  ( 0.000000000000000000, 0.000000000000000000, -1.000000000000000000 ) ) ;
#34981 = ORIENTED_EDGE ( 'NONE', *, *, #1824, .T. ) ;
#34982 = ORIENTED_EDGE ( 'NONE', *, *, #2302, .T. ) ;
#34983 = CARTESIAN_POINT ( 'NONE',  ( 30.00000000000000355, -10.99999999999997868, 0.000000000000000000 ) ) ;
#34984 = VECTOR ( 'NONE', #26531, 1000.000000000000000 ) ;
#34985 = CARTESIAN_POINT ( 'NONE',  ( -34.50000000000000000, -113.9929510916435049, 10.50625754673586876 ) ) ;
#34986 = DIRECTION ( 'NONE',  ( 0.000000000000000000, 0.000000000000000000, 1.000000000000000000 ) ) ;
#34987 = CARTESIAN_POINT ( 'NONE',  ( 7.999999999999992895, 0.000000000000000000, 0.000000000000000000 ) ) ;
#34988 = CARTESIAN_POINT ( 'NONE',  ( -34.50000000000000000, -113.9883062625807071, 10.50570311110699961 ) ) ;
#34989 = AXIS2_PLACEMENT_3D ( 'NONE', #12942, #21382, #27167 ) ;
#34990 = CARTESIAN_POINT ( 'NONE',  ( -35.98364338251434447, -115.9929510916434481, 13.11827392651456314 ) ) ;
#34991 = DIRECTION ( 'NONE',  ( 0.000000000000000000, 0.000000000000000000, -1.000000000000000000 ) ) ;
#34992 = CIRCLE ( 'NONE', #3940, 20.00000000000000711 ) ;
#34993 = CARTESIAN_POINT ( 'NONE',  ( -4.000000000000000000, -2.710505431213761085E-17, 55.00000000000000000 ) ) ;
#34994 = EDGE_LOOP ( 'NONE', ( #27559, #17971 ) ) ;
#34995 = CARTESIAN_POINT ( 'NONE',  ( 0.000000000000000000, 46.19362259308845609, -8.585149169757999132 ) ) ;
#34996 = DIRECTION ( 'NONE',  ( 1.000000000000000000, 0.000000000000000000, 0.000000000000000000 ) ) ;
#34997 = CIRCLE ( 'NONE', #17142, 20.00000000000000355 ) ;
#34998 = CARTESIAN_POINT ( 'NONE',  ( 0.000000000000000000, 14.18878633068160866, 6.236773481718133283 ) ) ;
#34999 = EDGE_CURVE ( 'NONE', #11172, #33126, #30817, .T. ) ;
#35000 = VERTEX_POINT ( 'NONE', #13908 ) ;
#35001 = LINE ( 'NONE', #26713, #7248 ) ;
#35002 = CARTESIAN_POINT ( 'NONE',  ( -35.50000000000000711, -112.0140978167138712, 0.2502176474015765373 ) ) ;
#35003 = CARTESIAN_POINT ( 'NONE',  ( 46.00000000000000000, 0.000000000000000000, -8.000000000000000000 ) ) ;
#35004 = CARTESIAN_POINT ( 'NONE',  ( -35.50000000000000711, -114.9819937217110635, 10.35556074009299188 ) ) ;
#35005 = DIRECTION ( 'NONE',  ( 1.000000000000000000, -5.339440136655842133E-16, -1.047965281155519420E-16 ) ) ;
#35006 = VERTEX_POINT ( 'NONE', #22000 ) ;
#35007 = FACE_OUTER_BOUND ( 'NONE', #4344, .T. ) ;
#35008 = ADVANCED_FACE ( 'NONE', ( #11559 ), #16600, .T. ) ;
#35009 = CARTESIAN_POINT ( 'NONE',  ( -35.50000000000000000, -113.2224311500466030, -2.624782352598442614 ) ) ;
#35010 = VERTEX_POINT ( 'NONE', #22700 ) ;
#35011 = ORIENTED_EDGE ( 'NONE', *, *, #5919, .F. ) ;
#35012 = EDGE_CURVE ( 'NONE', #14425, #19237, #10745, .T. ) ;
#35013 = CARTESIAN_POINT ( 'NONE',  ( -36.33479806579561000, -114.7490116281687165, 7.691024454178450043 ) ) ;
#35014 = AXIS2_PLACEMENT_3D ( 'NONE', #15940, #35234, #32876 ) ;
#35015 = EDGE_CURVE ( 'NONE', #9304, #22471, #32997, .T. ) ;
#35016 = CIRCLE ( 'NONE', #12586, 20.00000000000000711 ) ;
#35017 = FILL_AREA_STYLE_COLOUR ( '', #2966 ) ;
#35018 = DIRECTION ( 'NONE',  ( 0.000000000000000000, 0.9672551082808337197, -0.2538061376417689030 ) ) ;
#35019 = VERTEX_POINT ( 'NONE', #30647 ) ;
#35020 = ORIENTED_EDGE ( 'NONE', *, *, #26376, .F. ) ;
#35021 = AXIS2_PLACEMENT_3D ( 'NONE', #16997, #22757, #16824 ) ;
#35022 = CARTESIAN_POINT ( 'NONE',  ( -34.50000000000000000, -113.0140978167156902, -0.6247823525984268489 ) ) ;
#35023 = ADVANCED_FACE ( 'NONE', ( #5982 ), #22528, .F. ) ;
#35024 = CARTESIAN_POINT ( 'NONE',  ( -90.00000000000002842, 0.000000000000000000, 6.938893903907228378E-15 ) ) ;
#35025 = EDGE_CURVE ( 'NONE', #23255, #27617, #1538, .T. ) ;
#35026 = DIRECTION ( 'NONE',  ( 0.000000000000000000, 0.000000000000000000, -1.000000000000000000 ) ) ;
#35027 = CARTESIAN_POINT ( 'NONE',  ( -38.00000000000000711, -114.9929510916434339, 12.56351784598954779 ) ) ;
#35028 = DIRECTION ( 'NONE',  ( -1.000000000000000000, 0.000000000000000000, 0.000000000000000000 ) ) ;
#35029 = FACE_OUTER_BOUND ( 'NONE', #1562, .T. ) ;
#35030 = CARTESIAN_POINT ( 'NONE',  ( -34.50000000000000000, -112.0157046079661995, -0.6902086197697556713 ) ) ;
#35031 = LINE ( 'NONE', #8292, #10785 ) ;
#35032 = CYLINDRICAL_SURFACE ( 'NONE', #24350, 19.99999999999998579 ) ;
#35033 = CARTESIAN_POINT ( 'NONE',  ( 0.000000000000000000, -8.931325931664709117, 16.53603053422203573 ) ) ;
#35034 = ORIENTED_EDGE ( 'NONE', *, *, #28165, .T. ) ;
#35035 = AXIS2_PLACEMENT_3D ( 'NONE', #2468, #24080, #29831 ) ;
#35036 = CARTESIAN_POINT ( 'NONE',  ( -35.50000000000000000, -115.9929510916434481, 12.26648026267477398 ) ) ;
#35037 = CARTESIAN_POINT ( 'NONE',  ( -35.50000000000000711, -116.0124910254613297, -0.6902086197697608894 ) ) ;
#35038 =( NAMED_UNIT ( * ) PLANE_ANGLE_UNIT ( ) SI_UNIT ( $, .RADIAN. ) );
#35039 = CARTESIAN_POINT ( 'NONE',  ( 4.000000000000000000, 4.627536653468036720E-16, -30.90000000000000568 ) ) ;
#35040 = EDGE_CURVE ( 'NONE', #34390, #25018, #10147, .T. ) ;
#35041 = CARTESIAN_POINT ( 'NONE',  ( 0.000000000000000000, -0.2227391519119825691, 46.98410307550729215 ) ) ;
#35042 = ORIENTED_EDGE ( 'NONE', *, *, #7263, .F. ) ;
#35043 = VECTOR ( 'NONE', #763, 1000.000000000000000 ) ;
#35044 = DIRECTION ( 'NONE',  ( -1.000000000000000000, 0.000000000000000000, 0.000000000000000000 ) ) ;
#35045 = DIRECTION ( 'NONE',  ( 1.000000000000000000, 0.000000000000000000, 0.000000000000000000 ) ) ;
#35046 = PRODUCT_RELATED_PRODUCT_CATEGORY ( 'part', '', ( #9806 ) ) ;
#35047 = CARTESIAN_POINT ( 'NONE',  ( 3.872983346207489852, 0.9999999999999522604, -32.00000000000000000 ) ) ;
#35048 = CARTESIAN_POINT ( 'NONE',  ( -55.00000000000000000, 19.99999999999998934, 120.0000000000000000 ) ) ;
#35049 = DIRECTION ( 'NONE',  ( 0.000000000000000000, 1.000000000000000000, 0.000000000000000000 ) ) ;
#35050 = CARTESIAN_POINT ( 'NONE',  ( 39.30000000000000426, 7.219292880973646134E-15, 0.000000000000000000 ) ) ;
#35051 = EDGE_LOOP ( 'NONE', ( #33753, #20387, #32329, #13690 ) ) ;
#35052 = ORIENTED_EDGE ( 'NONE', *, *, #11570, .F. ) ;
#35053 = LINE ( 'NONE', #10543, #21023 ) ;
#35054 = EDGE_CURVE ( 'NONE', #17302, #29440, #27436, .T. ) ;
#35055 = DIRECTION ( 'NONE',  ( 1.226634733346697831E-16, -0.7071067811865557884, 0.7071067811865392461 ) ) ;
#35056 = LINE ( 'NONE', #4631, #31211 ) ;
#35057 = ORIENTED_EDGE ( 'NONE', *, *, #20973, .F. ) ;
#35058 = ADVANCED_FACE ( 'NONE', ( #25430 ), #393, .T. ) ;
#35059 = CARTESIAN_POINT ( 'NONE',  ( -35.54388159064475872, -115.3723087153909432, 4.183975545821551734 ) ) ;
#35060 = EDGE_CURVE ( 'NONE', #35360, #18475, #4431, .T. ) ;
#35061 = ORIENTED_EDGE ( 'NONE', *, *, #7627, .F. ) ;
#35062 = VERTEX_POINT ( 'NONE', #1654 ) ;
#35063 = ORIENTED_EDGE ( 'NONE', *, *, #20733, .T. ) ;
#35064 = LINE ( 'NONE', #10386, #13747 ) ;
#35065 = AXIS2_PLACEMENT_3D ( 'NONE', #26419, #10025, #31991 ) ;
#35066 = EDGE_CURVE ( 'NONE', #25795, #3084, #29008, .T. ) ;
#35067 = CARTESIAN_POINT ( 'NONE',  ( 0.000000000000000000, -42.41764978026593269, -20.20639853260333751 ) ) ;
#35068 = ORIENTED_EDGE ( 'NONE', *, *, #7100, .T. ) ;
#35069 = ORIENTED_EDGE ( 'NONE', *, *, #12507, .F. ) ;
#35070 = AXIS2_PLACEMENT_3D ( 'NONE', #9399, #29219, #17680 ) ;
#35071 = FACE_OUTER_BOUND ( 'NONE', #13204, .T. ) ;
#35072 = CARTESIAN_POINT ( 'NONE',  ( -44.00000000000000000, 1.349783804395672066E-31, 0.000000000000000000 ) ) ;
#35073 = CIRCLE ( 'NONE', #1129, 4.800000000000000711 ) ;
#35074 = CARTESIAN_POINT ( 'NONE',  ( 8.000000000000007105, -5.679790370316031733, 7.613867765417587030 ) ) ;
#35075 = DIRECTION ( 'NONE',  ( 1.000000000000000000, -5.339440136655842133E-16, -1.047965281155519420E-16 ) ) ;
#35076 = DIRECTION ( 'NONE',  ( -1.000000000000000000, 0.000000000000000000, 0.000000000000000000 ) ) ;
#35077 = DIRECTION ( 'NONE',  ( 0.000000000000000000, 0.5877852522924682521, 0.8090169943749511150 ) ) ;
#35078 = CARTESIAN_POINT ( 'NONE',  ( -38.45611840935523418, -115.3723087153909432, 3.566024454178448710 ) ) ;
#35079 = CARTESIAN_POINT ( 'NONE',  ( -34.50000000000000000, -115.9929510916434481, 11.73841344789270202 ) ) ;
#35080 = DIRECTION ( 'NONE',  ( -1.000000000000000000, 0.000000000000000000, 0.000000000000000000 ) ) ;
#35081 = ADVANCED_FACE ( 'NONE', ( #1284 ), #26134, .T. ) ;
#35082 = CARTESIAN_POINT ( 'NONE',  ( 7.999999999999992895, -5.667686777402029641, 46.64153600743602368 ) ) ;
#35083 = CARTESIAN_POINT ( 'NONE',  ( 7.999999999999992895, -19.74581912682808493, -48.10512059033414545 ) ) ;
#35084 = LINE ( 'NONE', #10407, #285 ) ;
#35085 = EDGE_CURVE ( 'NONE', #13957, #33344, #14784, .T. ) ;
#35086 = DIRECTION ( 'NONE',  ( 0.000000000000000000, 0.000000000000000000, 1.000000000000000000 ) ) ;
#35087 = CARTESIAN_POINT ( 'NONE',  ( -9.999999999999994671, 0.000000000000000000, 0.000000000000000000 ) ) ;
#35088 = EDGE_LOOP ( 'NONE', ( #19631, #7705 ) ) ;
#35089 = CARTESIAN_POINT ( 'NONE',  ( -38.97545270896704039, -114.8876895276775087, 3.152725545821551290 ) ) ;
#35090 = CARTESIAN_POINT ( 'NONE',  ( 7.999999999999992895, -27.43636312076294814, -38.14186064215180494 ) ) ;
#35091 = DIRECTION ( 'NONE',  ( 0.000000000000000000, 0.9848077530122084644, -0.1736481776669276389 ) ) ;
#35092 = VERTEX_POINT ( 'NONE', #1115 ) ;
#35093 = AXIS2_PLACEMENT_3D ( 'NONE', #9716, #15453, #4329 ) ;
#35094 = ORIENTED_EDGE ( 'NONE', *, *, #2663, .T. ) ;
#35095 = CARTESIAN_POINT ( 'NONE',  ( 8.000000000000000000, -14.48509162075955281, -8.733917826871511636 ) ) ;
#35096 = PLANE ( 'NONE',  #24969 ) ;
#35097 = ORIENTED_EDGE ( 'NONE', *, *, #15664, .T. ) ;
#35098 = ADVANCED_FACE ( 'NONE', ( #9744, #33879, #28834, #26320, #34059 ), #14596, .T. ) ;
#35099 = ORIENTED_EDGE ( 'NONE', *, *, #26503, .T. ) ;
#35100 = ORIENTED_EDGE ( 'NONE', *, *, #2926, .T. ) ;
#35101 = ADVANCED_FACE ( 'NONE', ( #18011 ), #17663, .T. ) ;
#35102 = AXIS2_PLACEMENT_3D ( 'NONE', #15747, #29823, #24235 ) ;
#35103 = CYLINDRICAL_SURFACE ( 'NONE', #34989, 4.872650870659778199 ) ;
#35104 = CARTESIAN_POINT ( 'NONE',  ( -36.94073759706868287, -115.9999999999999858, 8.871475545821551734 ) ) ;
#35105 = DIRECTION ( 'NONE',  ( 1.000000000000000000, 0.000000000000000000, 0.000000000000000000 ) ) ;
#35106 = FACE_OUTER_BOUND ( 'NONE', #28526, .T. ) ;
#35107 = EDGE_LOOP ( 'NONE', ( #35477, #33513, #17110, #12909 ) ) ;
#35108 = VERTEX_POINT ( 'NONE', #20343 ) ;
#35109 = CARTESIAN_POINT ( 'NONE',  ( -35.50000000000000711, -112.7765286249690035, 1.847058736912741583 ) ) ;
#35110 = CARTESIAN_POINT ( 'NONE',  ( 2.000000000000001776, 0.000000000000000000, 0.000000000000000000 ) ) ;
#35111 = CIRCLE ( 'NONE', #21276, 3.799999999999999822 ) ;
#35112 = DIRECTION ( 'NONE',  ( -1.000000000000000000, 0.000000000000000000, 0.000000000000000000 ) ) ;
#35113 = ORIENTED_EDGE ( 'NONE', *, *, #16026, .F. ) ;
#35114 = DIRECTION ( 'NONE',  ( -1.000000000000000000, 0.000000000000000000, 0.000000000000000000 ) ) ;
#35115 = AXIS2_PLACEMENT_3D ( 'NONE', #30236, #5576, #27883 ) ;
#35116 = CARTESIAN_POINT ( 'NONE',  ( -34.50000000000000000, -112.0209493036498287, 0.9959249592223760050 ) ) ;
#35117 = CARTESIAN_POINT ( 'NONE',  ( -34.50000000000000000, -114.9928438774171582, 10.49113435197128652 ) ) ;
#35118 = DIRECTION ( 'NONE',  ( 0.000000000000000000, 0.9822872507286879440, 0.1873813145857285423 ) ) ;
#35119 = CARTESIAN_POINT ( 'NONE',  ( -35.87040530316090070, -114.9929510916434339, 13.10254527216545917 ) ) ;
#35120 = DIRECTION ( 'NONE',  ( -1.000000000000000000, 0.000000000000000000, 0.000000000000000000 ) ) ;
#35121 = AXIS2_PLACEMENT_3D ( 'NONE', #17914, #18631, #26207 ) ;
#35122 = CARTESIAN_POINT ( 'NONE',  ( -34.50000000000000000, -114.9929510916434339, 10.51175824272318415 ) ) ;
#35123 = CARTESIAN_POINT ( 'NONE',  ( 50.00000000000000711, 0.000000000000000000, 0.000000000000000000 ) ) ;
#35124 = EDGE_CURVE ( 'NONE', #35493, #10728, #4010, .T. ) ;
#35125 = FACE_OUTER_BOUND ( 'NONE', #5732, .T. ) ;
#35126 = DIRECTION ( 'NONE',  ( 0.000000000000000000, 0.000000000000000000, 1.000000000000000000 ) ) ;
#35127 = ORIENTED_EDGE ( 'NONE', *, *, #23354, .T. ) ;
#35128 = CARTESIAN_POINT ( 'NONE',  ( 3.413765605486549060, -14.29811891091956078, 0.000000000000000000 ) ) ;
#35129 = DIRECTION ( 'NONE',  ( 1.000000000000000000, 0.000000000000000000, 0.000000000000000000 ) ) ;
#35130 = EDGE_CURVE ( 'NONE', #4384, #22842, #34429, .T. ) ;
#35131 = EDGE_LOOP ( 'NONE', ( #21121, #35099, #12331, #30094 ) ) ;
#35132 = CARTESIAN_POINT ( 'NONE',  ( -36.03906250000000000, -114.9929510916434339, 13.11852480586264669 ) ) ;
#35133 = EDGE_LOOP ( 'NONE', ( #25696, #27483, #10211, #30981 ) ) ;
#35134 = CARTESIAN_POINT ( 'NONE',  ( -35.62769128460905677, -115.4561184093552413, 4.691024454178448266 ) ) ;
#35135 = CARTESIAN_POINT ( 'NONE',  ( 27.00000000000001066, 1.304248841091931379E-14, 0.000000000000000000 ) ) ;
#35136 = ORIENTED_EDGE ( 'NONE', *, *, #9751, .F. ) ;
#35137 = ORIENTED_EDGE ( 'NONE', *, *, #6239, .F. ) ;
#35138 = CARTESIAN_POINT ( 'NONE',  ( -3.799999999999999822, 4.653657836759942730E-16, -43.60000000000000142 ) ) ;
#35139 = AXIS2_PLACEMENT_3D ( 'NONE', #15630, #9402, #34077 ) ;
#35140 = VERTEX_POINT ( 'NONE', #9384 ) ;
#35141 = CARTESIAN_POINT ( 'NONE',  ( -38.30190309005061522, -116.9754527089670546, 4.972274454178449155 ) ) ;
#35142 = CARTESIAN_POINT ( 'NONE',  ( 4.000000000000003553, 51.93417535146742381, 2.615612846549361770 ) ) ;
#35143 = CARTESIAN_POINT ( 'NONE',  ( 8.000000000000000000, -15.46619997295643856, 1.007799283846635863 ) ) ;
#35144 = ORIENTED_EDGE ( 'NONE', *, *, #28355, .T. ) ;
#35145 = ORIENTED_EDGE ( 'NONE', *, *, #3395, .T. ) ;
#35146 = DIRECTION ( 'NONE',  ( -1.000000000000000000, 0.000000000000000000, 0.000000000000000000 ) ) ;
#35147 = AXIS2_PLACEMENT_3D ( 'NONE', #2053, #29942, #8500 ) ;
#35148 =( GEOMETRIC_REPRESENTATION_CONTEXT ( 3 ) GLOBAL_UNCERTAINTY_ASSIGNED_CONTEXT ( ( #30143 ) ) GLOBAL_UNIT_ASSIGNED_CONTEXT ( ( #17750, #1739, #6955 ) ) REPRESENTATION_CONTEXT ( 'NONE', 'WORKASPACE' ) );
#35149 = CIRCLE ( 'NONE', #32818, 7.199999999999994849 ) ;
#35150 =( NAMED_UNIT ( * ) SI_UNIT ( $, .STERADIAN. ) SOLID_ANGLE_UNIT ( ) );
#35151 = CARTESIAN_POINT ( 'NONE',  ( 8.000000000000000000, 0.000000000000000000, 0.000000000000000000 ) ) ;
#35152 = ORIENTED_EDGE ( 'NONE', *, *, #18986, .F. ) ;
#35153 = VERTEX_POINT ( 'NONE', #15122 ) ;
#35154 = CARTESIAN_POINT ( 'NONE',  ( -34.50000000000000000, -111.0301281775997353, -0.8858242144478579716 ) ) ;
#35155 = PRODUCT_DEFINITION_SHAPE ( 'NONE', 'NONE',  #35646 ) ;
#35156 = CARTESIAN_POINT ( 'NONE',  ( 7.999999999999992895, 37.91532898920923600, 28.61088654061652647 ) ) ;
#35157 = VERTEX_POINT ( 'NONE', #12633 ) ;
#35158 = CARTESIAN_POINT ( 'NONE',  ( -35.50000000000000711, -114.1021862393805577, 9.512197583835053649 ) ) ;
#35159 = CARTESIAN_POINT ( 'NONE',  ( -34.50000000000000000, -113.9929510916433912, 10.50625754673588474 ) ) ;
#35160 = FACE_OUTER_BOUND ( 'NONE', #12051, .T. ) ;
#35161 = CARTESIAN_POINT ( 'NONE',  ( 0.000000000000000000, 0.000000000000000000, 65.00000000000000000 ) ) ;
#35162 = CARTESIAN_POINT ( 'NONE',  ( -37.42187499999996447, -113.9929510916434339, 13.11852480586264846 ) ) ;
#35163 = CARTESIAN_POINT ( 'NONE',  ( -37.99599240977853754, -115.9929510916434481, 12.68378527132499656 ) ) ;
#35164 = DIRECTION ( 'NONE',  ( 0.000000000000000000, -0.3420201433256755963, 0.9396926207859057634 ) ) ;
#35165 = DIRECTION ( 'NONE',  ( -1.000000000000000000, 0.000000000000000000, 0.000000000000000000 ) ) ;
#35166 = EDGE_CURVE ( 'NONE', #33894, #27904, #8448, .T. ) ;
#35167 = EDGE_LOOP ( 'NONE', ( #15926, #9988, #9776, #16401 ) ) ;
#35168 = AXIS2_PLACEMENT_3D ( 'NONE', #29004, #20338, #12627 ) ;
#35169 = PRESENTATION_LAYER_ASSIGNMENT (  '', '', ( #20759 ) ) ;
#35170 = DIRECTION ( 'NONE',  ( -1.000000000000000000, 0.000000000000000000, 0.000000000000000000 ) ) ;
#35171 = CARTESIAN_POINT ( 'NONE',  ( 7.999999999999992895, 0.000000000000000000, 0.000000000000000000 ) ) ;
#35172 = CIRCLE ( 'NONE', #32278, 47.49900000000001654 ) ;
#35173 = CYLINDRICAL_SURFACE ( 'NONE', #23188, 3.999999999999998224 ) ;
#35174 = EDGE_LOOP ( 'NONE', ( #19975, #17334, #12666, #205 ) ) ;
#35175 = DIRECTION ( 'NONE',  ( 0.000000000000000000, 0.000000000000000000, -1.000000000000000000 ) ) ;
#35176 = APPLICATION_CONTEXT ( 'automotive_design' ) ;
#35177 = CARTESIAN_POINT ( 'NONE',  ( -35.50000000000000000, -113.0140978167134449, 0.8752176474011410523 ) ) ;
#35178 = DIRECTION ( 'NONE',  ( -1.000000000000000000, 0.000000000000000000, -0.000000000000000000 ) ) ;
#35179 = EDGE_CURVE ( 'NONE', #6533, #4002, #20168, .T. ) ;
#35180 = CARTESIAN_POINT ( 'NONE',  ( -35.50000000000000711, -114.9929510916434339, 10.85830208992344303 ) ) ;
#35181 = DIRECTION ( 'NONE',  ( 1.000000000000000000, 0.000000000000000000, -0.000000000000000000 ) ) ;
#35182 = ORIENTED_EDGE ( 'NONE', *, *, #30751, .F. ) ;
#35183 = CARTESIAN_POINT ( 'NONE',  ( 8.000000000000000000, 4.898587196589413815E-16, -4.000000000000000000 ) ) ;
#35184 = CARTESIAN_POINT ( 'NONE',  ( -35.50000000000000000, -111.0140978167138570, 0.6252176474015680441 ) ) ;
#35185 = ORIENTED_EDGE ( 'NONE', *, *, #26707, .T. ) ;
#35186 = VERTEX_POINT ( 'NONE', #1466 ) ;
#35187 = CIRCLE ( 'NONE', #28845, 8.000000000000001776 ) ;
#35188 = CARTESIAN_POINT ( 'NONE',  ( -37.97545270896701908, -113.5265240346955977, 6.847274454178448266 ) ) ;
#35189 = DIRECTION ( 'NONE',  ( -1.000000000000000000, 0.000000000000000000, 0.000000000000000000 ) ) ;
#35190 = ORIENTED_EDGE ( 'NONE', *, *, #14757, .F. ) ;
#35191 = ORIENTED_EDGE ( 'NONE', *, *, #8077, .T. ) ;
#35192 = CARTESIAN_POINT ( 'NONE',  ( -34.50000000000000000, -113.3474311500483935, -0.6247823525984269599 ) ) ;
#35193 = CIRCLE ( 'NONE', #3567, 20.00000000000000355 ) ;
#35194 =( GEOMETRIC_REPRESENTATION_CONTEXT ( 3 ) GLOBAL_UNCERTAINTY_ASSIGNED_CONTEXT ( ( #35268 ) ) GLOBAL_UNIT_ASSIGNED_CONTEXT ( ( #33699, #9037, #30654 ) ) REPRESENTATION_CONTEXT ( 'NONE', 'WORKASPACE' ) );
#35195 = CARTESIAN_POINT ( 'NONE',  ( 0.000000000000000000, 0.000000000000000000, -55.00000000000000000 ) ) ;
#35196 = DIRECTION ( 'NONE',  ( 1.000000000000000000, -0.000000000000000000, 0.000000000000000000 ) ) ;
#35197 = CARTESIAN_POINT ( 'NONE',  ( -38.00000000000000711, -114.9929510916434339, 12.57451923796417503 ) ) ;
#35198 = DIRECTION ( 'NONE',  ( 1.000000000000000000, -5.339440136655842133E-16, -1.047965281155519420E-16 ) ) ;
#35199 = CARTESIAN_POINT ( 'NONE',  ( 0.000000000000000000, 8.931325931664870765, -16.53603053422199665 ) ) ;
#35200 = CARTESIAN_POINT ( 'NONE',  ( -34.50000000000000000, -112.3995503592287690, -1.424448457485529618 ) ) ;
#35201 = CARTESIAN_POINT ( 'NONE',  ( -42.49999999999999289, -28.31857036507959791, 80.03062855292519373 ) ) ;
#35202 = AXIS2_PLACEMENT_3D ( 'NONE', #21575, #10448, #29707 ) ;
#35203 = EDGE_CURVE ( 'NONE', #19887, #34547, #31539, .T. ) ;
#35204 = EDGE_CURVE ( 'NONE', #15074, #4315, #13651, .T. ) ;
#35205 = CARTESIAN_POINT ( 'NONE',  ( 8.000000000000000000, -19.77827456857337651, 2.969824084036393863 ) ) ;
#35206 = ORIENTED_EDGE ( 'NONE', *, *, #13439, .F. ) ;
#35207 = CARTESIAN_POINT ( 'NONE',  ( -37.99359134332094357, -115.9929510916434481, 12.69998175888958514 ) ) ;
#35208 = LINE ( 'NONE', #30335, #28586 ) ;
#35209 = CYLINDRICAL_SURFACE ( 'NONE', #33484, 4.800000000000000711 ) ;
#35210 = DIRECTION ( 'NONE',  ( 0.000000000000000000, 0.000000000000000000, -1.000000000000000000 ) ) ;
#35211 = DIRECTION ( 'NONE',  ( -0.000000000000000000, 0.000000000000000000, -1.000000000000000000 ) ) ;
#35212 = ORIENTED_EDGE ( 'NONE', *, *, #23108, .T. ) ;
#35213 = LINE ( 'NONE', #24930, #33182 ) ;
#35214 = CARTESIAN_POINT ( 'NONE',  ( 8.000000000000000000, 0.000000000000000000, 0.000000000000000000 ) ) ;
#35215 = FACE_BOUND ( 'NONE', #24863, .T. ) ;
#35216 = DIRECTION ( 'NONE',  ( 0.000000000000000000, 0.000000000000000000, 1.000000000000000000 ) ) ;
#35217 = EDGE_CURVE ( 'NONE', #10666, #30768, #1568, .T. ) ;
#35218 = AXIS2_PLACEMENT_3D ( 'NONE', #14697, #15051, #25711 ) ;
#35219 = AXIS2_PLACEMENT_3D ( 'NONE', #26187, #4067, #30880 ) ;
#35220 = DIRECTION ( 'NONE',  ( 1.000000000000000000, -0.000000000000000000, -0.000000000000000000 ) ) ;
#35221 = DIRECTION ( 'NONE',  ( -1.000000000000000000, 0.000000000000000000, 0.000000000000000000 ) ) ;
#35222 = EDGE_CURVE ( 'NONE', #31834, #4628, #3822, .T. ) ;
#35223 = ORIENTED_EDGE ( 'NONE', *, *, #12263, .F. ) ;
#35224 = EDGE_LOOP ( 'NONE', ( #17309, #8791, #12072, #26492 ) ) ;
#35225 = DIRECTION ( 'NONE',  ( -1.000000000000000000, 0.000000000000000000, 0.000000000000000000 ) ) ;
#35226 = CARTESIAN_POINT ( 'NONE',  ( 8.000000000000000000, 0.000000000000000000, 0.000000000000000000 ) ) ;
#35227 = DIRECTION ( 'NONE',  ( 0.000000000000000000, 0.000000000000000000, 1.000000000000000000 ) ) ;
#35228 = ORIENTED_EDGE ( 'NONE', *, *, #13246, .T. ) ;
#35229 = CARTESIAN_POINT ( 'NONE',  ( -36.94073759706868287, -115.9999999999999858, 4.371475545821550845 ) ) ;
#35230 = ORIENTED_EDGE ( 'NONE', *, *, #17321, .F. ) ;
#35232 = ORIENTED_EDGE ( 'NONE', *, *, #30371, .F. ) ;
#35231 = VECTOR ( 'NONE', #23860, 1000.000000000000000 ) ;
#35233 = ORIENTED_EDGE ( 'NONE', *, *, #34342, .F. ) ;
#35234 = DIRECTION ( 'NONE',  ( -1.000000000000000000, 0.000000000000000000, 0.000000000000000000 ) ) ;
#35235 = EDGE_CURVE ( 'NONE', #33428, #33166, #6162, .T. ) ;
#35236 = CARTESIAN_POINT ( 'NONE',  ( 7.999999999999992895, 46.11014828289831513, 9.022736828081523441 ) ) ;
#35237 = VERTEX_POINT ( 'NONE', #20706 ) ;
#35238 = EDGE_LOOP ( 'NONE', ( #26840, #22651, #10287, #8971 ) ) ;
#35239 = DIRECTION ( 'NONE',  ( 0.000000000000000000, 0.000000000000000000, -1.000000000000000000 ) ) ;
#35240 = LINE ( 'NONE', #7669, #18353 ) ;
#35241 = CIRCLE ( 'NONE', #18544, 20.00000000000000711 ) ;
#35242 = DIRECTION ( 'NONE',  ( -5.339440136655842133E-16, -1.000000000000000000, 6.938893903907197563E-17 ) ) ;
#35243 = DIRECTION ( 'NONE',  ( 0.000000000000000000, 0.000000000000000000, -1.000000000000000000 ) ) ;
#35244 = DIRECTION ( 'NONE',  ( 0.000000000000000000, 0.9822872507286893873, -0.1873813145857213258 ) ) ;
#35245 = EDGE_CURVE ( 'NONE', #23477, #1839, #23972, .T. ) ;
#35246 = EDGE_CURVE ( 'NONE', #4579, #6999, #29207, .T. ) ;
#35247 = CARTESIAN_POINT ( 'NONE',  ( -37.88768952767750164, -115.9754527089670262, 6.472274454178449155 ) ) ;
#35248 = ADVANCED_FACE ( 'NONE', ( #4892, #24149 ), #23610, .F. ) ;
#35249 = CARTESIAN_POINT ( 'NONE',  ( -34.50000000000000000, -115.9929510916434481, 10.61627146648203990 ) ) ;
#35250 = DIRECTION ( 'NONE',  ( 1.110223024625156540E-16, 1.000000000000000000, 0.000000000000000000 ) ) ;
#35251 = DIRECTION ( 'NONE',  ( 0.000000000000000000, 0.000000000000000000, 1.000000000000000000 ) ) ;
#35252 = CIRCLE ( 'NONE', #4211, 47.49900000000000944 ) ;
#35253 = VECTOR ( 'NONE', #30712, 1000.000000000000000 ) ;
#35254 = CARTESIAN_POINT ( 'NONE',  ( 4.000000000000000000, 4.627536653468036720E-16, 54.99999999999999289 ) ) ;
#35255 = FACE_OUTER_BOUND ( 'NONE', #29560, .T. ) ;
#35256 = FACE_OUTER_BOUND ( 'NONE', #25804, .T. ) ;
#35257 = DIRECTION ( 'NONE',  ( 0.000000000000000000, 0.000000000000000000, 1.000000000000000000 ) ) ;
#35258 = ORIENTED_EDGE ( 'NONE', *, *, #20032, .F. ) ;
#35259 = EDGE_CURVE ( 'NONE', #34917, #35594, #29557, .T. ) ;
#35260 = CARTESIAN_POINT ( 'NONE',  ( -37.05926240293131713, -111.0000000000000284, 9.621475545821549957 ) ) ;
#35261 = FACE_OUTER_BOUND ( 'NONE', #11390, .T. ) ;
#35262 = CARTESIAN_POINT ( 'NONE',  ( 70.00000000000001421, -30.47068043442695284, 88.33026027086506815 ) ) ;
#35263 = CARTESIAN_POINT ( 'NONE',  ( -50.00000000000000000, 0.000000000000000000, 70.00000000000000000 ) ) ;
#35264 = EDGE_CURVE ( 'NONE', #21428, #22807, #2014, .T. ) ;
#35265 = VERTEX_POINT ( 'NONE', #34968 ) ;
#35266 = EDGE_LOOP ( 'NONE', ( #18481, #6698, #9374, #5413 ) ) ;
#35267 = EDGE_CURVE ( 'NONE', #10084, #5612, #29906, .T. ) ;
#35268 = UNCERTAINTY_MEASURE_WITH_UNIT (LENGTH_MEASURE( 1.000000000000000082E-05 ), #33699, 'distance_accuracy_value', 'NONE');
#35269 = DIRECTION ( 'NONE',  ( 0.000000000000000000, 0.000000000000000000, -1.000000000000000000 ) ) ;
#35270 = AXIS2_PLACEMENT_3D ( 'NONE', #20680, #34403, #6655 ) ;
#35271 = DIRECTION ( 'NONE',  ( 0.000000000000000000, 1.000000000000000000, 0.000000000000000000 ) ) ;
#35272 = ORIENTED_EDGE ( 'NONE', *, *, #14081, .T. ) ;
#35273 = ORIENTED_EDGE ( 'NONE', *, *, #34385, .F. ) ;
#35274 = DIRECTION ( 'NONE',  ( 0.000000000000000000, 2.423959199780483078E-15, -1.000000000000000000 ) ) ;
#35275 = CYLINDRICAL_SURFACE ( 'NONE', #1027, 7.199999999999993960 ) ;
#35276 = CARTESIAN_POINT ( 'NONE',  ( -45.00000000000000000, -25.98076211353322051, 84.99999999999995737 ) ) ;
#35277 = EDGE_CURVE ( 'NONE', #7529, #12629, #17637, .T. ) ;
#35278 = DIRECTION ( 'NONE',  ( -1.000000000000000000, -0.000000000000000000, -0.000000000000000000 ) ) ;
#35279 = ORIENTED_EDGE ( 'NONE', *, *, #16794, .T. ) ;
#35280 = ORIENTED_EDGE ( 'NONE', *, *, #4271, .T. ) ;
#35281 = CIRCLE ( 'NONE', #18580, 6.000000000000005329 ) ;
#35282 = CARTESIAN_POINT ( 'NONE',  ( -35.50000000000000711, -112.5103839485166333, -1.498529437127682495 ) ) ;
#35283 = EDGE_CURVE ( 'NONE', #7270, #13488, #29378, .T. ) ;
#35284 = DIRECTION ( 'NONE',  ( 0.000000000000000000, 1.000000000000000000, 0.000000000000000000 ) ) ;
#35285 = DIRECTION ( 'NONE',  ( -1.000000000000000000, 0.000000000000000000, 0.000000000000000000 ) ) ;
#35286 = EDGE_CURVE ( 'NONE', #34828, #27661, #27211, .T. ) ;
#35287 = ORIENTED_EDGE ( 'NONE', *, *, #27033, .T. ) ;
#35288 = LINE ( 'NONE', #10437, #8584 ) ;
#35289 = CARTESIAN_POINT ( 'NONE',  ( -34.50000000000000000, -114.6807644833805000, -1.624782352598427959 ) ) ;
#35290 = VECTOR ( 'NONE', #19627, 1000.000000000000000 ) ;
#35291 = CARTESIAN_POINT ( 'NONE',  ( -37.54906985245724371, -114.9929510916434339, 14.11777216781844579 ) ) ;
#35292 = CIRCLE ( 'NONE', #3648, 22.00000000000000000 ) ;
#35293 = DIRECTION ( 'NONE',  ( 0.000000000000000000, 0.000000000000000000, 1.000000000000000000 ) ) ;
#35294 = ADVANCED_FACE ( 'NONE', ( #32247 ), #32071, .T. ) ;
#35295 = CARTESIAN_POINT ( 'NONE',  ( -38.00000000000000711, -114.9929510916434339, 10.50625754673587231 ) ) ;
#35296 = DIRECTION ( 'NONE',  ( 1.000000000000000000, -5.339440136655842133E-16, -1.047965281155519420E-16 ) ) ;
#35297 = EDGE_CURVE ( 'NONE', #13349, #1026, #6721, .T. ) ;
#35298 = CARTESIAN_POINT ( 'NONE',  ( -34.50000000000000000, -114.9927795562974069, 10.48735431211914815 ) ) ;
#35299 = DIRECTION ( 'NONE',  ( 0.000000000000000000, 0.000000000000000000, 1.000000000000000000 ) ) ;
#35300 = CARTESIAN_POINT ( 'NONE',  ( -38.00000000000000711, -114.9929510916434339, 12.60752341388803721 ) ) ;
#35301 = CYLINDRICAL_SURFACE ( 'NONE', #1341, 20.00000000000000355 ) ;
#35302 = ORIENTED_EDGE ( 'NONE', *, *, #20991, .F. ) ;
#35303 = CARTESIAN_POINT ( 'NONE',  ( 7.999999999999992895, 0.000000000000000000, 0.000000000000000000 ) ) ;
#35304 = DIRECTION ( 'NONE',  ( 0.000000000000000000, 0.000000000000000000, 1.000000000000000000 ) ) ;
#35305 = VERTEX_POINT ( 'NONE', #18727 ) ;
#35306 = CARTESIAN_POINT ( 'NONE',  ( -37.89983305244309975, -114.9929510916434339, 12.92579853460519246 ) ) ;
#35307 = VERTEX_POINT ( 'NONE', #18556 ) ;
#35308 = CARTESIAN_POINT ( 'NONE',  ( -37.05926240293131713, -115.9999999999999858, 6.378524454178448266 ) ) ;
#35309 = DIRECTION ( 'NONE',  ( 1.541976423090495387E-16, -1.000000000000000000, 0.000000000000000000 ) ) ;
#35310 = EDGE_CURVE ( 'NONE', #26957, #8310, #31453, .T. ) ;
#35311 = EDGE_LOOP ( 'NONE', ( #26865, #21498 ) ) ;
#35312 = ORIENTED_EDGE ( 'NONE', *, *, #4036, .F. ) ;
#35313 = CARTESIAN_POINT ( 'NONE',  ( 4.000000000000003553, 10.15474465512060398, 9.637487275701170475 ) ) ;
#35314 = DIRECTION ( 'NONE',  ( -1.000000000000000000, 0.000000000000000000, 0.000000000000000000 ) ) ;
#35315 = ORIENTED_EDGE ( 'NONE', *, *, #17629, .T. ) ;
#35316 = CARTESIAN_POINT ( 'NONE',  ( -36.94073759706866156, -111.0000000000000284, 4.128524454178449155 ) ) ;
#35317 = CARTESIAN_POINT ( 'NONE',  ( -3.799999999999999822, 4.653657836759942730E-16, -55.00000000000000000 ) ) ;
#35318 = AXIS2_PLACEMENT_3D ( 'NONE', #13172, #18906, #10988 ) ;
#35319 = CARTESIAN_POINT ( 'NONE',  ( -35.50000000000000711, -116.0140978167138712, -0.3122823525984417259 ) ) ;
#35320 = CIRCLE ( 'NONE', #25540, 47.49900000000001654 ) ;
#35321 = ORIENTED_EDGE ( 'NONE', *, *, #21795, .F. ) ;
#35322 = ORIENTED_EDGE ( 'NONE', *, *, #29917, .F. ) ;
#35323 = DIRECTION ( 'NONE',  ( -1.000000000000000000, -0.000000000000000000, -0.000000000000000000 ) ) ;
#35324 = EDGE_CURVE ( 'NONE', #3820, #9927, #4642, .T. ) ;
#35325 = CARTESIAN_POINT ( 'NONE',  ( 0.000000000000000000, -11.11653975335780942, -12.74840161668743299 ) ) ;
#35326 = EDGE_LOOP ( 'NONE', ( #8644, #21644, #20847, #26092 ) ) ;
#35327 = ORIENTED_EDGE ( 'NONE', *, *, #26740, .T. ) ;
#35328 = CARTESIAN_POINT ( 'NONE',  ( -34.50000000000000000, -111.0140978167138570, 0.3752176474015639918 ) ) ;
#35329 = ADVANCED_FACE ( 'NONE', ( #12812 ), #18909, .T. ) ;
#35330 = DIRECTION ( 'NONE',  ( 0.000000000000000000, -1.000000000000000000, 0.000000000000000000 ) ) ;
#35331 = ORIENTED_EDGE ( 'NONE', *, *, #30394, .F. ) ;
#35332 = CARTESIAN_POINT ( 'NONE',  ( -35.50000000000000711, -114.9656200615856818, 10.26631071845107179 ) ) ;
#35333 = CARTESIAN_POINT ( 'NONE',  ( -34.50000000000000000, -113.9929510916434339, 10.50625754673588474 ) ) ;
#35334 = CYLINDRICAL_SURFACE ( 'NONE', #1075, 7.199999999999993960 ) ;
#35335 = DIRECTION ( 'NONE',  ( -1.783119874454246424E-31, -1.187911941725854497E-31, 1.000000000000000000 ) ) ;
#35336 = CARTESIAN_POINT ( 'NONE',  ( -34.50000000000000000, -113.9000545103886850, 10.49516883415891577 ) ) ;
#35337 = CARTESIAN_POINT ( 'NONE',  ( -37.46093750000000711, -115.9929510916434481, 13.11852480586264846 ) ) ;
#35338 = DIRECTION ( 'NONE',  ( 0.000000000000000000, 0.000000000000000000, 1.000000000000000000 ) ) ;
#35340 = AXIS2_PLACEMENT_3D ( 'NONE', #29675, #29861, #7876 ) ;
#35339 = DIRECTION ( 'NONE',  ( 0.000000000000000000, 0.000000000000000000, 1.000000000000000000 ) ) ;
#35341 = CIRCLE ( 'NONE', #18066, 52.00000000000000711 ) ;
#35342 = ORIENTED_EDGE ( 'NONE', *, *, #9673, .T. ) ;
#35343 = CYLINDRICAL_SURFACE ( 'NONE', #7918, 8.000000000000001776 ) ;
#35344 = DIRECTION ( 'NONE',  ( 0.000000000000000000, 0.000000000000000000, 1.000000000000000000 ) ) ;
#35345 = DIRECTION ( 'NONE',  ( -1.000000000000000000, -0.000000000000000000, 0.000000000000000000 ) ) ;
#35346 = VERTEX_POINT ( 'NONE', #13347 ) ;
#35347 = CARTESIAN_POINT ( 'NONE',  ( -90.00000000000002842, -3.455569164145799535E-16, -4.980000000000010196 ) ) ;
#35348 = CARTESIAN_POINT ( 'NONE',  ( -35.50000000000000711, -116.0140978167138712, 0.6252176474015648244 ) ) ;
#35349 = CARTESIAN_POINT ( 'NONE',  ( 0.000000000000000000, -0.3212489022566501484, 16.91141623315869680 ) ) ;
#35350 = CARTESIAN_POINT ( 'NONE',  ( -35.50000000000000711, -114.9929510916434339, 10.94631322572069365 ) ) ;
#35351 = DIRECTION ( 'NONE',  ( 0.000000000000000000, 0.5000000000000009992, -0.8660254037844380415 ) ) ;
#35352 = ORIENTED_EDGE ( 'NONE', *, *, #16067, .T. ) ;
#35353 = CARTESIAN_POINT ( 'NONE',  ( -1.599999999999990319, 0.000000000000000000, 0.000000000000000000 ) ) ;
#35354 = CARTESIAN_POINT ( 'NONE',  ( -35.50000000000000000, -111.0140978167138570, -0.4997823525984338988 ) ) ;
#35355 = ORIENTED_EDGE ( 'NONE', *, *, #7774, .F. ) ;
#35356 = VERTEX_POINT ( 'NONE', #2376 ) ;
#35357 = CARTESIAN_POINT ( 'NONE',  ( -35.00000000000000000, -114.0592624029313242, 3.003524454178448710 ) ) ;
#35358 = SHAPE_REPRESENTATION_RELATIONSHIP ( 'NONE' , 'NONE' ,  #11863, #1766 ) ;
#35359 = CARTESIAN_POINT ( 'NONE',  ( 0.000000000000000000, 0.000000000000000000, 0.000000000000000000 ) ) ;
#35360 = VERTEX_POINT ( 'NONE', #35317 ) ;
#35361 = ORIENTED_EDGE ( 'NONE', *, *, #26258, .T. ) ;
#35362 = CARTESIAN_POINT ( 'NONE',  ( -34.50000000000000000, -113.0140978167138712, 0.8752176474015154195 ) ) ;
#35363 = DIRECTION ( 'NONE',  ( 0.000000000000000000, 0.000000000000000000, -1.000000000000000000 ) ) ;
#35364 = AXIS2_PLACEMENT_3D ( 'NONE', #25163, #25340, #32908 ) ;
#35365 = ADVANCED_FACE ( 'NONE', ( #10639 ), #21595, .F. ) ;
#35366 = AXIS2_PLACEMENT_3D ( 'NONE', #1593, #25906, #28951 ) ;
#35367 = CARTESIAN_POINT ( 'NONE',  ( 0.000000000000000000, 0.000000000000000000, 65.00000000000000000 ) ) ;
#35368 = AXIS2_PLACEMENT_3D ( 'NONE', #14326, #14863, #14674 ) ;
#35369 = DIRECTION ( 'NONE',  ( 0.000000000000000000, 0.2486898871648482723, 0.9685831611286328524 ) ) ;
#35370 = CARTESIAN_POINT ( 'NONE',  ( -38.00000000000000711, -114.9929510916434339, 12.50851088611646311 ) ) ;
#35371 = FACE_OUTER_BOUND ( 'NONE', #29291, .T. ) ;
#35372 = DIRECTION ( 'NONE',  ( 0.000000000000000000, 0.7705132427757861446, 0.6374239897486934092 ) ) ;
#35373 = CARTESIAN_POINT ( 'NONE',  ( -34.50000000000000000, -112.0140978167138712, -0.4997823525984337878 ) ) ;
#35374 = AXIS2_PLACEMENT_3D ( 'NONE', #14233, #22159, #13725 ) ;
#35375 = DIRECTION ( 'NONE',  ( 0.000000000000000000, -6.994405055138476738E-15, 1.000000000000000000 ) ) ;
#35376 = PLANE ( 'NONE',  #31286 ) ;
#35377 = ORIENTED_EDGE ( 'NONE', *, *, #15007, .T. ) ;
#35378 = CARTESIAN_POINT ( 'NONE',  ( -37.99994980024369085, -115.9929510916434481, 12.62670525340494621 ) ) ;
#35379 = CARTESIAN_POINT ( 'NONE',  ( -49.99999999999999289, -25.98076211353320275, 84.99999999999992895 ) ) ;
#35380 = DIRECTION ( 'NONE',  ( 1.000000000000000000, 0.000000000000000000, 0.000000000000000000 ) ) ;
#35381 = DIRECTION ( 'NONE',  ( -1.000000000000000000, -0.000000000000000000, 0.000000000000000000 ) ) ;
#35382 = CARTESIAN_POINT ( 'NONE',  ( 8.000000000000000000, 0.000000000000000000, 0.000000000000000000 ) ) ;
#35383 = ORIENTED_EDGE ( 'NONE', *, *, #33233, .T. ) ;
#35384 = LINE ( 'NONE', #7821, #21651 ) ;
#35385 = DIRECTION ( 'NONE',  ( -1.000000000000000000, 0.000000000000000000, 0.000000000000000000 ) ) ;
#35386 = AXIS2_PLACEMENT_3D ( 'NONE', #23678, #28905, #26200 ) ;
#35387 = AXIS2_PLACEMENT_3D ( 'NONE', #19705, #22594, #14147 ) ;
#35388 = CARTESIAN_POINT ( 'NONE',  ( 8.000000000000000000, 0.000000000000000000, 0.000000000000000000 ) ) ;
#35389 = CYLINDRICAL_SURFACE ( 'NONE', #28187, 45.00000000000000000 ) ;
#35390 = DIRECTION ( 'NONE',  ( 0.000000000000000000, -0.2486898871648622611, 0.9685831611286292997 ) ) ;
#35391 = DIRECTION ( 'NONE',  ( 0.000000000000000000, 0.000000000000000000, -1.000000000000000000 ) ) ;
#35392 = AXIS2_PLACEMENT_3D ( 'NONE', #3721, #822, #33592 ) ;
#35393 = ORIENTED_EDGE ( 'NONE', *, *, #29960, .T. ) ;
#35394 = ORIENTED_EDGE ( 'NONE', *, *, #2711, .T. ) ;
#35395 = AXIS2_PLACEMENT_3D ( 'NONE', #25170, #8413, #493 ) ;
#35396 = DIRECTION ( 'NONE',  ( -1.000000000000000000, 1.502314598737152375E-16, 8.673617379884158732E-17 ) ) ;
#35397 = DIRECTION ( 'NONE',  ( -1.000000000000000000, -0.000000000000000000, -0.000000000000000000 ) ) ;
#35398 = CYLINDRICAL_SURFACE ( 'NONE', #11100, 7.199999999999994849 ) ;
#35399 = ORIENTED_EDGE ( 'NONE', *, *, #25362, .F. ) ;
#35400 = CARTESIAN_POINT ( 'NONE',  ( -38.45611840935523418, -112.6276912846090568, 4.933975545821551734 ) ) ;
#35401 = VERTEX_POINT ( 'NONE', #9920 ) ;
#35402 = CIRCLE ( 'NONE', #26188, 8.000000000000000000 ) ;
#35403 = VERTEX_POINT ( 'NONE', #7930 ) ;
#35404 = ORIENTED_EDGE ( 'NONE', *, *, #4363, .T. ) ;
#35405 = CARTESIAN_POINT ( 'NONE',  ( -42.49999999999999289, -17.72201855431906736, 96.30456345124113682 ) ) ;
#35406 = EDGE_CURVE ( 'NONE', #23627, #7912, #32226, .T. ) ;
#35407 = EDGE_CURVE ( 'NONE', #10004, #6879, #8643, .T. ) ;
#35408 = DIRECTION ( 'NONE',  ( 1.000000000000000000, -0.000000000000000000, 0.000000000000000000 ) ) ;
#35409 = ORIENTED_EDGE ( 'NONE', *, *, #16384, .T. ) ;
#35410 = ORIENTED_EDGE ( 'NONE', *, *, #7425, .F. ) ;
#35411 = AXIS2_PLACEMENT_3D ( 'NONE', #10363, #21323, #5152 ) ;
#35412 = DIRECTION ( 'NONE',  ( 0.000000000000000000, 1.000000000000000000, 3.497202527569241525E-15 ) ) ;
#35413 = CARTESIAN_POINT ( 'NONE',  ( 7.999999999999992895, -31.08872492059928305, -41.68322423723133596 ) ) ;
#35414 = EDGE_CURVE ( 'NONE', #26625, #34828, #1178, .T. ) ;
#35415 = LINE ( 'NONE', #10744, #35522 ) ;
#35416 = CIRCLE ( 'NONE', #29083, 8.000000000000007105 ) ;
#35417 = DIRECTION ( 'NONE',  ( -1.000000000000000000, 0.000000000000000000, -0.000000000000000000 ) ) ;
#35418 = DIRECTION ( 'NONE',  ( -1.000000000000000000, 0.000000000000000000, 0.000000000000000000 ) ) ;
#35419 = DIRECTION ( 'NONE',  ( 1.000000000000000000, -0.000000000000000000, -0.000000000000000000 ) ) ;
#35420 = CARTESIAN_POINT ( 'NONE',  ( -37.62254989966453422, -115.9929510916434481, 14.11371147303758278 ) ) ;
#35421 = CARTESIAN_POINT ( 'NONE',  ( 8.000000000000000000, 16.71027810728552154, -2.620268201066000113 ) ) ;
#35422 = DIRECTION ( 'NONE',  ( -1.000000000000000000, 0.000000000000000000, 0.000000000000000000 ) ) ;
#35423 = AXIS2_PLACEMENT_3D ( 'NONE', #12029, #12211, #860 ) ;
#35424 = DIRECTION ( 'NONE',  ( -1.000000000000000000, 0.000000000000000000, 0.000000000000000000 ) ) ;
#35425 = DIRECTION ( 'NONE',  ( -1.000000000000000000, 0.000000000000000000, 0.000000000000000000 ) ) ;
#35426 = CARTESIAN_POINT ( 'NONE',  ( 8.000000000000000000, -8.128228055638974325, 16.94522934049209795 ) ) ;
#35427 = SURFACE_STYLE_FILL_AREA ( #13810 ) ;
#35428 = ORIENTED_EDGE ( 'NONE', *, *, #10154, .T. ) ;
#35429 = CARTESIAN_POINT ( 'NONE',  ( -36.94073759706868287, -115.9999999999999858, 4.371475545821550845 ) ) ;
#35430 = CARTESIAN_POINT ( 'NONE',  ( 50.00005079999998969, 0.000000000000000000, 0.000000000000000000 ) ) ;
#35431 = FACE_OUTER_BOUND ( 'NONE', #6673, .T. ) ;
#35432 = EDGE_CURVE ( 'NONE', #16603, #31617, #28573, .T. ) ;
#35433 = FACE_OUTER_BOUND ( 'NONE', #17104, .T. ) ;
#35434 = ORIENTED_EDGE ( 'NONE', *, *, #18796, .F. ) ;
#35435 = ORIENTED_EDGE ( 'NONE', *, *, #35012, .F. ) ;
#35436 =( NAMED_UNIT ( * ) PLANE_ANGLE_UNIT ( ) SI_UNIT ( $, .RADIAN. ) );
#35437 = CIRCLE ( 'NONE', #6095, 20.00000000000000711 ) ;
#35438 = DIRECTION ( 'NONE',  ( -1.000000000000000000, -0.000000000000000000, 0.000000000000000000 ) ) ;
#35439 = ORIENTED_EDGE ( 'NONE', *, *, #12848, .F. ) ;
#35440 = ORIENTED_EDGE ( 'NONE', *, *, #4246, .F. ) ;
#35441 =( GEOMETRIC_REPRESENTATION_CONTEXT ( 3 ) GLOBAL_UNCERTAINTY_ASSIGNED_CONTEXT ( ( #1006 ) ) GLOBAL_UNIT_ASSIGNED_CONTEXT ( ( #14051, #22676, #11017 ) ) REPRESENTATION_CONTEXT ( 'NONE', 'WORKASPACE' ) );
#35442 = AXIS2_PLACEMENT_3D ( 'NONE', #3418, #27889, #22120 ) ;
#35443 = AXIS2_PLACEMENT_3D ( 'NONE', #7828, #35221, #10538 ) ;
#35444 = EDGE_CURVE ( 'NONE', #11499, #17618, #28780, .T. ) ;
#35445 = DIRECTION ( 'NONE',  ( 0.000000000000000000, -0.7705132427757815927, -0.6374239897486989603 ) ) ;
#35446 = ADVANCED_FACE ( 'NONE', ( #8098 ), #25212, .T. ) ;
#35447 = DIRECTION ( 'NONE',  ( -1.000000000000000000, 0.000000000000000000, 0.000000000000000000 ) ) ;
#35448 = ADVANCED_FACE ( 'NONE', ( #24501 ), #30775, .T. ) ;
#35449 = AXIS2_PLACEMENT_3D ( 'NONE', #1327, #1157, #31747 ) ;
#35450 = SHAPE_DEFINITION_REPRESENTATION ( #25315, #2005 ) ;
#35451 = DIRECTION ( 'NONE',  ( -1.000000000000000000, 0.000000000000000000, 0.000000000000000000 ) ) ;
#35452 = ORIENTED_EDGE ( 'NONE', *, *, #14010, .F. ) ;
#35453 = VERTEX_POINT ( 'NONE', #14210 ) ;
#35454 = CARTESIAN_POINT ( 'NONE',  ( -55.00000000000000000, -2.726571689596996976E-14, 114.0000000000000000 ) ) ;
#35455 = EDGE_CURVE ( 'NONE', #28345, #1645, #2918, .T. ) ;
#35456 = CARTESIAN_POINT ( 'NONE',  ( 50.00005079999999680, 0.000000000000000000, 0.000000000000000000 ) ) ;
#35457 = EDGE_LOOP ( 'NONE', ( #26956, #15164, #21701, #1638 ) ) ;
#35458 = CARTESIAN_POINT ( 'NONE',  ( 7.999999999999992895, 24.47917365150010482, -45.87777302070911389 ) ) ;
#35459 = EDGE_CURVE ( 'NONE', #7443, #1605, #30505, .T. ) ;
#35460 = CARTESIAN_POINT ( 'NONE',  ( -34.50000000000000000, -113.8474311500459777, -1.624782352598427959 ) ) ;
#35461 = CARTESIAN_POINT ( 'NONE',  ( -38.98797722933582577, -114.9929510916434339, 12.81430620224974959 ) ) ;
#35462 = AXIS2_PLACEMENT_3D ( 'NONE', #14412, #17650, #17468 ) ;
#35463 = CARTESIAN_POINT ( 'NONE',  ( -4.000000000000000000, -2.710505431213761085E-17, 54.99999999999999289 ) ) ;
#35464 = CARTESIAN_POINT ( 'NONE',  ( -35.50000000000000000, -113.9000545103886850, 10.49516883415891577 ) ) ;
#35465 = CARTESIAN_POINT ( 'NONE',  ( 8.000000000000000000, -16.92083251265322374, -4.460989585141144076 ) ) ;
#35466 = CARTESIAN_POINT ( 'NONE',  ( -37.46093750000000711, -114.9929510916434339, 14.11852480586264846 ) ) ;
#35467 = CARTESIAN_POINT ( 'NONE',  ( -42.49999999999999289, -25.98076211353322051, 84.99999999999992895 ) ) ;
#35468 = AXIS2_PLACEMENT_3D ( 'NONE', #29139, #7864, #7683 ) ;
#35469 = DIRECTION ( 'NONE',  ( 0.000000000000000000, 0.000000000000000000, 1.000000000000000000 ) ) ;
#35470 = EDGE_LOOP ( 'NONE', ( #927, #27569, #19591, #13821 ) ) ;
#35471 = CIRCLE ( 'NONE', #7283, 8.000000000000007105 ) ;
#35472 = CARTESIAN_POINT ( 'NONE',  ( 0.000000000000000000, 0.000000000000000000, 0.000000000000000000 ) ) ;
#35473 = DIRECTION ( 'NONE',  ( 0.000000000000000000, 0.000000000000000000, 1.000000000000000000 ) ) ;
#35474 = VERTEX_POINT ( 'NONE', #16725 ) ;
#35475 = AXIS2_PLACEMENT_3D ( 'NONE', #30542, #29848, #13975 ) ;
#35476 = CARTESIAN_POINT ( 'NONE',  ( -35.99386409314529800, -114.9929510916434339, 13.11852378322482515 ) ) ;
#35477 = ORIENTED_EDGE ( 'NONE', *, *, #664, .T. ) ;
#35478 = CARTESIAN_POINT ( 'NONE',  ( -37.88768952767750164, -115.9754527089670262, 4.972274454178448266 ) ) ;
#35479 = CARTESIAN_POINT ( 'NONE',  ( 8.000000000000000000, -16.59870953437682672, 10.45300502024378986 ) ) ;
#35480 = EDGE_CURVE ( 'NONE', #22703, #10949, #3475, .T. ) ;
#35481 = VECTOR ( 'NONE', #12886, 1000.000000000000000 ) ;
#35482 = ORIENTED_EDGE ( 'NONE', *, *, #10850, .T. ) ;
#35483 = ORIENTED_EDGE ( 'NONE', *, *, #19334, .T. ) ;
#35484 = DIRECTION ( 'NONE',  ( 0.000000000000000000, -1.000000000000000000, 0.000000000000000000 ) ) ;
#35485 = PRODUCT_RELATED_PRODUCT_CATEGORY ( 'part', '', ( #8910 ) ) ;
#35486 = PLANE ( 'NONE',  #5421 ) ;
#35487 = ADVANCED_FACE ( 'NONE', ( #27736 ), #13698, .T. ) ;
#35488 = ORIENTED_EDGE ( 'NONE', *, *, #11651, .F. ) ;
#35489 = CARTESIAN_POINT ( 'NONE',  ( -33.97545270896703329, -115.1833782841879810, 2.590225545821551734 ) ) ;
#35490 = CARTESIAN_POINT ( 'NONE',  ( -34.49999999999998579, -25.98076211353322051, 84.99999999999992895 ) ) ;
#35491 = AXIS2_PLACEMENT_3D ( 'NONE', #6349, #30497, #11225 ) ;
#35492 = CARTESIAN_POINT ( 'NONE',  ( 7.999999999999992895, 5.871425383722286284, -51.66745943012276854 ) ) ;
#35493 = VERTEX_POINT ( 'NONE', #19081 ) ;
#35494 = ORIENTED_EDGE ( 'NONE', *, *, #13687, .T. ) ;
#35495 = EDGE_CURVE ( 'NONE', #10255, #18652, #22438, .T. ) ;
#35496 = CARTESIAN_POINT ( 'NONE',  ( 0.000000000000000000, 0.000000000000000000, 0.000000000000000000 ) ) ;
#35497 = EDGE_CURVE ( 'NONE', #7838, #12939, #32774, .T. ) ;
#35498 = CIRCLE ( 'NONE', #25701, 47.49900000000001654 ) ;
#35499 = DIRECTION ( 'NONE',  ( 0.000000000000000000, 0.000000000000000000, -1.000000000000000000 ) ) ;
#35500 = ORIENTED_EDGE ( 'NONE', *, *, #3812, .T. ) ;
#35501 = ORIENTED_EDGE ( 'NONE', *, *, #7670, .T. ) ;
#35502 = CARTESIAN_POINT ( 'NONE',  ( -34.50000000000000000, -113.3474311500483935, -2.624782352598442614 ) ) ;
#35503 = AXIS2_PLACEMENT_3D ( 'NONE', #8503, #16408, #8669 ) ;
#35504 = VECTOR ( 'NONE', #9993, 1000.000000000000000 ) ;
#35505 = AXIS2_PLACEMENT_3D ( 'NONE', #15564, #29285, #7125 ) ;
#35506 = CYLINDRICAL_SURFACE ( 'NONE', #6407, 47.49900000000001654 ) ;
#35507 = ORIENTED_EDGE ( 'NONE', *, *, #15219, .F. ) ;
#35508 = CARTESIAN_POINT ( 'NONE',  ( 4.000000000000003553, 39.64889472655731595, 33.64468972902522381 ) ) ;
#35509 = ADVANCED_FACE ( 'NONE', ( #5596 ), #24677, .T. ) ;
#35510 = CARTESIAN_POINT ( 'NONE',  ( -36.01562499999997158, -113.9929510916434339, 14.11852480586265024 ) ) ;
#35511 = DIRECTION ( 'NONE',  ( 0.000000000000000000, 0.000000000000000000, 1.000000000000000000 ) ) ;
#35512 = DIRECTION ( 'NONE',  ( -1.000000000000000000, 0.000000000000000000, 0.000000000000000000 ) ) ;
#35513 = CARTESIAN_POINT ( 'NONE',  ( -38.00000000000000711, -113.9929510916434339, 12.50851088611646311 ) ) ;
#35514 = CARTESIAN_POINT ( 'NONE',  ( -35.50000000000000711, -114.3464919575557843, 9.568884482464163455 ) ) ;
#35515 = DIRECTION ( 'NONE',  ( 0.000000000000000000, 0.000000000000000000, 1.000000000000000000 ) ) ;
#35516 = DIRECTION ( 'NONE',  ( 1.000000000000000000, -4.336808689941997226E-15, -1.084202172485499306E-15 ) ) ;
#35517 = AXIS2_PLACEMENT_3D ( 'NONE', #15230, #15762, #10028 ) ;
#35518 = ORIENTED_EDGE ( 'NONE', *, *, #5691, .T. ) ;
#35519 = CARTESIAN_POINT ( 'NONE',  ( 8.000000000000000000, -18.48663108841356717, 4.615718728111985136 ) ) ;
#35520 = FACE_OUTER_BOUND ( 'NONE', #15469, .T. ) ;
#35521 = DIRECTION ( 'NONE',  ( -1.000000000000000000, 0.000000000000000000, -0.000000000000000000 ) ) ;
#35522 = VECTOR ( 'NONE', #32707, 1000.000000000000000 ) ;
#35523 = VECTOR ( 'NONE', #5598, 1000.000000000000000 ) ;
#35524 = EDGE_CURVE ( 'NONE', #352, #25438, #22313, .T. ) ;
#35525 = ORIENTED_EDGE ( 'NONE', *, *, #5734, .F. ) ;
#35526 = CIRCLE ( 'NONE', #7898, 8.000000000000008882 ) ;
#35527 = LINE ( 'NONE', #14061, #23364 ) ;
#35528 = VERTEX_POINT ( 'NONE', #19597 ) ;
#35529 = EDGE_CURVE ( 'NONE', #25030, #13426, #32789, .T. ) ;
#35530 = CARTESIAN_POINT ( 'NONE',  ( -35.50000000000000711, -116.0124910254613297, -0.6902086197697608894 ) ) ;
#35531 = FACE_OUTER_BOUND ( 'NONE', #31346, .T. ) ;
#35532 = ADVANCED_FACE ( 'NONE', ( #22484 ), #27902, .T. ) ;
#35533 = CARTESIAN_POINT ( 'NONE',  ( -36.25098837183129774, -113.3347980657956242, 5.816024454178450043 ) ) ;
#35534 = AXIS2_PLACEMENT_3D ( 'NONE', #443, #20036, #28340 ) ;
#35535 = CARTESIAN_POINT ( 'NONE',  ( -35.50000000000000711, -114.9929510916434339, 12.57451923796416082 ) ) ;
#35536 = CARTESIAN_POINT ( 'NONE',  ( 8.000000000000000000, -15.92965478239629817, 15.17386234660377831 ) ) ;
#35537 = ORIENTED_EDGE ( 'NONE', *, *, #25380, .T. ) ;
#35538 = DIRECTION ( 'NONE',  ( -1.000000000000000000, 0.000000000000000000, 0.000000000000000000 ) ) ;
#35539 = CARTESIAN_POINT ( 'NONE',  ( -35.50000000000000000, -113.0765974847181781, -2.624803185604914102 ) ) ;
#35540 = ORIENTED_EDGE ( 'NONE', *, *, #20991, .T. ) ;
#35541 = ORIENTED_EDGE ( 'NONE', *, *, #3533, .T. ) ;
#35542 = EDGE_CURVE ( 'NONE', #16232, #14694, #15520, .T. ) ;
#35543 = CARTESIAN_POINT ( 'NONE',  ( -36.23083527818512550, -116.0245472910329880, 3.284774454178449155 ) ) ;
#35544 = EDGE_CURVE ( 'NONE', #11231, #29049, #29357, .T. ) ;
#35545 = AXIS2_PLACEMENT_3D ( 'NONE', #20192, #31200, #32098 ) ;
#35546 = DIRECTION ( 'NONE',  ( 0.000000000000000000, -0.6427876096865456912, 0.7660444431189726844 ) ) ;
#35547 = VERTEX_POINT ( 'NONE', #12358 ) ;
#35548 = ORIENTED_EDGE ( 'NONE', *, *, #26743, .F. ) ;
#35549 = CARTESIAN_POINT ( 'NONE',  ( -34.50000000000000000, -115.0140978167138712, -0.6247823525985405357 ) ) ;
#35550 = DIRECTION ( 'NONE',  ( -1.000000000000000000, 0.000000000000000000, 0.000000000000000000 ) ) ;
#35551 = CIRCLE ( 'NONE', #29695, 14.00000000000000000 ) ;
#35552 = CIRCLE ( 'NONE', #21152, 15.49899999999998279 ) ;
#35553 = DIRECTION ( 'NONE',  ( 0.000000000000000000, 0.000000000000000000, 1.000000000000000000 ) ) ;
#35554 = CIRCLE ( 'NONE', #34386, 52.00000000000000711 ) ;
#35555 = LINE ( 'NONE', #27089, #27754 ) ;
#35556 = AXIS2_PLACEMENT_3D ( 'NONE', #20621, #25704, #17038 ) ;
#35557 = CARTESIAN_POINT ( 'NONE',  ( -35.50000000000000000, -113.9929510916434339, 12.60752341388803721 ) ) ;
#35558 = DIRECTION ( 'NONE',  ( 0.000000000000000000, -0.9048270524660146918, -0.4257792915650830956 ) ) ;
#35559 = LINE ( 'NONE', #24565, #27448 ) ;
#35560 = CIRCLE ( 'NONE', #19420, 7.999999999999992895 ) ;
#35561 = CARTESIAN_POINT ( 'NONE',  ( -34.50000000000000000, -112.0140978167138712, 0.5627176474015717078 ) ) ;
#35562 = CARTESIAN_POINT ( 'NONE',  ( -35.51674767832922441, -115.9929510916434481, 14.04194344061634325 ) ) ;
#35563 = DIRECTION ( 'NONE',  ( -1.000000000000000000, 0.000000000000000000, -0.000000000000000000 ) ) ;
#35564 = FACE_OUTER_BOUND ( 'NONE', #4902, .T. ) ;
#35565 = ORIENTED_EDGE ( 'NONE', *, *, #10018, .T. ) ;
#35566 = CARTESIAN_POINT ( 'NONE',  ( -37.80727372874345349, -115.9929510916434481, 13.01835785830664705 ) ) ;
#35567 = CARTESIAN_POINT ( 'NONE',  ( 7.999999999999992895, -46.11014828289849277, 9.022736828080537563 ) ) ;
#35568 = SURFACE_STYLE_FILL_AREA ( #16258 ) ;
#35569 = CARTESIAN_POINT ( 'NONE',  ( 0.000000000000000000, 46.77034588191337150, -22.72740077717178053 ) ) ;
#35570 = DIRECTION ( 'NONE',  ( 0.000000000000000000, -0.3681245526846853022, 0.9297764858882484607 ) ) ;
#35571 = EDGE_CURVE ( 'NONE', #16323, #32690, #4104, .T. ) ;
#35572 = ORIENTED_EDGE ( 'NONE', *, *, #20121, .F. ) ;
#35573 = LINE ( 'NONE', #13417, #1541 ) ;
#35574 = DIRECTION ( 'NONE',  ( 1.000000000000000000, -0.000000000000000000, -0.000000000000000000 ) ) ;
#35575 = EDGE_CURVE ( 'NONE', #30211, #8680, #23157, .T. ) ;
#35576 = DIRECTION ( 'NONE',  ( -1.000000000000000000, 0.000000000000000000, 0.000000000000000000 ) ) ;
#35577 = DIRECTION ( 'NONE',  ( 0.000000000000000000, 0.000000000000000000, 1.000000000000000000 ) ) ;
#35578 = AXIS2_PLACEMENT_3D ( 'NONE', #24475, #26828, #35293 ) ;
#35579 = FACE_OUTER_BOUND ( 'NONE', #18421, .T. ) ;
#35580 = CARTESIAN_POINT ( 'NONE',  ( 8.000000000000000000, -14.71414642875963708, 9.471478019455089381 ) ) ;
#35581 = EDGE_LOOP ( 'NONE', ( #11927, #11725, #9899, #13830 ) ) ;
#35582 = EDGE_LOOP ( 'NONE', ( #25291, #31226, #19992, #13934 ) ) ;
#35583 = CIRCLE ( 'NONE', #25211, 4.800000000000005151 ) ;
#35584 = DIRECTION ( 'NONE',  ( 0.000000000000000000, 0.000000000000000000, 1.000000000000000000 ) ) ;
#35585 = DIRECTION ( 'NONE',  ( -1.000000000000000000, 0.000000000000000000, -0.000000000000000000 ) ) ;
#35586 = DIRECTION ( 'NONE',  ( 0.000000000000000000, -1.000000000000000000, 0.000000000000000000 ) ) ;
#35587 = VERTEX_POINT ( 'NONE', #26407 ) ;
#35588 = CARTESIAN_POINT ( 'NONE',  ( -38.97545270896704039, -114.8876895276775087, 9.152725545821555286 ) ) ;
#35589 = ORIENTED_EDGE ( 'NONE', *, *, #7535, .T. ) ;
#35590 = VERTEX_POINT ( 'NONE', #15398 ) ;
#35591 = VERTEX_POINT ( 'NONE', #20794 ) ;
#35592 = DIRECTION ( 'NONE',  ( -1.000000000000000000, 0.000000000000000000, 0.000000000000000000 ) ) ;
#35593 = CARTESIAN_POINT ( 'NONE',  ( 0.000000000000000000, 0.000000000000000000, -0.7999999999999951594 ) ) ;
#35594 = VERTEX_POINT ( 'NONE', #3924 ) ;
#35595 = CARTESIAN_POINT ( 'NONE',  ( 4.000000000000003553, 31.08872492060014991, -41.68322423723069647 ) ) ;
#35596 = DIRECTION ( 'NONE',  ( 0.000000000000000000, 0.7535859266250380939, 0.6573494133204066392 ) ) ;
#35597 = CARTESIAN_POINT ( 'NONE',  ( 7.999999999999992895, 0.000000000000000000, 0.000000000000000000 ) ) ;
#35598 = CARTESIAN_POINT ( 'NONE',  ( 8.000000000000000000, 0.000000000000000000, 0.000000000000000000 ) ) ;
#35599 = DIRECTION ( 'NONE',  ( -1.000000000000000000, 0.000000000000000000, 0.000000000000000000 ) ) ;
#35600 = AXIS2_PLACEMENT_3D ( 'NONE', #32299, #16424, #2428 ) ;
#35601 = DIRECTION ( 'NONE',  ( 1.000000000000000000, 0.000000000000000000, -0.000000000000000000 ) ) ;
#35602 = CARTESIAN_POINT ( 'NONE',  ( -38.98797722933581866, -115.9929510916434481, 12.81430620224974959 ) ) ;
#35603 = CARTESIAN_POINT ( 'NONE',  ( 0.000000000000000000, 0.000000000000000000, 55.00000000000000000 ) ) ;
#35604 = FACE_OUTER_BOUND ( 'NONE', #33300, .T. ) ;
#35605 = DIRECTION ( 'NONE',  ( 0.000000000000000000, -6.982962677686266711E-15, 1.000000000000000000 ) ) ;
#35606 = DIRECTION ( 'NONE',  ( 0.000000000000000000, 0.000000000000000000, -1.000000000000000000 ) ) ;
#35607 = ADVANCED_FACE ( 'NONE', ( #31977 ), #12903, .T. ) ;
#35608 = CARTESIAN_POINT ( 'NONE',  ( 50.00005079999998969, 0.000000000000000000, 0.000000000000000000 ) ) ;
#35609 = PRESENTATION_STYLE_ASSIGNMENT (( #25151 ) ) ;
#35610 = ORIENTED_EDGE ( 'NONE', *, *, #4150, .T. ) ;
#35611 = CARTESIAN_POINT ( 'NONE',  ( -37.35495115944176803, -115.0245472910329880, 4.465225545821550845 ) ) ;
#35612 = LINE ( 'NONE', #25155, #21554 ) ;
#35613 = CARTESIAN_POINT ( 'NONE',  ( 8.000000000000000000, 11.19999565274265230, -10.71350075272062874 ) ) ;
#35614 = CARTESIAN_POINT ( 'NONE',  ( 8.000000000000000000, -3.678165988948685516, 15.05623113391066070 ) ) ;
#35615 = ORIENTED_EDGE ( 'NONE', *, *, #25116, .F. ) ;
#35616 = NEXT_ASSEMBLY_USAGE_OCCURRENCE ( 'NAUO1', ' ', ' ', #5763, #8382, $ ) ;
#35617 = NEXT_ASSEMBLY_USAGE_OCCURRENCE ( 'NAUO2', ' ', ' ', #5763, #33925, $ ) ;
#35618 = NEXT_ASSEMBLY_USAGE_OCCURRENCE ( 'NAUO3', ' ', ' ', #5763, #912, $ ) ;
#35619 = NEXT_ASSEMBLY_USAGE_OCCURRENCE ( 'NAUO4', ' ', ' ', #5763, #30188, $ ) ;
#35620 = NEXT_ASSEMBLY_USAGE_OCCURRENCE ( 'NAUO5', ' ', ' ', #5763, #22682, $ ) ;
#35621 = NEXT_ASSEMBLY_USAGE_OCCURRENCE ( 'NAUO6', ' ', ' ', #5763, #5129, $ ) ;
#35622 = NEXT_ASSEMBLY_USAGE_OCCURRENCE ( 'NAUO7', ' ', ' ', #5763, #18964, $ ) ;
#35623 = NEXT_ASSEMBLY_USAGE_OCCURRENCE ( 'NAUO8', ' ', ' ', #5763, #34383, $ ) ;
#35624 = NEXT_ASSEMBLY_USAGE_OCCURRENCE ( 'NAUO9', ' ', ' ', #5763, #32378, $ ) ;
#35625 = NEXT_ASSEMBLY_USAGE_OCCURRENCE ( 'NAUO10', ' ', ' ', #5763, #21149, $ ) ;
#35626 = NEXT_ASSEMBLY_USAGE_OCCURRENCE ( 'NAUO11', ' ', ' ', #5763, #21149, $ ) ;
#35627 = NEXT_ASSEMBLY_USAGE_OCCURRENCE ( 'NAUO12', ' ', ' ', #5763, #21149, $ ) ;
#35628 = NEXT_ASSEMBLY_USAGE_OCCURRENCE ( 'NAUO13', ' ', ' ', #5763, #21149, $ ) ;
#35629 = NEXT_ASSEMBLY_USAGE_OCCURRENCE ( 'NAUO14', ' ', ' ', #5763, #24258, $ ) ;
#35630 = NEXT_ASSEMBLY_USAGE_OCCURRENCE ( 'NAUO15', ' ', ' ', #5763, #21149, $ ) ;
#35631 = NEXT_ASSEMBLY_USAGE_OCCURRENCE ( 'NAUO16', ' ', ' ', #5763, #21149, $ ) ;
#35632 = NEXT_ASSEMBLY_USAGE_OCCURRENCE ( 'NAUO17', ' ', ' ', #5763, #8827, $ ) ;
#35633 = NEXT_ASSEMBLY_USAGE_OCCURRENCE ( 'NAUO18', ' ', ' ', #5763, #20037, $ ) ;
#35634 = NEXT_ASSEMBLY_USAGE_OCCURRENCE ( 'NAUO19', ' ', ' ', #5763, #6847, $ ) ;
#35635 = NEXT_ASSEMBLY_USAGE_OCCURRENCE ( 'NAUO20', ' ', ' ', #5763, #3129, $ ) ;
#35636 = NEXT_ASSEMBLY_USAGE_OCCURRENCE ( 'NAUO21', ' ', ' ', #5763, #23811, $ ) ;
#35637 = NEXT_ASSEMBLY_USAGE_OCCURRENCE ( 'NAUO22', ' ', ' ', #5763, #23811, $ ) ;
#35638 = NEXT_ASSEMBLY_USAGE_OCCURRENCE ( 'NAUO23', ' ', ' ', #5763, #23811, $ ) ;
#35639 = NEXT_ASSEMBLY_USAGE_OCCURRENCE ( 'NAUO24', ' ', ' ', #5763, #23811, $ ) ;
#35640 = NEXT_ASSEMBLY_USAGE_OCCURRENCE ( 'NAUO25', ' ', ' ', #5763, #23811, $ ) ;
#35641 = NEXT_ASSEMBLY_USAGE_OCCURRENCE ( 'NAUO26', ' ', ' ', #5763, #23811, $ ) ;
#35642 = NEXT_ASSEMBLY_USAGE_OCCURRENCE ( 'NAUO27', ' ', ' ', #5763, #23811, $ ) ;
#35643 = NEXT_ASSEMBLY_USAGE_OCCURRENCE ( 'NAUO28', ' ', ' ', #5763, #23811, $ ) ;
#35644 = NEXT_ASSEMBLY_USAGE_OCCURRENCE ( 'NAUO29', ' ', ' ', #5763, #23811, $ ) ;
#35645 = NEXT_ASSEMBLY_USAGE_OCCURRENCE ( 'NAUO30', ' ', ' ', #5763, #23811, $ ) ;
#35646 = NEXT_ASSEMBLY_USAGE_OCCURRENCE ( 'NAUO31', ' ', ' ', #5763, #23811, $ ) ;
#35647 = NEXT_ASSEMBLY_USAGE_OCCURRENCE ( 'NAUO32', ' ', ' ', #5763, #23811, $ ) ;
#35648 = NEXT_ASSEMBLY_USAGE_OCCURRENCE ( 'NAUO33', ' ', ' ', #5763, #23811, $ ) ;
#35649 = NEXT_ASSEMBLY_USAGE_OCCURRENCE ( 'NAUO34', ' ', ' ', #5763, #23811, $ ) ;
#35650 = NEXT_ASSEMBLY_USAGE_OCCURRENCE ( 'NAUO35', ' ', ' ', #5763, #23811, $ ) ;
#35651 = NEXT_ASSEMBLY_USAGE_OCCURRENCE ( 'NAUO36', ' ', ' ', #5763, #27561, $ ) ;
#35652 = NEXT_ASSEMBLY_USAGE_OCCURRENCE ( 'NAUO37', ' ', ' ', #5763, #23811, $ ) ;
#35653 = NEXT_ASSEMBLY_USAGE_OCCURRENCE ( 'NAUO38', ' ', ' ', #5763, #23811, $ ) ;
#35654 = NEXT_ASSEMBLY_USAGE_OCCURRENCE ( 'NAUO39', ' ', ' ', #5763, #23811, $ ) ;
#35655 = NEXT_ASSEMBLY_USAGE_OCCURRENCE ( 'NAUO40', ' ', ' ', #5763, #23811, $ ) ;
ENDSEC;
END-ISO-10303-21;
